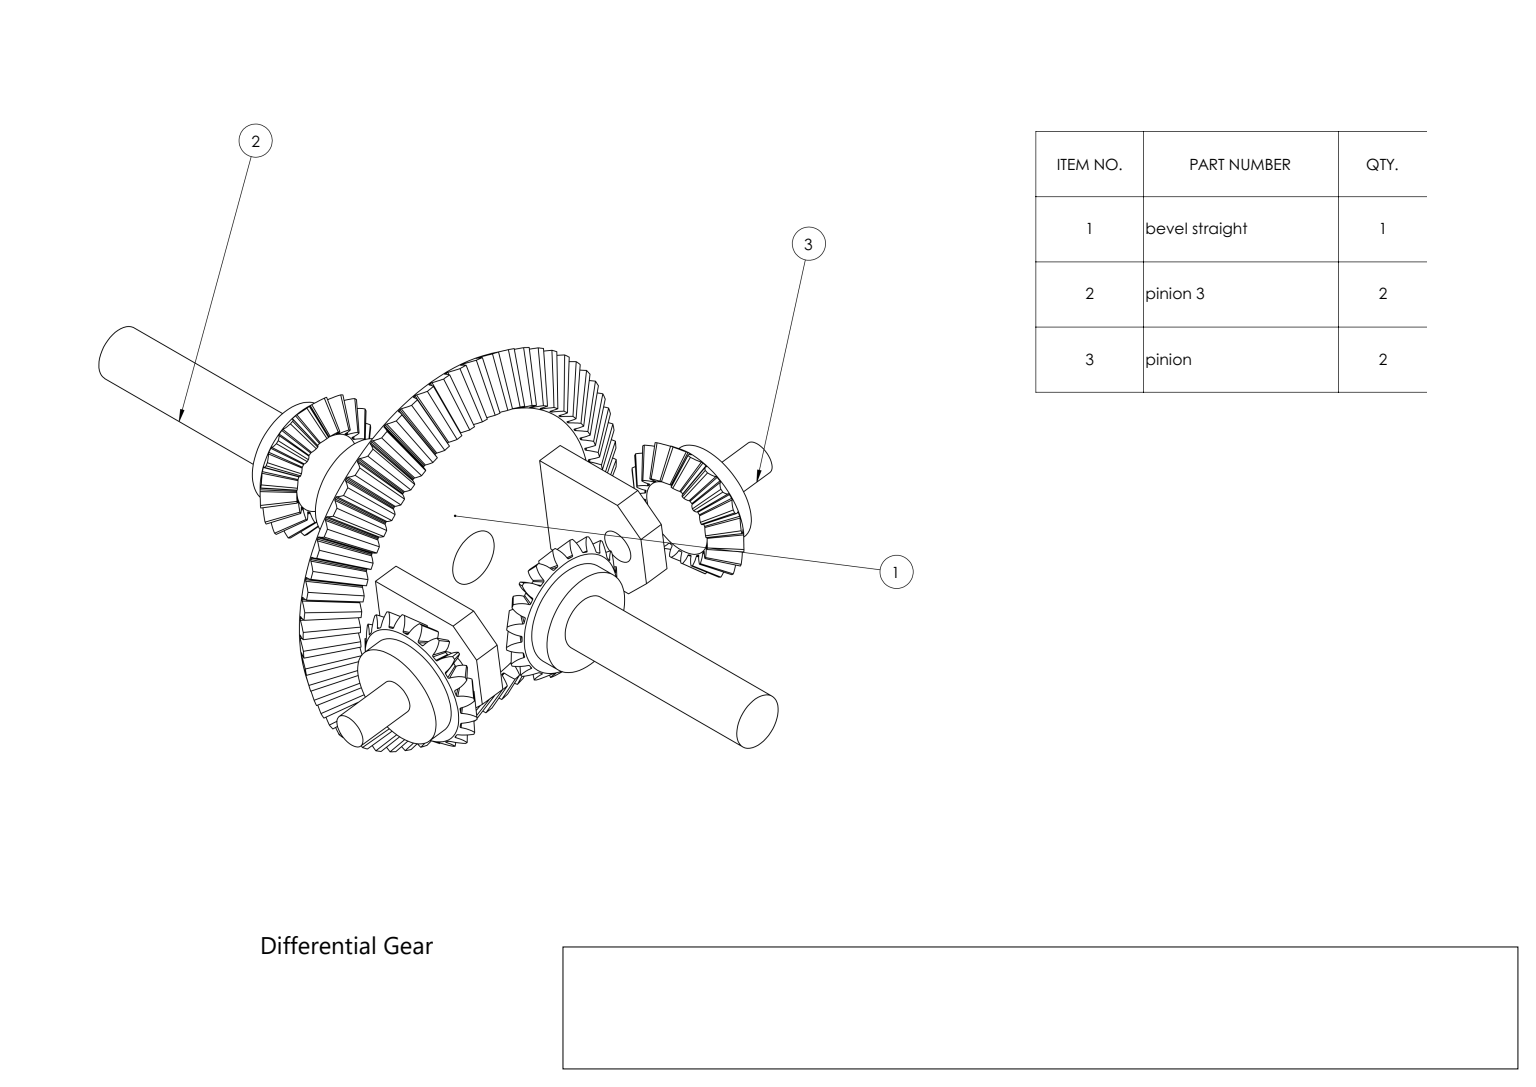
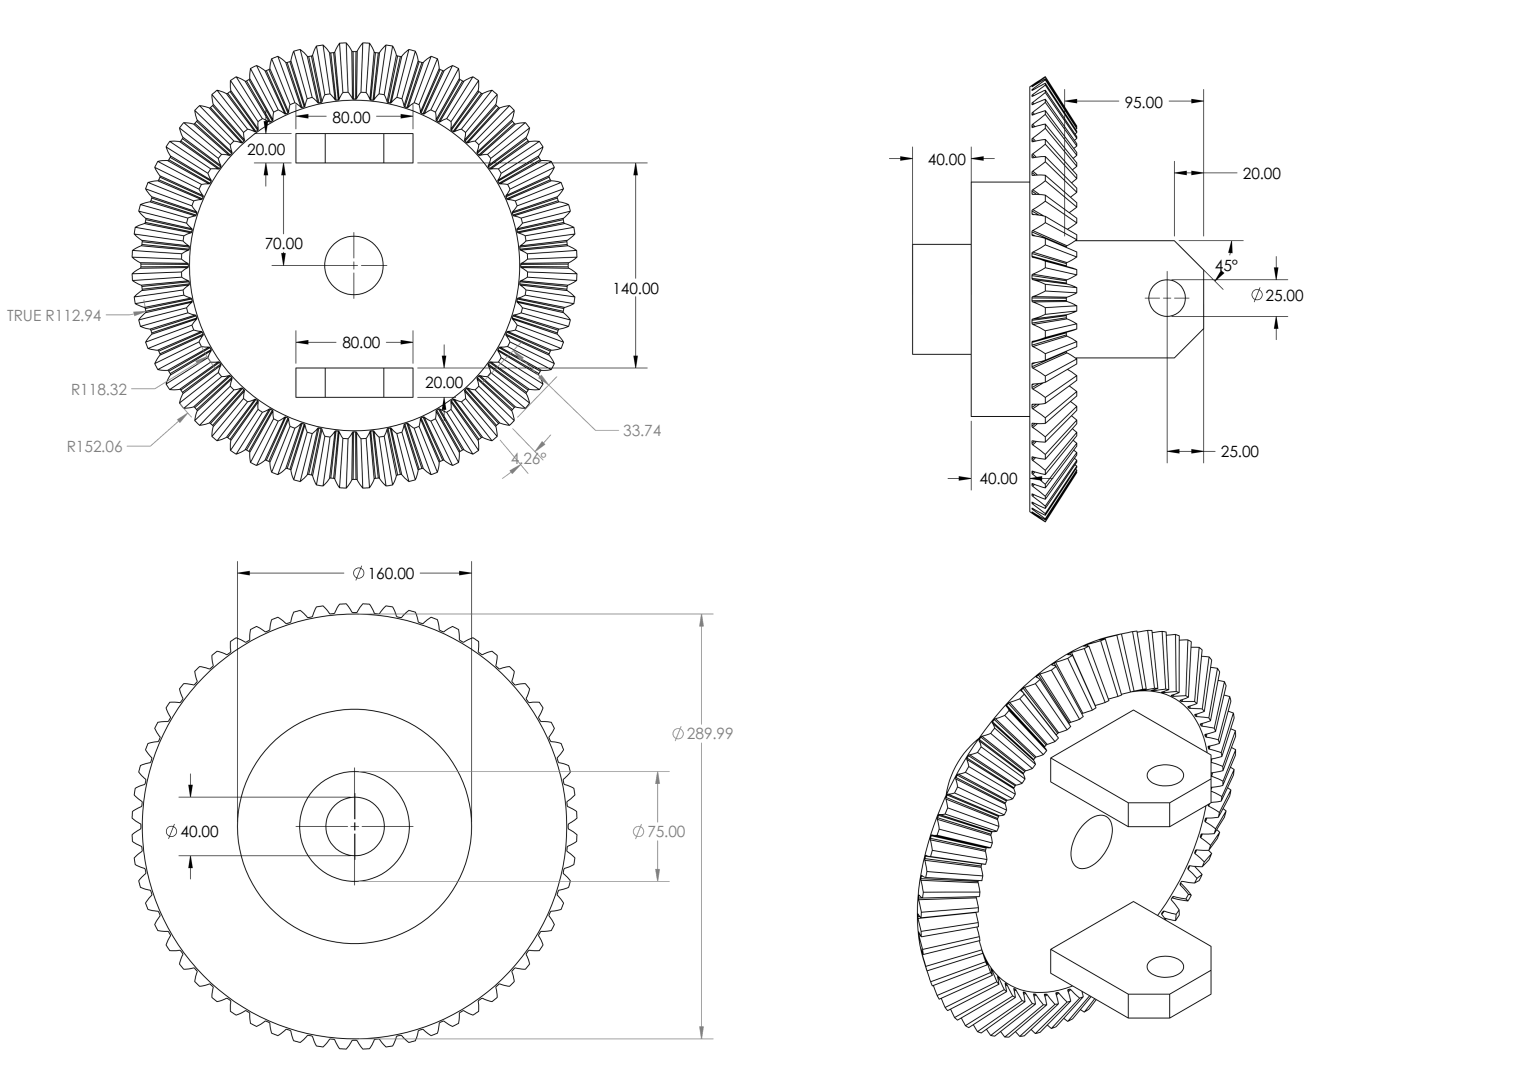
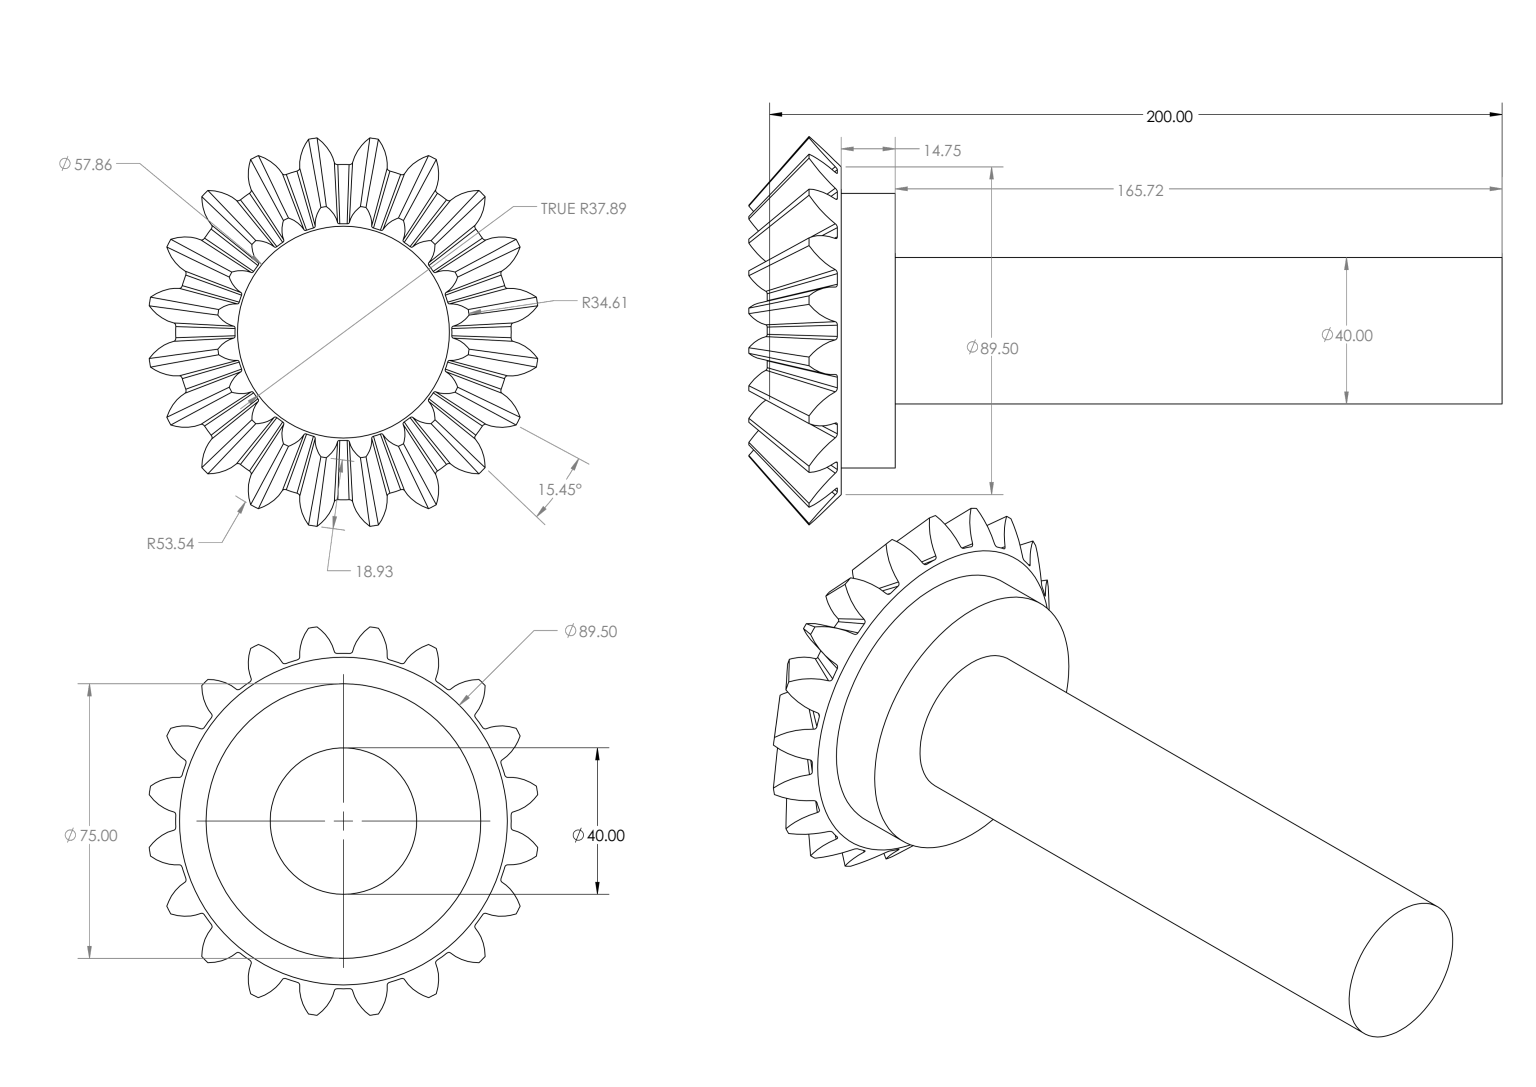
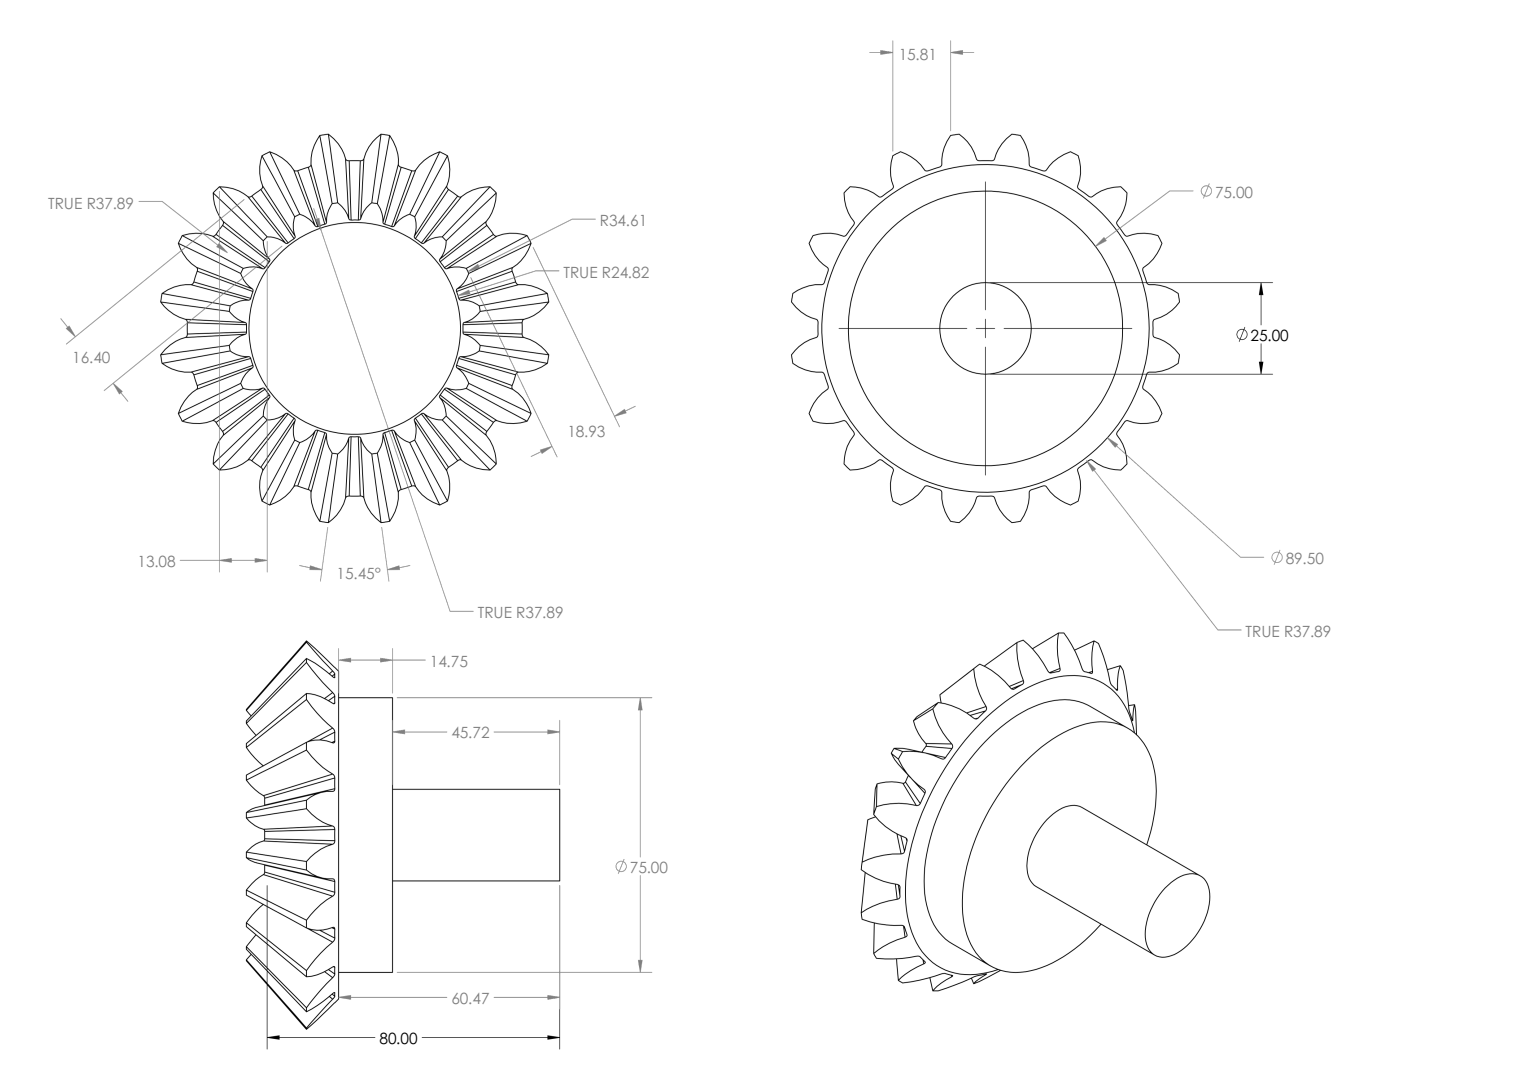
ISO-10303-21;
HEADER;
FILE_DESCRIPTION (('STEP AP214'),
    '1' );
FILE_NAME ('MAT-025',
    '2026-10-27T17:59:55',
    ( '' ),
    ( '' ),
    'SwSTEP 2.0',
    'SolidWorks 2025',
    '' );
FILE_SCHEMA (( 'AUTOMOTIVE_DESIGN' ));
ENDSEC;

DATA;
#1 = EDGE_LOOP ( 'NONE', ( #10472, #7018, #25272, #25137 ) ) ;
#2 = CARTESIAN_POINT ( 'NONE',  ( 1.833838850855486591, 72.47782099564645364, 125.7132320915350618 ) ) ;
#3 = CARTESIAN_POINT ( 'NONE',  ( -25.21435515916043713, -23.92354251275954979, -25.00736669481013053 ) ) ;
#4 = ORIENTED_EDGE ( 'NONE', *, *, #19841, .F. ) ;
#5 = CARTESIAN_POINT ( 'NONE',  ( 26.11404676487259024, 103.8885755249575453, -45.01677474591305383 ) ) ;
#6 = DIRECTION ( 'NONE',  ( -1.000000000000000000, 6.938893903907226837E-18, -1.734723475976806709E-18 ) ) ;
#7 = CARTESIAN_POINT ( 'NONE',  ( 1.833838850855486813, -44.75675607098831676, -138.0350826608191994 ) ) ;
#8 = LINE ( 'NONE', #19590, #21176 ) ;
#9 = CARTESIAN_POINT ( 'NONE',  ( -7.711401346138400115, 25.75361633141491424, -45.70592430511727144 ) ) ;
#10 = CARTESIAN_POINT ( 'NONE',  ( 1.833485406944043827, 96.69979900902318093, -108.1939177044916107 ) ) ;
#11 = CARTESIAN_POINT ( 'NONE',  ( -1.464342487929861214, -35.90631960086394514, 29.09292098541700611 ) ) ;
#12 = DIRECTION ( 'NONE',  ( -1.000000000000000000, -0.000000000000000000, -0.000000000000000000 ) ) ;
#13 = CARTESIAN_POINT ( 'NONE',  ( 1.834118845439484335, 107.9567937753806035, -96.96525081349894037 ) ) ;
#14 = CARTESIAN_POINT ( 'NONE',  ( -12.82751273423877514, -44.03362901246993744, 21.21958768041844579 ) ) ;
#15 = CARTESIAN_POINT ( 'NONE',  ( 2.433796855181219243, -43.58222566461740399, 138.8296532063086772 ) ) ;
#16 = CARTESIAN_POINT ( 'NONE',  ( 109.1721716018069657, 0.01157047143379281995, 0.01254847260354831351 ) ) ;
#17 = ORIENTED_EDGE ( 'NONE', *, *, #19645, .F. ) ;
#18 = EDGE_CURVE ( 'NONE', #18004, #25022, #27276, .T. ) ;
#19 = VERTEX_POINT ( 'NONE', #7434 ) ;
#20 = CARTESIAN_POINT ( 'NONE',  ( 1.833206308920067640, -126.0392061186627330, 71.90885838897354176 ) ) ;
#21 = CONICAL_SURFACE ( 'NONE', #3715, 34.60786435723138510, 0.8559913436420825139 ) ;
#22 = CARTESIAN_POINT ( 'NONE',  ( 32.73300124599738581, -32.68291970228155918, -113.0038235389605461 ) ) ;
#23 = VECTOR ( 'NONE', #27500, 1000.000000000000000 ) ;
#24 = EDGE_LOOP ( 'NONE', ( #16873, #10935, #10142, #25938 ) ) ;
#25 = VECTOR ( 'NONE', #23229, 1000.000000000000000 ) ;
#26 = VERTEX_POINT ( 'NONE', #9734 ) ;
#27 = EDGE_CURVE ( 'NONE', #15045, #24750, #18584, .T. ) ;
#28 = ORIENTED_EDGE ( 'NONE', *, *, #4351, .F. ) ;
#30 = AXIS2_PLACEMENT_3D ( 'NONE', #2388, #25118, #7714 ) ;
#29 =( BOUNDED_SURFACE ( )  B_SPLINE_SURFACE ( 3, 1, ( 
 ( #18833, #10616 ),
 ( #3858, #14509 ),
 ( #27599, #23743 ),
 ( #7922, #12623 ) ),
 .UNSPECIFIED., .F., .F., .F. ) 
 B_SPLINE_SURFACE_WITH_KNOTS ( ( 4, 4 ),
 ( 2, 2 ),
 ( 0.000000000000000000, 1.000000000000000000 ),
 ( 0.000000000000000000, 1.000000000000000000 ),
 .UNSPECIFIED. ) 
 GEOMETRIC_REPRESENTATION_ITEM ( )  RATIONAL_B_SPLINE_SURFACE ( (
 ( 1.000000000000000000, 1.000000000000000000),
 ( 0.9934239774497837239, 0.8357310067453919133),
 ( 0.9934239774497837239, 0.8357310067453919133),
 ( 1.000000000000000000, 1.000000000000000000) ) ) 
 REPRESENTATION_ITEM ( '' )  SURFACE ( )  );
#31 = EDGE_CURVE ( 'NONE', #25314, #21344, #6914, .T. ) ;
#32 = PRODUCT ( 'bevel straight', 'bevel straight', '', ( #7748 ) ) ;
#33 = CARTESIAN_POINT ( 'NONE',  ( 1.833838848569445235, 138.0625820091624689, 44.67212175381883554 ) ) ;
#34 = CARTESIAN_POINT ( 'NONE',  ( -1.019300379054419947, -44.15350047934390432, 12.21833869579511500 ) ) ;
#35 = B_SPLINE_CURVE_WITH_KNOTS ( 'NONE', 3,
 ( #6398, #19625, #8695, #17458, #4374, #21935, #7700, #20914, #16456, #5081 ),
 .UNSPECIFIED., .F., .F.,
 ( 4, 2, 2, 2, 4 ),
 ( 0.000000000000000000, 0.0003346267210630939765, 0.0006692534421261879529, 0.001003880163189281929, 0.001338506884252375906 ),
 .UNSPECIFIED. ) ;
#36 = CARTESIAN_POINT ( 'NONE',  ( -1.058197053496162887, -25.48582931365496762, -38.06270006878843759 ) ) ;
#37 = CARTESIAN_POINT ( 'NONE',  ( -20.57838717382308147, -16.28767523336102130, 25.16001208503123365 ) ) ;
#38 = CARTESIAN_POINT ( 'NONE',  ( 1.832998868059858122, 117.7096351258399238, -84.86110816369483700 ) ) ;
#39 = VECTOR ( 'NONE', #10071, 1000.000000000000000 ) ;
#40 = AXIS2_PLACEMENT_3D ( 'NONE', #19702, #25783, #12945 ) ;
#41 = CARTESIAN_POINT ( 'NONE',  ( -22.34422965417124374, 26.20925041532892763, 27.39717383755251490 ) ) ;
#42 = VECTOR ( 'NONE', #28114, 1000.000000000000000 ) ;
#43 = CARTESIAN_POINT ( 'NONE',  ( 25.64692872815576408, -110.5102270591924309, 23.16082795281220186 ) ) ;
#44 = CARTESIAN_POINT ( 'NONE',  ( -8.259864102781671491, -47.98931516265581365, 22.52209142944983711 ) ) ;
#45 = CARTESIAN_POINT ( 'NONE',  ( -1.050230346682696103, 37.05264119692688496, -26.91946103437118509 ) ) ;
#46 = CARTESIAN_POINT ( 'NONE',  ( 28.43349137099831836, 89.57679848841924297, -86.10800331998703427 ) ) ;
#47 = VECTOR ( 'NONE', #2248, 999.9999999999998863 ) ;
#48 = ORIENTED_EDGE ( 'NONE', *, *, #19991, .T. ) ;
#49 = ORIENTED_EDGE ( 'NONE', *, *, #17339, .T. ) ;
#51 = CARTESIAN_POINT ( 'NONE',  ( 5.340103556456315737, 133.7487107983443195, 62.06990747183722590 ) ) ;
#50 = DIRECTION ( 'NONE',  ( 0.000000000000000000, 5.223019709707975211E-21, -1.000000000000000000 ) ) ;
#52 = CARTESIAN_POINT ( 'NONE',  ( 2.433796855181233454, 109.1007109081226076, 96.28145139437721411 ) ) ;
#53 = CARTESIAN_POINT ( 'NONE',  ( 55.49584447822657296, -36.04376091928499903, -62.96491934286030556 ) ) ;
#54 = CARTESIAN_POINT ( 'NONE',  ( 32.73300124599741423, -75.82012867748416340, -89.94078864464141532 ) ) ;
#55 = CARTESIAN_POINT ( 'NONE',  ( -8.786685647604890903, -52.67761315067293282, -9.545808661480407409 ) ) ;
#56 = EDGE_LOOP ( 'NONE', ( #3504, #20915, #25986, #8058 ) ) ;
#57 = FACE_OUTER_BOUND ( 'NONE', #2614, .T. ) ;
#58 = EDGE_CURVE ( 'NONE', #28126, #17270, #1739, .T. ) ;
#59 = EDGE_LOOP ( 'NONE', ( #16364, #16288, #13278, #22767 ) ) ;
#60 = CARTESIAN_POINT ( 'NONE',  ( 2.108393763691174261, -144.3574619851891327, -16.46048390411948148 ) ) ;
#61 = FACE_OUTER_BOUND ( 'NONE', #13204, .T. ) ;
#62 = EDGE_LOOP ( 'NONE', ( #22452, #15366, #26764, #26750 ) ) ;
#63 = ORIENTED_EDGE ( 'NONE', *, *, #20098, .F. ) ;
#64 = ADVANCED_FACE ( 'NONE', ( #16053 ), #6020, .F. ) ;
#65 = CARTESIAN_POINT ( 'NONE',  ( 1.834118845439484335, 0.1779704863070283027, 145.1099497418795750 ) ) ;
#67 = ORIENTED_EDGE ( 'NONE', *, *, #11570, .T. ) ;
#66 = B_SPLINE_CURVE_WITH_KNOTS ( 'NONE', 3,
 ( #19256, #1821, #17232, #21839, #4133, #8326, #19665, #8599, #6307, #27897 ),
 .UNSPECIFIED., .F., .F.,
 ( 4, 3, 3, 4 ),
 ( 3.925231146709437917E-17, 0.0002669559177086131842, 0.0005339118354151096806, 0.001067817517169159696 ),
 .UNSPECIFIED. ) ;
#68 = CARTESIAN_POINT ( 'NONE',  ( 6.224689322667647851, -43.30635742325475945, 141.5842213414011894 ) ) ;
#69 = ORIENTED_EDGE ( 'NONE', *, *, #25818, .T. ) ;
#70 = EDGE_CURVE ( 'NONE', #24626, #27978, #23754, .T. ) ;
#71 = VECTOR ( 'NONE', #18224, 1000.000000000000114 ) ;
#72 =( GEOMETRIC_REPRESENTATION_CONTEXT ( 3 ) GLOBAL_UNCERTAINTY_ASSIGNED_CONTEXT ( ( #16000 ) ) GLOBAL_UNIT_ASSIGNED_CONTEXT ( ( #25277, #3392, #1644 ) ) REPRESENTATION_CONTEXT ( 'NONE', 'WORKASPACE' ) );
#73 = CARTESIAN_POINT ( 'NONE',  ( 1.833485406944057594, 97.49333871408690300, 107.4794113447412940 ) ) ;
#74 = EDGE_CURVE ( 'NONE', #7427, #22997, #15851, .T. ) ;
#75 = VECTOR ( 'NONE', #20368, 1000.000000000000000 ) ;
#76 = ORIENTED_EDGE ( 'NONE', *, *, #10432, .T. ) ;
#77 =( BOUNDED_SURFACE ( )  B_SPLINE_SURFACE ( 3, 1, ( 
 ( #18368, #537 ),
 ( #2696, #7179 ),
 ( #16223, #3130 ),
 ( #25029, #14055 ) ),
 .UNSPECIFIED., .F., .F., .F. ) 
 B_SPLINE_SURFACE_WITH_KNOTS ( ( 4, 4 ),
 ( 2, 2 ),
 ( 0.000000000000000000, 1.000000000000000000 ),
 ( 0.000000000000000000, 1.000000000000000000 ),
 .UNSPECIFIED. ) 
 GEOMETRIC_REPRESENTATION_ITEM ( )  RATIONAL_B_SPLINE_SURFACE ( (
 ( 1.000000000000000000, 1.000000000000000000),
 ( 0.7789835883360576307, 0.9689951854195403280),
 ( 0.7789835883360576307, 0.9689951854195403280),
 ( 1.000000000000000000, 1.000000000000000000) ) ) 
 REPRESENTATION_ITEM ( '' )  SURFACE ( )  );
#78 = CARTESIAN_POINT ( 'NONE',  ( 32.73300124599738581, -55.46353551261936587, -103.7392577722181812 ) ) ;
#79 = CARTESIAN_POINT ( 'NONE',  ( 2.430230287190589422, 13.76600171652836302, -144.8619874886005334 ) ) ;
#80 = CARTESIAN_POINT ( 'NONE',  ( 25.86096068574580897, 55.66087367585407009, 98.40249579084530751 ) ) ;
#81 = CARTESIAN_POINT ( 'NONE',  ( 10.93730112725972070, -4.928439153521261495, 151.0983828010090804 ) ) ;
#82 = B_SPLINE_CURVE_WITH_KNOTS ( 'NONE', 3,
 ( #16407, #22468, #25063, #2733, #11511, #18128 ),
 .UNSPECIFIED., .F., .F.,
 ( 4, 2, 4 ),
 ( 4.906538933386797396E-18, 0.0004335151646191543395, 0.0008670303292383036917 ),
 .UNSPECIFIED. ) ;
#83 = CARTESIAN_POINT ( 'NONE',  ( -1.583189561560256253, 11.94859433442902130, -44.83405390829675952 ) ) ;
#84 = FACE_OUTER_BOUND ( 'NONE', #26105, .T. ) ;
#85 = B_SPLINE_CURVE_WITH_KNOTS ( 'NONE', 3,
 ( #11291, #16435, #20350, #18180, #12122, #2499 ),
 .UNSPECIFIED., .F., .F.,
 ( 4, 2, 4 ),
 ( 3.525929482785130599E-16, 0.003576372551511158761, 0.007152745103021965374 ),
 .UNSPECIFIED. ) ;
#86 = CARTESIAN_POINT ( 'NONE',  ( 25.64681081121879203, -56.81519825470687834, -97.57530875170664331 ) ) ;
#87 = CARTESIAN_POINT ( 'NONE',  ( -24.53237795827004319, 33.71192251888839309, -3.868415699415555853 ) ) ;
#88 = CARTESIAN_POINT ( 'NONE',  ( 1.833206310202335487, 125.2945016693821572, -73.19872434058655131 ) ) ;
#89 = CARTESIAN_POINT ( 'NONE',  ( 28.37644542392839853, 115.1790646972555550, -46.84227702240664826 ) ) ;
#90 = DIRECTION ( 'NONE',  ( -0.5946245182733607137, 0.2512550613902174712, 0.7637359336799413034 ) ) ;
#91 = ORIENTED_EDGE ( 'NONE', *, *, #18115, .F. ) ;
#92 = CONICAL_SURFACE ( 'NONE', #10236, 117.6351876552689504, 0.9945805576725580410 ) ;
#93 = CARTESIAN_POINT ( 'NONE',  ( -25.21435515916043713, -34.05351380035337883, -6.169479169075319014 ) ) ;
#94 = CARTESIAN_POINT ( 'NONE',  ( 55.79472521941428198, -54.55111121764050353, -48.13855120843939517 ) ) ;
#95 = CARTESIAN_POINT ( 'NONE',  ( 30.58324630866339433, 67.85993782330898227, -100.1119227962713580 ) ) ;
#96 = EDGE_CURVE ( 'NONE', #11003, #17556, #6371, .T. ) ;
#97 = EDGE_LOOP ( 'NONE', ( #15926, #16768, #23788, #24002 ) ) ;
#98 = CARTESIAN_POINT ( 'NONE',  ( -55.24390624410018802, 0.009374879212967415429, 0.004572280736702902422 ) ) ;
#99 = EDGE_CURVE ( 'NONE', #10555, #9765, #28256, .T. ) ;
#100 = CARTESIAN_POINT ( 'NONE',  ( 25.64681081121879203, 84.18689316040048709, 75.24277141833519522 ) ) ;
#101 = ORIENTED_EDGE ( 'NONE', *, *, #24597, .T. ) ;
#102 = CARTESIAN_POINT ( 'NONE',  ( 25.64708228042119131, -112.9112740241347410, -0.03938584558111280637 ) ) ;
#103 = CARTESIAN_POINT ( 'NONE',  ( 55.49584447822657296, 29.75369869231044007, -66.16986612640745591 ) ) ;
#104 = AXIS2_PLACEMENT_3D ( 'NONE', #10529, #19295, #19436 ) ;
#105 = CARTESIAN_POINT ( 'NONE',  ( 10.93730112725932813, 150.7858122213658305, 10.89264110825069132 ) ) ;
#106 = VERTEX_POINT ( 'NONE', #1511 ) ;
#107 = CARTESIAN_POINT ( 'NONE',  ( -55.24390624410018802, -0.007245494385991085341, 0.007503127514277716827 ) ) ;
#108 = CIRCLE ( 'NONE', #9760, 53.53553390275978785 ) ;
#109 = CARTESIAN_POINT ( 'NONE',  ( -1.464342487929870096, 35.90631960086420094, -29.09292098541673965 ) ) ;
#110 = AXIS2_PLACEMENT_3D ( 'NONE', #20120, #552, #11348 ) ;
#111 = CARTESIAN_POINT ( 'NONE',  ( 28.37599760073042532, -10.20682761621855050, -114.2774414139536105 ) ) ;
#112 = DIRECTION ( 'NONE',  ( 0.5914120900931443270, 0.7870418015781034393, 0.1754905759872925630 ) ) ;
#113 = CARTESIAN_POINT ( 'NONE',  ( -25.21435515916043357, 16.39063784838743132, -30.48034229288645136 ) ) ;
#114 = CARTESIAN_POINT ( 'NONE',  ( 2.433796855181219243, -126.7346379669260443, 71.49415740225030902 ) ) ;
#115 = EDGE_LOOP ( 'NONE', ( #6839, #637, #24909, #28009 ) ) ;
#116 = CARTESIAN_POINT ( 'NONE',  ( 26.11404676487259024, -92.25884714080363835, -65.63269960453335727 ) ) ;
#117 = CARTESIAN_POINT ( 'NONE',  ( -16.86833981943422600, -7.884812276281804699, 43.51541671545733436 ) ) ;
#118 = CARTESIAN_POINT ( 'NONE',  ( -40.00000000000000000, 4.592425496802575944E-15, 37.50000000000002132 ) ) ;
#119 = VERTEX_POINT ( 'NONE', #8423 ) ;
#120 = ORIENTED_EDGE ( 'NONE', *, *, #24125, .T. ) ;
#121 = ORIENTED_EDGE ( 'NONE', *, *, #10704, .F. ) ;
#122 = ORIENTED_EDGE ( 'NONE', *, *, #1235, .F. ) ;
#123 = CARTESIAN_POINT ( 'NONE',  ( -1.048996300304493312, -27.53442103413720332, -36.59642367107734628 ) ) ;
#124 = CARTESIAN_POINT ( 'NONE',  ( -28.13707043255157103, -6.342158660426852279, 22.00298671236746273 ) ) ;
#125 = CARTESIAN_POINT ( 'NONE',  ( 25.64704443564079028, 75.45310550990150489, 83.99864088993793132 ) ) ;
#126 = CARTESIAN_POINT ( 'NONE',  ( 2.430230287190589422, 60.50928654924753403, 132.3371620660953170 ) ) ;
#127 = CARTESIAN_POINT ( 'NONE',  ( 25.64681081121879203, -103.3177883989782657, 45.54494737132187510 ) ) ;
#128 = CARTESIAN_POINT ( 'NONE',  ( 25.98552792386802324, 47.00040718953771801, 102.9121737515621930 ) ) ;
#129 = ORIENTED_EDGE ( 'NONE', *, *, #24590, .F. ) ;
#130 = CARTESIAN_POINT ( 'NONE',  ( -4.178947244162636743, 48.81675275154077553, -3.367451375481286036 ) ) ;
#131 = CARTESIAN_POINT ( 'NONE',  ( -23.79248802219731118, 28.61009539422409631, 16.82188324679449565 ) ) ;
#132 = CARTESIAN_POINT ( 'NONE',  ( -1.050229599974486616, -36.90196321294315140, -27.12684363859242254 ) ) ;
#133 = CARTESIAN_POINT ( 'NONE',  ( 25.70243777736188306, -112.9457924277214431, -0.7331659071607105060 ) ) ;
#134 = LINE ( 'NONE', #9062, #397 ) ;
#135 = EDGE_CURVE ( 'NONE', #16438, #8336, #27522, .T. ) ;
#136 = CARTESIAN_POINT ( 'NONE',  ( -8.259864102781710571, 46.42816643551610412, 25.58601832199028436 ) ) ;
#137 = VECTOR ( 'NONE', #20030, 1000.000000000000114 ) ;
#138 = CIRCLE ( 'NONE', #7979, 34.60786435723138510 ) ;
#139 = CARTESIAN_POINT ( 'NONE',  ( 1.833485406944043827, -107.4794113447415924, 97.49333871408656194 ) ) ;
#140 = EDGE_CURVE ( 'NONE', #22201, #4550, #16497, .T. ) ;
#141 = CARTESIAN_POINT ( 'NONE',  ( 25.64704443564077252, -56.33997466860336090, -97.85065179540814029 ) ) ;
#142 = VERTEX_POINT ( 'NONE', #25977 ) ;
#143 = B_SPLINE_CURVE_WITH_KNOTS ( 'NONE', 3,
 ( #16043, #26973, #20213, #20507, #7279, #22545, #24997 ),
 .UNSPECIFIED., .F., .F.,
 ( 4, 3, 4 ),
 ( 1.105886215935214523E-17, 0.0007657099931970557912, 0.001530725384384964971 ),
 .UNSPECIFIED. ) ;
#144 = EDGE_CURVE ( 'NONE', #16046, #25406, #13445, .T. ) ;
#145 = ORIENTED_EDGE ( 'NONE', *, *, #25140, .T. ) ;
#146 = ORIENTED_EDGE ( 'NONE', *, *, #20602, .T. ) ;
#147 = CARTESIAN_POINT ( 'NONE',  ( -1.056502255334264895, 45.80535052436397336, -0.5104472526221494055 ) ) ;
#148 = CARTESIAN_POINT ( 'NONE',  ( 2.430230287190592531, 125.2872625092172569, -74.01081053030968349 ) ) ;
#149 = DIRECTION ( 'NONE',  ( 0.000000000000000000, 0.000000000000000000, 1.000000000000000000 ) ) ;
#150 = EDGE_LOOP ( 'NONE', ( #7208, #20367, #2015, #26988 ) ) ;
#151 = CARTESIAN_POINT ( 'NONE',  ( -55.25297051322618813, 0.007247191603129411047, -0.01306918787467283537 ) ) ;
#152 = CONICAL_SURFACE ( 'NONE', #15759, 111.9614997405030152, 0.5880026024245678107 ) ;
#153 = EDGE_CURVE ( 'NONE', #12676, #6634, #10682, .T. ) ;
#154 = AXIS2_PLACEMENT_3D ( 'NONE', #16528, #25317, #5594 ) ;
#155 = CARTESIAN_POINT ( 'NONE',  ( -1.583189561560253589, 36.01941156322789084, -29.24830400313178558 ) ) ;
#156 = ORIENTED_EDGE ( 'NONE', *, *, #10565, .F. ) ;
#157 = CARTESIAN_POINT ( 'NONE',  ( 26.04756280548352265, 92.21166514879097065, 65.62256188141753910 ) ) ;
#158 = ORIENTED_EDGE ( 'NONE', *, *, #12725, .F. ) ;
#159 = CARTESIAN_POINT ( 'NONE',  ( 60.46576798286869803, -4.195655488513964285E-16, 1.048913872128491071E-16 ) ) ;
#160 = CARTESIAN_POINT ( 'NONE',  ( -1.583189561560256253, -2.490696082060189109, -46.33203782964460515 ) ) ;
#161 = CARTESIAN_POINT ( 'NONE',  ( -1.031422197589716205, -43.06660437151298026, 15.60268798220682562 ) ) ;
#162 = CARTESIAN_POINT ( 'NONE',  ( 1.894214914920957282, 73.39939580274932496, 125.2241265685472769 ) ) ;
#163 = LINE ( 'NONE', #11103, #42 ) ;
#164 = ADVANCED_FACE ( 'NONE', ( #4090 ), #17761, .F. ) ;
#165 = CARTESIAN_POINT ( 'NONE',  ( -55.25719721206881729, -0.004044147484877910065, -0.01041086141212526316 ) ) ;
#166 = EDGE_CURVE ( 'NONE', #18597, #20724, #3825, .T. ) ;
#167 = DIRECTION ( 'NONE',  ( 0.7563875759206388771, -0.1685564395263385584, -0.6320336713238493553 ) ) ;
#168 = CARTESIAN_POINT ( 'NONE',  ( -20.24419206586953379, -24.70913649113841970, -16.36655224501358319 ) ) ;
#169 = B_SPLINE_CURVE_WITH_KNOTS ( 'NONE', 3,
 ( #9089, #24504, #26632, #13540, #23032, #14, #6943 ),
 .UNSPECIFIED., .F., .F.,
 ( 4, 3, 4 ),
 ( 0.000000000000000000, 0.006568092053401781462, 0.02506242213020847681 ),
 .UNSPECIFIED. ) ;
#170 = CARTESIAN_POINT ( 'NONE',  ( -22.23226125620943705, 29.33577758406451252, -11.82389163795220455 ) ) ;
#171 = ADVANCED_FACE ( 'NONE', ( #3953 ), #26753, .F. ) ;
#172 = CARTESIAN_POINT ( 'NONE',  ( 109.1778270068192853, 0.008960903982066559248, 0.002542344697966475615 ) ) ;
#173 = ORIENTED_EDGE ( 'NONE', *, *, #8292, .T. ) ;
#174 = VERTEX_POINT ( 'NONE', #332 ) ;
#175 = CARTESIAN_POINT ( 'NONE',  ( 2.433796855181219243, -126.7346379669260443, 71.49415740225030902 ) ) ;
#176 = FACE_OUTER_BOUND ( 'NONE', #3047, .T. ) ;
#177 = ORIENTED_EDGE ( 'NONE', *, *, #10269, .T. ) ;
#178 = EDGE_LOOP ( 'NONE', ( #3906, #2305, #10108, #5522 ) ) ;
#179 = ORIENTED_EDGE ( 'NONE', *, *, #12730, .F. ) ;
#180 = CARTESIAN_POINT ( 'NONE',  ( 30.59141879584279877, 84.53180090073671238, 79.74795589902048221 ) ) ;
#181 = CARTESIAN_POINT ( 'NONE',  ( 109.1587776205901577, 0.005880209827416989048, 0.004375189885414189697 ) ) ;
#182 = VERTEX_POINT ( 'NONE', #2340 ) ;
#183 = FACE_OUTER_BOUND ( 'NONE', #401, .T. ) ;
#184 = CARTESIAN_POINT ( 'NONE',  ( 109.1589550718174877, 0.006826119083824074701, 0.003284595046925682486 ) ) ;
#185 = CARTESIAN_POINT ( 'NONE',  ( 1.831572820252008738, -142.1425225354581983, 29.20415387690522024 ) ) ;
#186 = CARTESIAN_POINT ( 'NONE',  ( -20.90916690077964191, 34.84883504600978910, 18.74041620980130674 ) ) ;
#187 = CARTESIAN_POINT ( 'NONE',  ( 30.59138290137883232, -92.40465044710784071, 70.47507990428522362 ) ) ;
#188 = CARTESIAN_POINT ( 'NONE',  ( 109.1592201516379674, 0.007051465909551715011, 0.003476928926125415296 ) ) ;
#189 = EDGE_CURVE ( 'NONE', #8031, #1001, #28395, .T. ) ;
#190 = CARTESIAN_POINT ( 'NONE',  ( 16.05277956358205316, -121.7045645913023293, 75.66118899150477262 ) ) ;
#191 = CARTESIAN_POINT ( 'NONE',  ( -55.25297051322618813, -0.01483298743815008106, -0.001818774723749387676 ) ) ;
#192 = CARTESIAN_POINT ( 'NONE',  ( 1.833485406944057594, -117.0814567582550154, 85.72460230293657446 ) ) ;
#193 = EDGE_CURVE ( 'NONE', #16027, #27728, #13099, .T. ) ;
#194 = VERTEX_POINT ( 'NONE', #11141 ) ;
#195 = VERTEX_POINT ( 'NONE', #19915 ) ;
#197 = CARTESIAN_POINT ( 'NONE',  ( -55.24728320129491266, 0.005114031043466756021, 0.01362040845703047127 ) ) ;
#196 = CARTESIAN_POINT ( 'NONE',  ( 2.433796855181219243, -145.5024947199069913, 1.451562450949123395 ) ) ;
#198 = CARTESIAN_POINT ( 'NONE',  ( 2.433796855181205476, 137.9325382748285165, 46.34326152018790168 ) ) ;
#199 = CARTESIAN_POINT ( 'NONE',  ( -1.323830074806772839, 38.58891736138533446, -25.17121255494489418 ) ) ;
#200 = CARTESIAN_POINT ( 'NONE',  ( 25.64681081121879203, 0.4157506337743640534, -112.9102952884414464 ) ) ;
#201 = CARTESIAN_POINT ( 'NONE',  ( 32.73300124599733607, 103.7392577722176270, 55.46353551262048853 ) ) ;
#202 = ORIENTED_EDGE ( 'NONE', *, *, #27365, .T. ) ;
#203 = CARTESIAN_POINT ( 'NONE',  ( -55.24300891470650754, -0.002702093572892964434, 0.009439835024158798812 ) ) ;
#204 = ORIENTED_EDGE ( 'NONE', *, *, #22614, .T. ) ;
#205 = CARTESIAN_POINT ( 'NONE',  ( -1.046936909428695328, 43.14407378092994350, -15.35929614323679893 ) ) ;
#206 = CARTESIAN_POINT ( 'NONE',  ( -25.21435515916043713, -4.655591116594118617, 34.29329011225960500 ) ) ;
#207 = VERTEX_POINT ( 'NONE', #201 ) ;
#208 = ORIENTED_EDGE ( 'NONE', *, *, #15962, .F. ) ;
#209 = B_SPLINE_CURVE_WITH_KNOTS ( 'NONE', 3,
 ( #19495, #4231, #17048, #26252, #19767, #28124, #6140, #6547 ),
 .UNSPECIFIED., .F., .F.,
 ( 4, 2, 2, 4 ),
 ( 0.000000000000000000, 0.002761524886576660620, 0.005523049773153321240, 0.01104609954630662513 ),
 .UNSPECIFIED. ) ;
#210 = CARTESIAN_POINT ( 'NONE',  ( -55.24198130335446422, -0.004276389980779660843, 0.008252882783648829434 ) ) ;
#211 = VERTEX_POINT ( 'NONE', #55 ) ;
#212 = CARTESIAN_POINT ( 'NONE',  ( 32.73300124599732186, 0.000000000000000000, 0.000000000000000000 ) ) ;
#213 = VERTEX_POINT ( 'NONE', #26527 ) ;
#214 = CARTESIAN_POINT ( 'NONE',  ( -19.53423201713129842, 3.678323623448370869E-15, -28.92774122539760384 ) ) ;
#215 = ORIENTED_EDGE ( 'NONE', *, *, #19681, .F. ) ;
#216 = CARTESIAN_POINT ( 'NONE',  ( 19.66333377628698997, 133.7337774475000458, 33.01772659807154753 ) ) ;
#217 = CARTESIAN_POINT ( 'NONE',  ( -1.050230346682673677, -14.15203301556463167, -43.55772679531845881 ) ) ;
#218 = CARTESIAN_POINT ( 'NONE',  ( 109.1778270068192853, -0.008743876326162617132, 0.003210287141653769046 ) ) ;
#219 = EDGE_CURVE ( 'NONE', #10856, #1807, #18227, .T. ) ;
#220 = CARTESIAN_POINT ( 'NONE',  ( -21.41427618760446450, 1.815001260755841450, -30.75468365310879193 ) ) ;
#221 = CARTESIAN_POINT ( 'NONE',  ( -1.031422197589711764, 45.78027046666443312, 1.530725436377622817 ) ) ;
#222 = CARTESIAN_POINT ( 'NONE',  ( 10.93730112725969938, 79.81734490845904872, 128.3908183996593948 ) ) ;
#223 = EDGE_CURVE ( 'NONE', #27632, #18732, #6944, .T. ) ;
#224 = CARTESIAN_POINT ( 'NONE',  ( -22.23342874802669655, -24.24669006619387090, -20.31166691703116811 ) ) ;
#225 = CARTESIAN_POINT ( 'NONE',  ( -55.24390624410018802, 0.009374879212967415429, 0.004572280736702902422 ) ) ;
#226 = EDGE_CURVE ( 'NONE', #4538, #24427, #4523, .T. ) ;
#227 = ORIENTED_EDGE ( 'NONE', *, *, #10953, .F. ) ;
#228 = CARTESIAN_POINT ( 'NONE',  ( 109.1587776205901861, -0.006661366261223573317, 0.003057017121600521300 ) ) ;
#229 = CARTESIAN_POINT ( 'NONE',  ( 32.73300124599732186, 0.000000000000000000, 0.000000000000000000 ) ) ;
#230 = CARTESIAN_POINT ( 'NONE',  ( -2.904412668506678674, -47.56768199507435213, -2.864640348250463653 ) ) ;
#231 = CARTESIAN_POINT ( 'NONE',  ( -20.20700224038492721, -27.82980252387812570, 10.08426345511618649 ) ) ;
#232 = EDGE_CURVE ( 'NONE', #4316, #25484, #25242, .T. ) ;
#233 = ORIENTED_EDGE ( 'NONE', *, *, #28355, .F. ) ;
#234 = CARTESIAN_POINT ( 'NONE',  ( -1.044557008772713180, 15.70482370518816495, -43.01636061108991527 ) ) ;
#235 = CARTESIAN_POINT ( 'NONE',  ( 32.73300124599738581, -44.31599526637883457, -108.9684813982493097 ) ) ;
#236 = CARTESIAN_POINT ( 'NONE',  ( 26.11404676487256893, -92.25884714080449100, 65.63269960453210672 ) ) ;
#237 = DIRECTION ( 'NONE',  ( -0.5914120900931443270, -0.7333565075147377987, 0.3352908775637131744 ) ) ;
#238 = VERTEX_POINT ( 'NONE', #2060 ) ;
#239 = CARTESIAN_POINT ( 'NONE',  ( -55.25297051322618813, -0.01466904165775489814, 0.002853887643043841529 ) ) ;
#240 = CARTESIAN_POINT ( 'NONE',  ( 13.36082413113063083, -70.90215303572219341, 135.4964217943305016 ) ) ;
#241 = CARTESIAN_POINT ( 'NONE',  ( -23.79248802219723302, -33.03370827286728684, 3.207402715357496881 ) ) ;
#242 =( BOUNDED_SURFACE ( )  B_SPLINE_SURFACE ( 3, 1, ( 
 ( #18082, #26857 ),
 ( #7167, #25021 ),
 ( #5274, #14047 ),
 ( #19092, #12595 ) ),
 .UNSPECIFIED., .F., .F., .F. ) 
 B_SPLINE_SURFACE_WITH_KNOTS ( ( 4, 4 ),
 ( 2, 2 ),
 ( 0.000000000000000000, 1.000000000000000000 ),
 ( 0.000000000000000000, 1.000000000000000000 ),
 .UNSPECIFIED. ) 
 GEOMETRIC_REPRESENTATION_ITEM ( )  RATIONAL_B_SPLINE_SURFACE ( (
 ( 1.000000000000000000, 1.000000000000000000),
 ( 0.6386103224230316178, 0.9954351624131538845),
 ( 0.6386103224230316178, 0.9954351624131538845),
 ( 1.000000000000000000, 1.000000000000000000) ) ) 
 REPRESENTATION_ITEM ( '' )  SURFACE ( )  );
#243 = VERTEX_POINT ( 'NONE', #11283 ) ;
#244 = CARTESIAN_POINT ( 'NONE',  ( -7.078251931573406708, -11.16394717458641850, 50.86685171665422445 ) ) ;
#245 = B_SPLINE_CURVE_WITH_KNOTS ( 'NONE', 3,
 ( #3724, #1420, #27900, #10365, #12769, #28028 ),
 .UNSPECIFIED., .F., .F.,
 ( 4, 2, 4 ),
 ( 0.000000000000000000, 0.0006311571484585922365, 0.001262314296917184473 ),
 .UNSPECIFIED. ) ;
#246 = VERTEX_POINT ( 'NONE', #20051 ) ;
#247 = CARTESIAN_POINT ( 'NONE',  ( 25.64692872815577829, 103.2799065540890524, -45.63107645358226705 ) ) ;
#248 = CARTESIAN_POINT ( 'NONE',  ( 13.84597867724968090, -129.3717503931856641, 69.17016226639006504 ) ) ;
#249 = CARTESIAN_POINT ( 'NONE',  ( -20.20700224038492010, -16.58740185276728241, -24.51628800869040958 ) ) ;
#250 = CARTESIAN_POINT ( 'NONE',  ( -20.47566338032515532, 28.85746366088581283, 7.708089572830123082 ) ) ;
#251 = FACE_OUTER_BOUND ( 'NONE', #25592, .T. ) ;
#252 = CARTESIAN_POINT ( 'NONE',  ( 32.73300124599732897, 117.3295799645430151, 8.473903470906510194 ) ) ;
#253 = EDGE_CURVE ( 'NONE', #19163, #21576, #4177, .T. ) ;
#254 = ORIENTED_EDGE ( 'NONE', *, *, #9034, .T. ) ;
#255 = B_SPLINE_CURVE_WITH_KNOTS ( 'NONE', 3,
 ( #24853, #22407, #7154, #15914, #800, #7433, #27419 ),
 .UNSPECIFIED., .F., .F.,
 ( 4, 3, 4 ),
 ( 0.000000000000000000, 0.006568092053401802279, 0.02506242213020847681 ),
 .UNSPECIFIED. ) ;
#256 = CARTESIAN_POINT ( 'NONE',  ( 109.1721716018069515, -0.01392660302850065417, 0.009868622090669508864 ) ) ;
#257 = CARTESIAN_POINT ( 'NONE',  ( 25.64681081121879203, 34.49579773461926635, -107.5125461021399218 ) ) ;
#258 = CARTESIAN_POINT ( 'NONE',  ( -20.21097721650786738, 29.61001326827675939, -0.3305964462498667822 ) ) ;
#259 = CARTESIAN_POINT ( 'NONE',  ( 32.73300124599741423, 114.2056417606551406, -28.19767303745493336 ) ) ;
#260 = ORIENTED_EDGE ( 'NONE', *, *, #18337, .F. ) ;
#261 = EDGE_CURVE ( 'NONE', #22201, #20516, #2798, .T. ) ;
#262 = ORIENTED_EDGE ( 'NONE', *, *, #7996, .F. ) ;
#263 = ORIENTED_EDGE ( 'NONE', *, *, #15518, .T. ) ;
#264 = CARTESIAN_POINT ( 'NONE',  ( -1.048171036023509917, -26.08692787913895472, -37.64178826568597458 ) ) ;
#265 = CARTESIAN_POINT ( 'NONE',  ( -1.019300379054419947, 45.76814864815091255, 2.023851374322834573 ) ) ;
#266 = CARTESIAN_POINT ( 'NONE',  ( -1.539763995773682614, -38.84665165401045073, 25.17088606276588791 ) ) ;
#267 = CARTESIAN_POINT ( 'NONE',  ( -1.048171036023513247, 1.020520027229132598, -45.78635789057864969 ) ) ;
#268 = CARTESIAN_POINT ( 'NONE',  ( 1.833838848569428581, 72.40075357737826778, -125.7577269771224735 ) ) ;
#269 = FACE_OUTER_BOUND ( 'NONE', #11940, .T. ) ;
#270 = ORIENTED_EDGE ( 'NONE', *, *, #4191, .F. ) ;
#271 = CARTESIAN_POINT ( 'NONE',  ( -55.24198130335446422, 0.008252882783649323831, 0.004276389980779915848 ) ) ;
#272 = CARTESIAN_POINT ( 'NONE',  ( 1.893872463202044054, -58.16604752596636274, -132.9857054814986554 ) ) ;
#273 = CARTESIAN_POINT ( 'NONE',  ( 2.430230287190572103, 144.8619874886008745, -13.76600171652493998 ) ) ;
#274 = FACE_OUTER_BOUND ( 'NONE', #23362, .T. ) ;
#275 = CARTESIAN_POINT ( 'NONE',  ( 1.832998868059890096, 73.01698022778356290, 125.4013017422233247 ) ) ;
#276 = ORIENTED_EDGE ( 'NONE', *, *, #7410, .F. ) ;
#277 = CARTESIAN_POINT ( 'NONE',  ( 1.832998868059890096, 44.33343224355239443, 138.1720401012268553 ) ) ;
#278 = CARTESIAN_POINT ( 'NONE',  ( 25.64699802086726521, -56.66140964017665738, -97.66487797954063410 ) ) ;
#279 = ORIENTED_EDGE ( 'NONE', *, *, #27399, .T. ) ;
#280 = ORIENTED_EDGE ( 'NONE', *, *, #15755, .F. ) ;
#281 = ORIENTED_EDGE ( 'NONE', *, *, #16616, .F. ) ;
#282 =( BOUNDED_SURFACE ( )  B_SPLINE_SURFACE ( 3, 1, ( 
 ( #7883, #14041 ),
 ( #12179, #23143 ),
 ( #27133, #12311 ),
 ( #3114, #25284 ) ),
 .UNSPECIFIED., .F., .F., .F. ) 
 B_SPLINE_SURFACE_WITH_KNOTS ( ( 4, 4 ),
 ( 2, 2 ),
 ( 0.000000000000000000, 1.000000000000000000 ),
 ( 0.000000000000000000, 1.000000000000000000 ),
 .UNSPECIFIED. ) 
 GEOMETRIC_REPRESENTATION_ITEM ( )  RATIONAL_B_SPLINE_SURFACE ( (
 ( 1.000000000000000000, 1.000000000000000000),
 ( 0.6386103224230302855, 0.9954351624131538845),
 ( 0.6386103224230302855, 0.9954351624131538845),
 ( 1.000000000000000000, 1.000000000000000000) ) ) 
 REPRESENTATION_ITEM ( '' )  SURFACE ( )  );
#283 = CARTESIAN_POINT ( 'NONE',  ( -20.57838717382308147, -18.89542499756482741, 23.26537097894125594 ) ) ;
#284 = CARTESIAN_POINT ( 'NONE',  ( -1.019300379054419947, -35.83762006677421397, -28.53917295602885318 ) ) ;
#285 = EDGE_LOOP ( 'NONE', ( #12898, #28285, #1711, #7886 ) ) ;
#286 = CARTESIAN_POINT ( 'NONE',  ( -55.24390624410018802, 0.01027195578987812573, -0.001811362924359468263 ) ) ;
#287 = EDGE_CURVE ( 'NONE', #27787, #26061, #35, .T. ) ;
#288 = CARTESIAN_POINT ( 'NONE',  ( -1.048171036023500147, -1.020520027228813298, 45.78635789057867100 ) ) ;
#289 = ORIENTED_EDGE ( 'NONE', *, *, #8409, .F. ) ;
#290 = EDGE_CURVE ( 'NONE', #23510, #9049, #9297, .T. ) ;
#291 = EDGE_LOOP ( 'NONE', ( #9552, #9379, #25852, #8534 ) ) ;
#292 = CARTESIAN_POINT ( 'NONE',  ( 2.433796855181233454, 126.7346379669255754, 71.49415740225120430 ) ) ;
#293 = CARTESIAN_POINT ( 'NONE',  ( 28.37644542392844826, -58.62516076109965724, -109.6517504963494929 ) ) ;
#294 = CARTESIAN_POINT ( 'NONE',  ( -8.786685647604855376, -7.199674155859337787, -53.04920435127184675 ) ) ;
#295 = EDGE_CURVE ( 'NONE', #5458, #2573, #27496, .T. ) ;
#296 = CARTESIAN_POINT ( 'NONE',  ( 1.833206308920041883, -0.7447049373421851248, 145.1075835660718383 ) ) ;
#297 = CARTESIAN_POINT ( 'NONE',  ( -1.113427685306983550, -12.28784199929904730, 44.18561238466750041 ) ) ;
#298 = CARTESIAN_POINT ( 'NONE',  ( -20.20700224038492721, -28.44216453106542986, -8.199606986804219844 ) ) ;
#299 = CARTESIAN_POINT ( 'NONE',  ( 2.433796855181205476, -57.85512797797802165, -133.5135467655523769 ) ) ;
#300 = CARTESIAN_POINT ( 'NONE',  ( -9.156249394959713683, -48.78605533024723684, 24.29252099376542517 ) ) ;
#301 = PLANE ( 'NONE',  #25895 ) ;
#302 = CARTESIAN_POINT ( 'NONE',  ( 25.98107933586721430, -65.61242423298374149, -92.16448350435784675 ) ) ;
#303 = CARTESIAN_POINT ( 'NONE',  ( 1.833206310202331712, 141.7818020564282619, -30.89799345102821349 ) ) ;
#304 = CARTESIAN_POINT ( 'NONE',  ( 55.79472521941428198, -23.17337251492715922, -68.96476385670688103 ) ) ;
#305 = ORIENTED_EDGE ( 'NONE', *, *, #26640, .T. ) ;
#306 = ORIENTED_EDGE ( 'NONE', *, *, #5781, .T. ) ;
#307 = CARTESIAN_POINT ( 'NONE',  ( 25.64681081121879203, 0.4157506337743640534, -112.9102952884414464 ) ) ;
#308 = CARTESIAN_POINT ( 'NONE',  ( 25.87036335909425944, 107.2165474610300322, -35.87755773825609396 ) ) ;
#309 = VERTEX_POINT ( 'NONE', #27238 ) ;
#310 = ORIENTED_EDGE ( 'NONE', *, *, #10304, .F. ) ;
#311 = ORIENTED_EDGE ( 'NONE', *, *, #19586, .T. ) ;
#312 = CARTESIAN_POINT ( 'NONE',  ( -1.046935749540015115, 37.78548154587994645, -25.87617179820928826 ) ) ;
#313 = EDGE_CURVE ( 'NONE', #17905, #7760, #18301, .T. ) ;
#314 = CARTESIAN_POINT ( 'NONE',  ( 1.833603222531974719, 137.8693250773477814, 45.26427810762952930 ) ) ;
#315 = ORIENTED_EDGE ( 'NONE', *, *, #23818, .T. ) ;
#316 = CARTESIAN_POINT ( 'NONE',  ( -20.38016308990357928, -18.69911008768351479, -23.16952666206578826 ) ) ;
#317 = ADVANCED_FACE ( 'NONE', ( #25104 ), #23847, .F. ) ;
#318 = CARTESIAN_POINT ( 'NONE',  ( 10.93730112725978110, -119.3442956573278479, 92.80059208661636205 ) ) ;
#319 = CARTESIAN_POINT ( 'NONE',  ( -1.050231094221198536, 43.63617436699759367, 13.91061116148147292 ) ) ;
#320 = CARTESIAN_POINT ( 'NONE',  ( 1.894214914920949955, -144.4515288797482526, -14.22353624692145324 ) ) ;
#321 = LINE ( 'NONE', #25093, #2849 ) ;
#322 = CARTESIAN_POINT ( 'NONE',  ( 8.186469829614352989, -127.5731248499971997, -77.65916164626476359 ) ) ;
#323 = CARTESIAN_POINT ( 'NONE',  ( 25.81918753295379787, -65.67738364544791807, 91.98563552013010280 ) ) ;
#324 = CARTESIAN_POINT ( 'NONE',  ( 109.1587776205901861, 0.002904816147411970386, -0.006729130500864220592 ) ) ;
#325 = CARTESIAN_POINT ( 'NONE',  ( -1.619063947482201282, 43.26576862488434472, -16.67502769180576649 ) ) ;
#326 = EDGE_LOOP ( 'NONE', ( #25366, #7082, #18538, #9597 ) ) ;
#328 = CARTESIAN_POINT ( 'NONE',  ( -55.24198130335446422, -0.008310594958152726572, 0.004163123460802491127 ) ) ;
#327 = CARTESIAN_POINT ( 'NONE',  ( 25.64692232868534560, 91.53874134430799359, 66.10288322707224040 ) ) ;
#329 = CARTESIAN_POINT ( 'NONE',  ( -55.24198130335446422, 0.001516807524704581441, 0.009170435128245077103 ) ) ;
#330 = CARTESIAN_POINT ( 'NONE',  ( 25.64703792032467433, 46.06101937225606235, 103.0889146124066968 ) ) ;
#331 = CARTESIAN_POINT ( 'NONE',  ( -4.473127245936431073, 37.94261489385763753, 31.51789735524151226 ) ) ;
#332 = CARTESIAN_POINT ( 'NONE',  ( 32.73300124599734318, 99.90245962373836619, 62.10906484417276374 ) ) ;
#333 = ORIENTED_EDGE ( 'NONE', *, *, #2698, .T. ) ;
#334 = CARTESIAN_POINT ( 'NONE',  ( 109.1624594426973260, -0.004489871836309199289, -0.01531968460305922070 ) ) ;
#335 = VERTEX_POINT ( 'NONE', #11997 ) ;
#336 = CARTESIAN_POINT ( 'NONE',  ( -6.574463467970648622, -20.55340846381166742, -47.03022655117394635 ) ) ;
#337 = CARTESIAN_POINT ( 'NONE',  ( 1.833485406944043827, 141.8265699653867387, 30.69200235378984232 ) ) ;
#338 = ORIENTED_EDGE ( 'NONE', *, *, #13237, .T. ) ;
#339 = B_SPLINE_CURVE_WITH_KNOTS ( 'NONE', 3,
 ( #7794, #16848, #3453, #21294, #25631, #12237, #12504, #1706 ),
 .UNSPECIFIED., .F., .F.,
 ( 4, 2, 2, 4 ),
 ( 6.938893903907228378E-18, 0.0002429592666046687642, 0.0004859185332093305895, 0.0009718370664186714789 ),
 .UNSPECIFIED. ) ;
#340 = ORIENTED_EDGE ( 'NONE', *, *, #22680, .F. ) ;
#341 = CARTESIAN_POINT ( 'NONE',  ( -1.045287976400362417, -28.14015102489855735, -36.12803364096578207 ) ) ;
#342 = VERTEX_POINT ( 'NONE', #20623 ) ;
#343 = CARTESIAN_POINT ( 'NONE',  ( 2.063896406836605024, -96.20114399516322123, -108.8509294491474861 ) ) ;
#344 = B_SPLINE_CURVE_WITH_KNOTS ( 'NONE', 3,
 ( #15021, #2939, #13866, #20192 ),
 .UNSPECIFIED., .F., .F.,
 ( 4, 4 ),
 ( 2.281672496420497865E-17, 0.008383560773332699931 ),
 .UNSPECIFIED. ) ;
#345 = ORIENTED_EDGE ( 'NONE', *, *, #8746, .T. ) ;
#346 = CARTESIAN_POINT ( 'NONE',  ( -20.57838717382308147, 16.28767523336121315, -25.16001208503110931 ) ) ;
#347 = EDGE_CURVE ( 'NONE', #22931, #27450, #12814, .T. ) ;
#348 = EDGE_CURVE ( 'NONE', #19892, #25954, #10374, .T. ) ;
#349 = CARTESIAN_POINT ( 'NONE',  ( 32.73300124599732186, 0.000000000000000000, 0.000000000000000000 ) ) ;
#350 = EDGE_CURVE ( 'NONE', #18707, #4229, #24424, .T. ) ;
#351 = CARTESIAN_POINT ( 'NONE',  ( -55.24300891470650754, -0.009225237711100996510, 0.003362556190412404646 ) ) ;
#352 = CARTESIAN_POINT ( 'NONE',  ( 25.64703792032472407, -66.24710921678119746, 91.43447020678409842 ) ) ;
#353 = AXIS2_PLACEMENT_3D ( 'NONE', #16721, #21587, #19154 ) ;
#354 = CARTESIAN_POINT ( 'NONE',  ( 1.832998868059890096, 138.1720401012272816, -44.33343224355093781 ) ) ;
#355 = CARTESIAN_POINT ( 'NONE',  ( 2.433796855181205476, -60.50726454507993424, 132.3327394885229182 ) ) ;
#356 = FACE_OUTER_BOUND ( 'NONE', #18685, .T. ) ;
#357 = B_SPLINE_CURVE_WITH_KNOTS ( 'NONE', 3,
 ( #19510, #22251, #9143, #17897, #28277, #17341, #26130 ),
 .UNSPECIFIED., .F., .F.,
 ( 4, 3, 4 ),
 ( 0.000000000000000000, 0.006568092053401790135, 0.02506242213020846640 ),
 .UNSPECIFIED. ) ;
#358 = CARTESIAN_POINT ( 'NONE',  ( -25.21435515916043002, 23.92354251275938992, -25.00736669481030106 ) ) ;
#359 = DIRECTION ( 'NONE',  ( 0.000000000000000000, 0.000000000000000000, 1.000000000000000000 ) ) ;
#360 = CARTESIAN_POINT ( 'NONE',  ( 25.64660436782549269, -112.2303901742708376, 12.37913844083004733 ) ) ;
#361 = FACE_OUTER_BOUND ( 'NONE', #15013, .T. ) ;
#363 = CARTESIAN_POINT ( 'NONE',  ( -6.574463467970653063, 20.55340846381200848, 47.03022655117382556 ) ) ;
#362 = CARTESIAN_POINT ( 'NONE',  ( 2.433796855181219243, -31.67151202412867761, -142.0211193075559493 ) ) ;
#364 = CARTESIAN_POINT ( 'NONE',  ( 25.64681081121879203, -107.2555980796243773, 35.28660243342513070 ) ) ;
#365 = CARTESIAN_POINT ( 'NONE',  ( 1.894214914920953952, -125.2241265685475895, 73.39939580274894126 ) ) ;
#366 = ORIENTED_EDGE ( 'NONE', *, *, #21501, .T. ) ;
#367 = CARTESIAN_POINT ( 'NONE',  ( -1.155001620486262759, 16.13799328198422245, -42.97366440495917317 ) ) ;
#368 = CARTESIAN_POINT ( 'NONE',  ( 25.65782528836479770, 110.5695798068306317, -22.91156770660693454 ) ) ;
#369 = FACE_OUTER_BOUND ( 'NONE', #18098, .T. ) ;
#370 = DIRECTION ( 'NONE',  ( -1.000000000000000000, -0.000000000000000000, -0.000000000000000000 ) ) ;
#371 = AXIS2_PLACEMENT_3D ( 'NONE', #18675, #18230, #11912 ) ;
#372 = ORIENTED_EDGE ( 'NONE', *, *, #18657, .T. ) ;
#373 = CARTESIAN_POINT ( 'NONE',  ( 109.1592201516379674, -0.005485778713202971689, -0.005631912476303796086 ) ) ;
#374 = VECTOR ( 'NONE', #5725, 1000.000000000000000 ) ;
#375 = EDGE_CURVE ( 'NONE', #9976, #3267, #7611, .T. ) ;
#376 = CARTESIAN_POINT ( 'NONE',  ( -8.786685647604885574, 6.096987947571466530E-17, -1.524246986892866633E-17 ) ) ;
#377 = CARTESIAN_POINT ( 'NONE',  ( -1.113548883309548376, 45.82026503946953255, 1.968251867499028585 ) ) ;
#378 = VERTEX_POINT ( 'NONE', #8125 ) ;
#379 = CARTESIAN_POINT ( 'NONE',  ( 6.224689322667630975, 84.93872395422975785, 121.2721959030541115 ) ) ;
#380 = ADVANCED_FACE ( 'NONE', ( #10939 ), #22761, .F. ) ;
#381 = ORIENTED_EDGE ( 'NONE', *, *, #6506, .T. ) ;
#382 = LINE ( 'NONE', #15620, #6481 ) ;
#383 = CARTESIAN_POINT ( 'NONE',  ( -1.239374126674604337, -16.50008610789329921, -42.99367564261275021 ) ) ;
#384 = VERTEX_POINT ( 'NONE', #15379 ) ;
#385 = EDGE_CURVE ( 'NONE', #12613, #15221, #10008, .T. ) ;
#386 = CARTESIAN_POINT ( 'NONE',  ( -28.41354790283022069, 23.16239616762931064, -1.249099604787157425 ) ) ;
#387 = CARTESIAN_POINT ( 'NONE',  ( 25.64708010899963142, -34.83947233573751134, 107.4019003251855366 ) ) ;
#388 = CARTESIAN_POINT ( 'NONE',  ( -10.86508079875782329, -46.07061504567103327, -22.20099862734805996 ) ) ;
#389 = CARTESIAN_POINT ( 'NONE',  ( -1.463510566862830986, 16.57250862017420090, -43.13857742234511505 ) ) ;
#390 = CARTESIAN_POINT ( 'NONE',  ( 25.64681081121879203, 110.3564950173081769, 23.88203588908119457 ) ) ;
#391 = VERTEX_POINT ( 'NONE', #27957 ) ;
#392 = B_SPLINE_CURVE_WITH_KNOTS ( 'NONE', 3,
 ( #24535, #6970, #24240, #26380, #19904, #11274, #17740, #26517, #26809, #22059 ),
 .UNSPECIFIED., .F., .F.,
 ( 4, 2, 2, 2, 4 ),
 ( 4.336808689942017255E-19, 0.0003346267210630946812, 0.0006692534421261889287, 0.001003880163189283230, 0.001338506884252377424 ),
 .UNSPECIFIED. ) ;
#393 = AXIS2_PLACEMENT_3D ( 'NONE', #9843, #3208, #902 ) ;
#394 = B_SPLINE_CURVE_WITH_KNOTS ( 'NONE', 3,
 ( #14459, #12169, #11525, #17848, #8956, #17713, #6658, #15405 ),
 .UNSPECIFIED., .F., .F.,
 ( 4, 2, 2, 4 ),
 ( 2.214340075454938295E-16, 0.002761568181852865067, 0.005523136363705506355, 0.01104627272741079066 ),
 .UNSPECIFIED. ) ;
#395 = CARTESIAN_POINT ( 'NONE',  ( -55.25297051322618813, -0.01019003092403672657, 0.01093108995495161231 ) ) ;
#396 = CARTESIAN_POINT ( 'NONE',  ( -55.24300891470648622, 0.006048736206180948920, -0.007734635432132875611 ) ) ;
#397 = VECTOR ( 'NONE', #413, 1000.000000000000114 ) ;
#398 = FACE_OUTER_BOUND ( 'NONE', #13442, .T. ) ;
#399 = ORIENTED_EDGE ( 'NONE', *, *, #9408, .F. ) ;
#400 = ORIENTED_EDGE ( 'NONE', *, *, #20280, .T. ) ;
#401 = EDGE_LOOP ( 'NONE', ( #6763, #21380, #8242, #7080 ) ) ;
#402 = CARTESIAN_POINT ( 'NONE',  ( -90.83090735639699176, 2.449293598294706119E-15, 20.00000000000000000 ) ) ;
#403 = LINE ( 'NONE', #691, #28171 ) ;
#404 = CARTESIAN_POINT ( 'NONE',  ( 25.98107933586746654, -24.58827779736852648, 110.4296102877912205 ) ) ;
#405 = CARTESIAN_POINT ( 'NONE',  ( -1.050230347699842692, 5.964912479342754695E-15, -45.79907861674080749 ) ) ;
#406 = CARTESIAN_POINT ( 'NONE',  ( -55.24390624410018802, 0.009374879212971231821, -0.004572280736701976080 ) ) ;
#407 = CARTESIAN_POINT ( 'NONE',  ( 25.65782528836481191, -103.3897864210299105, 45.39960327191575118 ) ) ;
#408 = ORIENTED_EDGE ( 'NONE', *, *, #26281, .F. ) ;
#409 = CARTESIAN_POINT ( 'NONE',  ( -20.21097721712959228, -29.61001327235739566, -0.3305963429841727863 ) ) ;
#410 = CARTESIAN_POINT ( 'NONE',  ( 109.1586900883932856, -0.006960773163852201732, 0.001582822706032804708 ) ) ;
#411 = CARTESIAN_POINT ( 'NONE',  ( 25.64706233108855216, -0.08898442853967061805, 112.9112020921832453 ) ) ;
#412 = CARTESIAN_POINT ( 'NONE',  ( 25.64681081121880624, 12.21581276189807497, 112.2483031020013868 ) ) ;
#413 = DIRECTION ( 'NONE',  ( 0.7637818620346800147, -0.6068965246771045319, -0.2198041754873859832 ) ) ;
#414 = VERTEX_POINT ( 'NONE', #12558 ) ;
#415 = CARTESIAN_POINT ( 'NONE',  ( -1.619063947482197729, 38.92136151114943488, 25.20140673341330739 ) ) ;
#416 =( BOUNDED_SURFACE ( )  B_SPLINE_SURFACE ( 3, 1, ( 
 ( #23177, #18546 ),
 ( #1262, #20412 ),
 ( #15948, #22887 ),
 ( #3145, #12211 ) ),
 .UNSPECIFIED., .F., .F., .F. ) 
 B_SPLINE_SURFACE_WITH_KNOTS ( ( 4, 4 ),
 ( 2, 2 ),
 ( 0.000000000000000000, 1.000000000000000000 ),
 ( 0.000000000000000000, 1.000000000000000000 ),
 .UNSPECIFIED. ) 
 GEOMETRIC_REPRESENTATION_ITEM ( )  RATIONAL_B_SPLINE_SURFACE ( (
 ( 1.000000000000000000, 1.000000000000000000),
 ( 0.9593753223639863714, 0.9995975284513187731),
 ( 0.9593753223639863714, 0.9995975284513187731),
 ( 1.000000000000000000, 1.000000000000000000) ) ) 
 REPRESENTATION_ITEM ( '' )  SURFACE ( )  );
#417 = EDGE_CURVE ( 'NONE', #342, #6343, #26799, .T. ) ;
#418 = ORIENTED_EDGE ( 'NONE', *, *, #11574, .F. ) ;
#419 = LINE ( 'NONE', #6915, #25368 ) ;
#420 = B_SPLINE_CURVE_WITH_KNOTS ( 'NONE', 3,
 ( #20470, #3346, #12134, #20901, #1191, #9985, #22944 ),
 .UNSPECIFIED., .F., .F.,
 ( 4, 3, 4 ),
 ( 1.734723475976807094E-18, 0.02816610861753245793, 0.04000277880656208374 ),
 .UNSPECIFIED. ) ;
#421 = CARTESIAN_POINT ( 'NONE',  ( 1.833838850855462166, -117.3439621615258233, -85.36536653357470072 ) ) ;
#422 = VERTEX_POINT ( 'NONE', #16758 ) ;
#423 = EDGE_CURVE ( 'NONE', #4272, #25436, #20279, .T. ) ;
#424 = ORIENTED_EDGE ( 'NONE', *, *, #2283, .T. ) ;
#425 = ORIENTED_EDGE ( 'NONE', *, *, #11302, .F. ) ;
#426 = EDGE_CURVE ( 'NONE', #2712, #13659, #1071, .T. ) ;
#427 = CARTESIAN_POINT ( 'NONE',  ( 9.884929003653608603, 109.0134320167733364, 103.8128997986861322 ) ) ;
#428 = EDGE_CURVE ( 'NONE', #3933, #17753, #6233, .T. ) ;
#429 = LINE ( 'NONE', #11507, #25331 ) ;
#430 = CARTESIAN_POINT ( 'NONE',  ( 2.430230287190589422, -109.1043569252007615, -96.28466919684210268 ) ) ;
#431 = VERTEX_POINT ( 'NONE', #21481 ) ;
#432 = CARTESIAN_POINT ( 'NONE',  ( 32.73300124599738581, 99.90245962373917621, -62.10906484417127871 ) ) ;
#433 = FACE_OUTER_BOUND ( 'NONE', #2313, .T. ) ;
#434 = CARTESIAN_POINT ( 'NONE',  ( 55.79472521941428198, -43.35047097963410323, -58.42842213658372685 ) ) ;
#435 = ORIENTED_EDGE ( 'NONE', *, *, #9896, .F. ) ;
#436 = LINE ( 'NONE', #22029, #7013 ) ;
#437 = VERTEX_POINT ( 'NONE', #1752 ) ;
#438 = CARTESIAN_POINT ( 'NONE',  ( 2.433796855181233454, 142.6247129145648387, 28.83182736670586266 ) ) ;
#439 = CARTESIAN_POINT ( 'NONE',  ( 16.75465622695653423, -67.05928661304268701, -125.4242432475199962 ) ) ;
#440 = LINE ( 'NONE', #9227, #24777 ) ;
#441 = CARTESIAN_POINT ( 'NONE',  ( 32.73300124599732186, 0.000000000000000000, 0.000000000000000000 ) ) ;
#442 = CARTESIAN_POINT ( 'NONE',  ( 2.430230287190589422, -46.34481016236729545, -137.9371479820467243 ) ) ;
#443 = CARTESIAN_POINT ( 'NONE',  ( 32.73300124599735739, 32.68291970228236920, 113.0038235389603472 ) ) ;
#444 = CARTESIAN_POINT ( 'NONE',  ( -7.078251931573406708, -47.71415099571790108, 20.86696228105274997 ) ) ;
#445 = CARTESIAN_POINT ( 'NONE',  ( -20.57838717382308147, 16.28767523336157552, 25.16001208503087838 ) ) ;
#446 = CARTESIAN_POINT ( 'NONE',  ( -55.24271866751342941, -0.001545935011626541761, -0.009369360294294543784 ) ) ;
#447 = CARTESIAN_POINT ( 'NONE',  ( 1.832998868059890096, 97.49378069860796359, 107.4798986104863303 ) ) ;
#448 = CARTESIAN_POINT ( 'NONE',  ( 25.69398547355840989, -107.6418378907641511, -34.19446713634692259 ) ) ;
#449 = VERTEX_POINT ( 'NONE', #25543 ) ;
#450 =( BOUNDED_SURFACE ( )  B_SPLINE_SURFACE ( 3, 1, ( 
 ( #22540, #11583 ),
 ( #13591, #17896 ),
 ( #15756, #11163 ),
 ( #11441, #9010 ) ),
 .UNSPECIFIED., .F., .F., .F. ) 
 B_SPLINE_SURFACE_WITH_KNOTS ( ( 4, 4 ),
 ( 2, 2 ),
 ( 0.000000000000000000, 1.000000000000000000 ),
 ( 0.000000000000000000, 1.000000000000000000 ),
 .UNSPECIFIED. ) 
 GEOMETRIC_REPRESENTATION_ITEM ( )  RATIONAL_B_SPLINE_SURFACE ( (
 ( 1.000000000000000000, 1.000000000000000000),
 ( 0.9960225298536222738, 0.9999952330161893110),
 ( 0.9960225298536222738, 0.9999952330161893110),
 ( 1.000000000000000000, 1.000000000000000000) ) ) 
 REPRESENTATION_ITEM ( '' )  SURFACE ( )  );
#451 = ORIENTED_EDGE ( 'NONE', *, *, #25516, .F. ) ;
#452 = CARTESIAN_POINT ( 'NONE',  ( 25.64681081121879203, 23.88203588908081443, 110.3564950173082480 ) ) ;
#453 = CARTESIAN_POINT ( 'NONE',  ( -1.019300379054419947, -28.53917295602871818, 35.83762006677432055 ) ) ;
#454 = ORIENTED_EDGE ( 'NONE', *, *, #2186, .F. ) ;
#455 = EDGE_CURVE ( 'NONE', #26384, #7211, #18757, .T. ) ;
#456 = EDGE_LOOP ( 'NONE', ( #7870, #6919, #10973, #27044 ) ) ;
#457 = VERTEX_POINT ( 'NONE', #12411 ) ;
#458 = CARTESIAN_POINT ( 'NONE',  ( -55.24271866751342941, 0.001545935011631000867, -0.009369360294295843092 ) ) ;
#459 = EDGE_CURVE ( 'NONE', #23588, #27642, #11361, .T. ) ;
#460 = EDGE_CURVE ( 'NONE', #21703, #19144, #134, .T. ) ;
#461 = AXIS2_PLACEMENT_3D ( 'NONE', #8171, #27874, #16935 ) ;
#462 = CARTESIAN_POINT ( 'NONE',  ( 28.37603512858456156, 58.91311972676539455, 98.45183098817996381 ) ) ;
#463 = CARTESIAN_POINT ( 'NONE',  ( -55.24198130335446422, 0.009190321388309335635, 0.001391250620105184774 ) ) ;
#464 = B_SPLINE_CURVE_WITH_KNOTS ( 'NONE', 3,
 ( #6253, #23690, #8010, #3941 ),
 .UNSPECIFIED., .F., .F.,
 ( 4, 4 ),
 ( 0.0009910334943225120648, 0.001982023823822943315 ),
 .UNSPECIFIED. ) ;
#465 = CARTESIAN_POINT ( 'NONE',  ( -20.57838717382308502, 28.96176188950218844, -7.715628353033780584 ) ) ;
#466 = CARTESIAN_POINT ( 'NONE',  ( -7.078251931573400491, 5.101176922830666705, -51.82710018979476274 ) ) ;
#467 = CARTESIAN_POINT ( 'NONE',  ( -20.20700224038492010, 24.51628800869071867, 16.58740185276683832 ) ) ;
#468 = CARTESIAN_POINT ( 'NONE',  ( 8.186469777910550860, 143.0750864738774624, 42.84118569629400497 ) ) ;
#469 = CARTESIAN_POINT ( 'NONE',  ( 25.64670758986457599, 34.41755235608744101, 107.5375791514044579 ) ) ;
#470 = CARTESIAN_POINT ( 'NONE',  ( 25.87036335909428075, -65.65170964736196879, 92.04585932622757127 ) ) ;
#471 = CARTESIAN_POINT ( 'NONE',  ( -8.786685647604896232, 25.35688121747570278, 47.14957014837326454 ) ) ;
#472 = ORIENTED_EDGE ( 'NONE', *, *, #26439, .F. ) ;
#473 = AXIS2_PLACEMENT_3D ( 'NONE', #13879, #26834, #13590 ) ;
#474 = CARTESIAN_POINT ( 'NONE',  ( 32.73300124599740002, 62.10906484417377271, -99.90245962373766986 ) ) ;
#475 = VECTOR ( 'NONE', #9261, 1000.000000000000227 ) ;
#476 = CARTESIAN_POINT ( 'NONE',  ( 32.73300124599739291, 81.52272205837319063, -84.80615050150287004 ) ) ;
#477 = CARTESIAN_POINT ( 'NONE',  ( 109.1586900883932856, 0.005371970278528643075, 0.004701023939945730111 ) ) ;
#478 = CARTESIAN_POINT ( 'NONE',  ( 109.1624594426973118, 0.002863932759303090912, -0.01570508117120619079 ) ) ;
#479 = CARTESIAN_POINT ( 'NONE',  ( -22.23342874802668234, -26.81018246605525590, 16.78332232459670337 ) ) ;
#480 = ORIENTED_EDGE ( 'NONE', *, *, #423, .T. ) ;
#481 = CARTESIAN_POINT ( 'NONE',  ( -20.20700224038492721, -10.08426345511609235, -27.82980252387815767 ) ) ;
#482 = ORIENTED_EDGE ( 'NONE', *, *, #25056, .F. ) ;
#483 = CARTESIAN_POINT ( 'NONE',  ( -1.048172774974303278, 43.23017713506524728, -15.11899685083838030 ) ) ;
#484 = CARTESIAN_POINT ( 'NONE',  ( 28.37599760073040045, -100.2461467136614175, 55.80522390574083857 ) ) ;
#485 = ORIENTED_EDGE ( 'NONE', *, *, #70, .T. ) ;
#486 = ADVANCED_FACE ( 'NONE', ( #274 ), #4144, .F. ) ;
#487 = CARTESIAN_POINT ( 'NONE',  ( -1.619063947482197729, -29.22875152547781852, -35.99532424477369830 ) ) ;
#488 = ORIENTED_EDGE ( 'NONE', *, *, #17893, .F. ) ;
#489 = DIRECTION ( 'NONE',  ( 0.000000000000000000, 0.000000000000000000, 1.000000000000000000 ) ) ;
#490 = ORIENTED_EDGE ( 'NONE', *, *, #6319, .F. ) ;
#491 = EDGE_CURVE ( 'NONE', #21106, #21028, #26123, .T. ) ;
#492 = EDGE_CURVE ( 'NONE', #14205, #24138, #20617, .T. ) ;
#493 = ORIENTED_EDGE ( 'NONE', *, *, #16429, .F. ) ;
#494 = CARTESIAN_POINT ( 'NONE',  ( 10.93730112725996406, 10.89264110825190457, -150.7858122213661716 ) ) ;
#495 = CIRCLE ( 'NONE', #5559, 151.1787379149930359 ) ;
#496 = B_SPLINE_CURVE_WITH_KNOTS ( 'NONE', 3,
 ( #10138, #14280, #27678, #12557, #8124, #3925, #6368 ),
 .UNSPECIFIED., .F., .F.,
 ( 4, 3, 4 ),
 ( 5.442941977417787173E-16, 0.02816610861753245793, 0.04000277880656272211 ),
 .UNSPECIFIED. ) ;
#497 = CARTESIAN_POINT ( 'NONE',  ( 109.1586059443104944, -0.001014167950280833253, 0.007001002073871743885 ) ) ;
#498 = CARTESIAN_POINT ( 'NONE',  ( -1.049817751779873687, -13.66628317065018017, -43.71287583013722156 ) ) ;
#499 = DIRECTION ( 'NONE',  ( -0.7563875759206388771, -0.5490129373055306905, -0.3556158456312839555 ) ) ;
#500 = CIRCLE ( 'NONE', #6062, 34.60786435723138510 ) ;
#501 = CARTESIAN_POINT ( 'NONE',  ( 109.1586900883932856, -0.006231977675082131345, 0.003481399864227353348 ) ) ;
#502 = CARTESIAN_POINT ( 'NONE',  ( -55.24390624410018802, -0.001811362924359030029, -0.01027195578987783083 ) ) ;
#503 = CARTESIAN_POINT ( 'NONE',  ( -20.47566338032521216, -16.24827550219808003, 25.06314818626711372 ) ) ;
#505 = CARTESIAN_POINT ( 'NONE',  ( 25.65782528836480836, -0.5778133093785753349, 112.9169519833626509 ) ) ;
#504 = CARTESIAN_POINT ( 'NONE',  ( -28.41354790283022069, 1.249099604787076601, -23.16239616762931064 ) ) ;
#506 = CARTESIAN_POINT ( 'NONE',  ( -1.113427685306999759, -1.967672929087495470, -45.82016658690750432 ) ) ;
#507 = ORIENTED_EDGE ( 'NONE', *, *, #17028, .F. ) ;
#508 = CARTESIAN_POINT ( 'NONE',  ( -20.90916690077964901, -18.74041620980142753, 34.84883504600970383 ) ) ;
#509 = DIRECTION ( 'NONE',  ( 0.7563875759206388771, 0.03500244528122559151, -0.6531865459554678788 ) ) ;
#510 = CARTESIAN_POINT ( 'NONE',  ( -1.019300379054419947, -38.21680004809145714, 25.26451264419685572 ) ) ;
#511 = CARTESIAN_POINT ( 'NONE',  ( 2.430230287190589422, -43.58368230469487514, 138.8342928068218498 ) ) ;
#512 = CARTESIAN_POINT ( 'NONE',  ( 2.433796855181233454, 126.7346379669255754, 71.49415740225120430 ) ) ;
#513 = EDGE_CURVE ( 'NONE', #28027, #12090, #11490, .T. ) ;
#514 = ORIENTED_EDGE ( 'NONE', *, *, #11989, .T. ) ;
#515 = CARTESIAN_POINT ( 'NONE',  ( -23.77929240705204705, 26.20227034809557054, -25.06639637888430272 ) ) ;
#516 = VECTOR ( 'NONE', #25527, 1000.000000000000114 ) ;
#517 = CARTESIAN_POINT ( 'NONE',  ( 25.70243777736189017, 110.6300896395620157, -22.76560620136952906 ) ) ;
#518 = CARTESIAN_POINT ( 'NONE',  ( 1.832998868059858122, 45.34898734666231235, -137.8420662456165644 ) ) ;
#519 = ORIENTED_EDGE ( 'NONE', *, *, #17768, .F. ) ;
#520 = CARTESIAN_POINT ( 'NONE',  ( 25.64700659047692710, 110.4909389345862536, -23.25292178500255247 ) ) ;
#521 = VECTOR ( 'NONE', #13115, 1000.000000000000000 ) ;
#523 = EDGE_LOOP ( 'NONE', ( #9442, #25220, #8557, #9955 ) ) ;
#522 = EDGE_CURVE ( 'NONE', #14145, #16310, #19942, .T. ) ;
#524 = CARTESIAN_POINT ( 'NONE',  ( -1.058473599757830286, -15.81436910992550438, -42.99101666105224240 ) ) ;
#525 = EDGE_CURVE ( 'NONE', #18738, #20839, #8007, .T. ) ;
#526 = CIRCLE ( 'NONE', #16645, 117.6351876552689504 ) ;
#527 = CARTESIAN_POINT ( 'NONE',  ( 10.93730112725990011, -151.0983828010092225, 4.928439153519769356 ) ) ;
#528 = CARTESIAN_POINT ( 'NONE',  ( 26.11404676487257603, 112.4785329405483765, -12.95861723607337979 ) ) ;
#529 = ORIENTED_EDGE ( 'NONE', *, *, #3330, .T. ) ;
#530 = CARTESIAN_POINT ( 'NONE',  ( -21.41430102051751660, -28.68859753627386766, 11.22990201072307137 ) ) ;
#531 = VERTEX_POINT ( 'NONE', #9493 ) ;
#532 = CARTESIAN_POINT ( 'NONE',  ( -20.24399999263414784, 28.55700515887720670, -7.930419334766287243 ) ) ;
#533 = B_SPLINE_CURVE_WITH_KNOTS ( 'NONE', 3,
 ( #405, #17949, #26593, #834, #2856, #9186, #26735, #267, #4869, #25041 ),
 .UNSPECIFIED., .F., .F.,
 ( 4, 3, 3, 4 ),
 ( 0.001530725384384652287, 0.001531419946797919589, 0.002296279302920155134, 0.003061450627205758099 ),
 .UNSPECIFIED. ) ;
#534 = CARTESIAN_POINT ( 'NONE',  ( 10.93730112725991077, -79.81734490845832397, -128.3908183996600201 ) ) ;
#535 = B_SPLINE_CURVE_WITH_KNOTS ( 'NONE', 3,
 ( #21357, #5971, #23537, #25826, #16620, #12292, #12840 ),
 .UNSPECIFIED., .F., .F.,
 ( 4, 3, 4 ),
 ( 0.000000000000000000, 0.006568092053401830901, 0.02506242213020847681 ),
 .UNSPECIFIED. ) ;
#536 = CARTESIAN_POINT ( 'NONE',  ( -25.21435515916043713, -34.05351380035337883, -6.169479169075319014 ) ) ;
#537 = CARTESIAN_POINT ( 'NONE',  ( -1.583189561560253589, 16.68617981233763814, 43.29471907393723029 ) ) ;
#538 = B_SPLINE_CURVE_WITH_KNOTS ( 'NONE', 3,
 ( #22328, #10958, #3277, #25461, #1248, #12470, #17073, #12058, #12199, #19232 ),
 .UNSPECIFIED., .F., .F.,
 ( 4, 3, 3, 4 ),
 ( 5.003707553108401214E-17, 0.0002669559177086153526, 0.0005339118354151005733, 0.001067817517169148637 ),
 .UNSPECIFIED. ) ;
#539 = ORIENTED_EDGE ( 'NONE', *, *, #25407, .T. ) ;
#540 = CARTESIAN_POINT ( 'NONE',  ( 32.73300124599735739, -51.32617430724984331, 105.8473486001049224 ) ) ;
#541 = CARTESIAN_POINT ( 'NONE',  ( -55.24271866751342941, -0.001425019990781919424, 0.009388511352197656881 ) ) ;
#542 = CARTESIAN_POINT ( 'NONE',  ( 1.834118845439484335, 141.9759513273468485, -29.99597360112932520 ) ) ;
#543 = EDGE_LOOP ( 'NONE', ( #12436, #24728, #15919, #11277 ) ) ;
#544 = VECTOR ( 'NONE', #20502, 1000.000000000000000 ) ;
#545 = ADVANCED_FACE ( 'NONE', ( #26604 ), #27863, .F. ) ;
#546 = VERTEX_POINT ( 'NONE', #17962 ) ;
#547 = ORIENTED_EDGE ( 'NONE', *, *, #14124, .T. ) ;
#548 = FACE_OUTER_BOUND ( 'NONE', #7468, .T. ) ;
#549 = CARTESIAN_POINT ( 'NONE',  ( -25.21435515916043002, 23.92354251275938992, -25.00736669481030106 ) ) ;
#550 = CARTESIAN_POINT ( 'NONE',  ( -8.786685647604890903, -37.00619870957905277, 38.68584556812340480 ) ) ;
#551 = CARTESIAN_POINT ( 'NONE',  ( -55.24271866751342941, -0.009388511352199774979, 0.001425019990778933097 ) ) ;
#552 = DIRECTION ( 'NONE',  ( 0.000000000000000000, -1.000000000000000000, 0.000000000000000000 ) ) ;
#553 = CARTESIAN_POINT ( 'NONE',  ( 21.16825799904901828, -46.02882515936396857, -127.3716170292828167 ) ) ;
#554 = CARTESIAN_POINT ( 'NONE',  ( 10.93730112725993919, -42.00474393596157086, -145.2260730187406352 ) ) ;
#555 = EDGE_CURVE ( 'NONE', #27960, #13900, #7200, .T. ) ;
#556 = ORIENTED_EDGE ( 'NONE', *, *, #4783, .T. ) ;
#557 = CARTESIAN_POINT ( 'NONE',  ( 1.894214914920960835, 145.1469726764544532, -0.9536781033365084870 ) ) ;
#558 = CARTESIAN_POINT ( 'NONE',  ( -1.583189561560256253, -38.94740041318311796, -25.21827308671218404 ) ) ;
#559 = CARTESIAN_POINT ( 'NONE',  ( -25.21435515916043713, 15.02493970636190745, 31.17620025257570759 ) ) ;
#560 = CARTESIAN_POINT ( 'NONE',  ( 14.74894986621300319, -1.023413983156987147E-16, 2.558534957892467869E-17 ) ) ;
#561 = EDGE_CURVE ( 'NONE', #945, #6378, #2452, .T. ) ;
#562 = CARTESIAN_POINT ( 'NONE',  ( 13.36082413113061307, 81.89226687792266546, -129.1512766091112780 ) ) ;
#563 = ORIENTED_EDGE ( 'NONE', *, *, #1401, .F. ) ;
#564 = CARTESIAN_POINT ( 'NONE',  ( 25.64681081121879203, -12.21581276189731469, -112.2483031020014579 ) ) ;
#565 = VERTEX_POINT ( 'NONE', #13653 ) ;
#566 = CARTESIAN_POINT ( 'NONE',  ( -20.38016308990358638, 29.73560196176844528, -1.509191766064308382 ) ) ;
#567 = CARTESIAN_POINT ( 'NONE',  ( -20.20700224038492010, -0.9908225410476447781, 29.58392382092673500 ) ) ;
#568 = ORIENTED_EDGE ( 'NONE', *, *, #226, .T. ) ;
#569 = VECTOR ( 'NONE', #11846, 1000.000000000000114 ) ;
#570 = ORIENTED_EDGE ( 'NONE', *, *, #4414, .T. ) ;
#571 = ORIENTED_EDGE ( 'NONE', *, *, #1469, .T. ) ;
#572 = CARTESIAN_POINT ( 'NONE',  ( -55.25719721206881729, -0.01115102788683311301, 0.0006290797159230496292 ) ) ;
#573 = CARTESIAN_POINT ( 'NONE',  ( 109.1586900883932856, -0.005715190711488748326, -0.004277182003220934836 ) ) ;
#574 = DIRECTION ( 'NONE',  ( 0.000000000000000000, 0.000000000000000000, 1.000000000000000000 ) ) ;
#575 = CARTESIAN_POINT ( 'NONE',  ( 28.37644542392841274, 17.02293047611527399, -123.1691345231580783 ) ) ;
#576 = EDGE_LOOP ( 'NONE', ( #8508, #7598, #22350, #4722 ) ) ;
#577 = CARTESIAN_POINT ( 'NONE',  ( 1.894214914920941517, 14.22353624692188667, -144.4515288797482242 ) ) ;
#578 = CARTESIAN_POINT ( 'NONE',  ( -22.23226125620942284, 11.82389163795251541, 29.33577758406437042 ) ) ;
#579 = CARTESIAN_POINT ( 'NONE',  ( 25.64660436782565256, -45.39454672041182448, 103.3839381879729444 ) ) ;
#580 = ORIENTED_EDGE ( 'NONE', *, *, #26933, .T. ) ;
#581 = EDGE_CURVE ( 'NONE', #23740, #22045, #4854, .T. ) ;
#582 = ORIENTED_EDGE ( 'NONE', *, *, #6651, .F. ) ;
#583 = CARTESIAN_POINT ( 'NONE',  ( -1.019300379054419947, -45.76814864815092676, -2.023851374322514829 ) ) ;
#584 = ADVANCED_FACE ( 'NONE', ( #995 ), #20713, .F. ) ;
#585 = CARTESIAN_POINT ( 'NONE',  ( 19.66333377628711432, -64.94841092372091396, -121.4767361208140670 ) ) ;
#586 = CARTESIAN_POINT ( 'NONE',  ( -55.24271866751342941, -0.006671293903667678896, -0.006757859501010191408 ) ) ;
#587 = CARTESIAN_POINT ( 'NONE',  ( 24.01988960052062438, 23.05141021591281714, 129.0012934948647683 ) ) ;
#588 = CARTESIAN_POINT ( 'NONE',  ( 30.58324630866345473, -63.85566901681546881, -102.7123253644122087 ) ) ;
#590 =( BOUNDED_SURFACE ( )  B_SPLINE_SURFACE ( 3, 1, ( 
 ( #23272, #3523 ),
 ( #12305, #12797 ),
 ( #23778, #4027 ),
 ( #10517, #28197 ) ),
 .UNSPECIFIED., .F., .F., .F. ) 
 B_SPLINE_SURFACE_WITH_KNOTS ( ( 4, 4 ),
 ( 2, 2 ),
 ( 0.000000000000000000, 1.000000000000000000 ),
 ( 0.000000000000000000, 1.000000000000000000 ),
 .UNSPECIFIED. ) 
 GEOMETRIC_REPRESENTATION_ITEM ( )  RATIONAL_B_SPLINE_SURFACE ( (
 ( 1.000000000000000000, 1.000000000000000000),
 ( 0.9956975270656954757, 0.8568959468854893125),
 ( 0.9956975270656954757, 0.8568959468854893125),
 ( 1.000000000000000000, 1.000000000000000000) ) ) 
 REPRESENTATION_ITEM ( '' )  SURFACE ( )  );
#589 = CIRCLE ( 'NONE', #19894, 12.50000000000000000 ) ;
#591 = CARTESIAN_POINT ( 'NONE',  ( 9.884929003653626367, -50.49804566712026599, -141.8132360130362883 ) ) ;
#592 = CARTESIAN_POINT ( 'NONE',  ( 5.340103579038268045, 43.36842539899559767, -140.9275371836307613 ) ) ;
#593 = FACE_OUTER_BOUND ( 'NONE', #4583, .T. ) ;
#594 = VECTOR ( 'NONE', #26291, 1000.000000000000000 ) ;
#595 = ADVANCED_FACE ( 'NONE', ( #18838 ), #19043, .F. ) ;
#596 = FACE_OUTER_BOUND ( 'NONE', #16790, .T. ) ;
#597 = CARTESIAN_POINT ( 'NONE',  ( -4.162674018437132695, -41.48630000627035486, 25.90909455705156006 ) ) ;
#598 = CARTESIAN_POINT ( 'NONE',  ( 13.36082413113063083, 109.3026516754246558, -106.9547846563624773 ) ) ;
#599 = EDGE_CURVE ( 'NONE', #14659, #15269, #12220, .T. ) ;
#600 = VERTEX_POINT ( 'NONE', #5452 ) ;
#601 = DIRECTION ( 'NONE',  ( 0.000000000000000000, 0.000000000000000000, 1.000000000000000000 ) ) ;
#602 = CARTESIAN_POINT ( 'NONE',  ( -1.048994561756802169, 45.79144455904140898, 0.7655149579825029083 ) ) ;
#603 = B_SPLINE_CURVE_WITH_KNOTS ( 'NONE', 3,
 ( #15031, #8290, #3829, #25855, #6149, #12737 ),
 .UNSPECIFIED., .F., .F.,
 ( 4, 2, 4 ),
 ( 5.898697549827395015E-18, 0.0006311636237756845487, 0.001262327247551363243 ),
 .UNSPECIFIED. ) ;
#604 = VERTEX_POINT ( 'NONE', #5604 ) ;
#605 = CONICAL_SURFACE ( 'NONE', #20816, 151.1787379149930359, 0.5880026024245678107 ) ;
#606 = ORIENTED_EDGE ( 'NONE', *, *, #15154, .F. ) ;
#607 = VERTEX_POINT ( 'NONE', #25482 ) ;
#608 = DIRECTION ( 'NONE',  ( 0.000000000000000000, 5.223019709707975211E-21, -1.000000000000000000 ) ) ;
#609 = LINE ( 'NONE', #20463, #14259 ) ;
#610 = AXIS2_PLACEMENT_3D ( 'NONE', #8684, #19070, #1914 ) ;
#611 = CARTESIAN_POINT ( 'NONE',  ( -55.24271866751342941, 0.009388511352200527849, -0.001425019990779188969 ) ) ;
#612 = CARTESIAN_POINT ( 'NONE',  ( 10.93730112725972781, -71.28103789255033007, 133.3192575531796251 ) ) ;
#613 = CIRCLE ( 'NONE', #154, 20.00000000000000000 ) ;
#614 = FACE_BOUND ( 'NONE', #9901, .T. ) ;
#615 = CARTESIAN_POINT ( 'NONE',  ( 26.11404676487257603, -107.3263591096427945, -36.06104232266560672 ) ) ;
#616 = DIRECTION ( 'NONE',  ( -1.000000000000000000, -0.000000000000000000, -0.000000000000000000 ) ) ;
#617 = CARTESIAN_POINT ( 'NONE',  ( 25.64699802086724389, 112.2675771984165891, -12.03888878460358391 ) ) ;
#618 = CARTESIAN_POINT ( 'NONE',  ( 1.833485406944057594, 132.7804117027888253, 58.53321471326925263 ) ) ;
#619 = EDGE_CURVE ( 'NONE', #10772, #4669, #18254, .T. ) ;
#620 = B_SPLINE_CURVE_WITH_KNOTS ( 'NONE', 3,
 ( #10934, #14824, #28333, #23637, #19426, #23909, #17396, #19697, #14681, #26184, #16985, #24049, #3750 ),
 .UNSPECIFIED., .F., .F.,
 ( 4, 3, 3, 3, 4 ),
 ( 9.813077866773594792E-18, 0.0007657099931970658743, 0.001531419946797928045, 0.002296279302920156435, 0.003061450627205745956 ),
 .UNSPECIFIED. ) ;
#621 = CARTESIAN_POINT ( 'NONE',  ( 2.433796855181205476, -31.67151202413066713, 142.0211193075554945 ) ) ;
#622 = CARTESIAN_POINT ( 'NONE',  ( 1.833485406944057594, 59.50871042846225834, 132.3460930279893262 ) ) ;
#623 = CARTESIAN_POINT ( 'NONE',  ( 109.1592201516379674, 0.001331853079201392653, -0.007748443302134886378 ) ) ;
#624 = CARTESIAN_POINT ( 'NONE',  ( 25.64681081121880624, -23.88203588908156760, 110.3564950173080916 ) ) ;
#625 =( BOUNDED_SURFACE ( )  B_SPLINE_SURFACE ( 3, 1, ( 
 ( #16688, #27896 ),
 ( #10072, #14794 ),
 ( #25481, #19255 ),
 ( #7780, #16955 ) ),
 .UNSPECIFIED., .F., .F., .F. ) 
 B_SPLINE_SURFACE_WITH_KNOTS ( ( 4, 4 ),
 ( 2, 2 ),
 ( 0.000000000000000000, 1.000000000000000000 ),
 ( 0.000000000000000000, 1.000000000000000000 ),
 .UNSPECIFIED. ) 
 GEOMETRIC_REPRESENTATION_ITEM ( )  RATIONAL_B_SPLINE_SURFACE ( (
 ( 1.000000000000000000, 1.000000000000000000),
 ( 0.7789835883360578528, 0.9689951854195403280),
 ( 0.7789835883360578528, 0.9689951854195403280),
 ( 1.000000000000000000, 1.000000000000000000) ) ) 
 REPRESENTATION_ITEM ( '' )  SURFACE ( )  );
#627 = ORIENTED_EDGE ( 'NONE', *, *, #8785, .T. ) ;
#626 = EDGE_CURVE ( 'NONE', #21463, #9601, #19292, .T. ) ;
#628 = FACE_OUTER_BOUND ( 'NONE', #11290, .T. ) ;
#629 = CARTESIAN_POINT ( 'NONE',  ( -55.24271866751342941, -0.004365563123939050251, 0.008433070970613824532 ) ) ;
#630 = CARTESIAN_POINT ( 'NONE',  ( 16.75465622695655199, 87.30527857298585559, -112.2763423369171107 ) ) ;
#631 = CARTESIAN_POINT ( 'NONE',  ( 30.59141879584321799, 101.9665761624300728, -55.75104644134783172 ) ) ;
#632 = CARTESIAN_POINT ( 'NONE',  ( -1.058473599757814521, 15.81436910992580991, 42.99101666105212161 ) ) ;
#633 = ORIENTED_EDGE ( 'NONE', *, *, #20499, .F. ) ;
#634 = ORIENTED_EDGE ( 'NONE', *, *, #20397, .T. ) ;
#635 = DIRECTION ( 'NONE',  ( 1.000000000000000000, -6.938893903907226837E-18, 1.734723475976806709E-18 ) ) ;
#636 = CARTESIAN_POINT ( 'NONE',  ( 25.65782528836479770, -12.37768345530052905, 112.2379831684172302 ) ) ;
#637 = ORIENTED_EDGE ( 'NONE', *, *, #19856, .F. ) ;
#638 = CARTESIAN_POINT ( 'NONE',  ( -1.539760825549682410, -29.16712717142786460, -35.94320866319479535 ) ) ;
#639 = ORIENTED_EDGE ( 'NONE', *, *, #20990, .T. ) ;
#640 = CARTESIAN_POINT ( 'NONE',  ( 30.59141879584291956, -99.26511058698852707, -60.43012207291066318 ) ) ;
#641 = ORIENTED_EDGE ( 'NONE', *, *, #26722, .T. ) ;
#642 = EDGE_LOOP ( 'NONE', ( #20424, #21101, #20237, #10246 ) ) ;
#643 = CYLINDRICAL_SURFACE ( 'NONE', #10147, 12.50000000000000000 ) ;
#644 = CARTESIAN_POINT ( 'NONE',  ( -15.02187109954784106, 45.60876405941888123, -8.264310930412539946 ) ) ;
#645 = LINE ( 'NONE', #22976, #13807 ) ;
#646 = CARTESIAN_POINT ( 'NONE',  ( -25.21435515916043002, 4.655591116594353984, -34.29329011225956947 ) ) ;
#647 = CARTESIAN_POINT ( 'NONE',  ( -55.24271866751342941, 0.008488649505343330570, 0.004256484107795472684 ) ) ;
#648 = EDGE_CURVE ( 'NONE', #3159, #8671, #4487, .T. ) ;
#649 = B_SPLINE_CURVE_WITH_KNOTS ( 'NONE', 3,
 ( #20292, #9647, #11812, #722, #22472, #5322, #13667, #27341, #11664, #7351 ),
 .UNSPECIFIED., .F., .F.,
 ( 4, 3, 3, 4 ),
 ( 2.501853776554200607E-17, 0.0002669560319015759414, 0.0005492286108966312622, 0.0008315040496093394767 ),
 .UNSPECIFIED. ) ;
#650 = CARTESIAN_POINT ( 'NONE',  ( -24.53239521893645048, 22.94500969220232633, -24.99972072650149713 ) ) ;
#651 = CARTESIAN_POINT ( 'NONE',  ( -1.048994561756802391, 27.53485040342894408, -36.59609844253136401 ) ) ;
#652 = CARTESIAN_POINT ( 'NONE',  ( 25.86096068574580542, 83.34468010038291652, 76.38617895399373481 ) ) ;
#653 = EDGE_CURVE ( 'NONE', #28198, #2053, #6600, .T. ) ;
#654 = VERTEX_POINT ( 'NONE', #3441 ) ;
#655 = CARTESIAN_POINT ( 'NONE',  ( -16.86833981943426153, -20.94590537750580239, 38.94907963570745579 ) ) ;
#657 = CARTESIAN_POINT ( 'NONE',  ( -2.911734481061403645, 17.36785190846042681, 44.38410240830284437 ) ) ;
#656 = CARTESIAN_POINT ( 'NONE',  ( 55.49584447822657296, 72.12568090333353155, -7.849835876627591524 ) ) ;
#658 = ADVANCED_FACE ( 'NONE', ( #5307 ), #7111, .F. ) ;
#659 = CARTESIAN_POINT ( 'NONE',  ( -1.619063947482197729, -43.26576862488445130, -16.67502769180545386 ) ) ;
#660 = CARTESIAN_POINT ( 'NONE',  ( 1.833485406944043827, 138.1714136985314383, -44.33323125129781772 ) ) ;
#661 = EDGE_LOOP ( 'NONE', ( #13887, #8286, #21471, #8177 ) ) ;
#662 = ORIENTED_EDGE ( 'NONE', *, *, #9978, .F. ) ;
#663 = CARTESIAN_POINT ( 'NONE',  ( 109.1586900883932856, -0.005371970278523999220, 0.004701023939953835606 ) ) ;
#664 = CARTESIAN_POINT ( 'NONE',  ( 109.1586900883932856, -0.007002774699553650055, 0.001385221016536926190 ) ) ;
#665 = CARTESIAN_POINT ( 'NONE',  ( 109.1721716018069515, 0.01254847260354035460, 0.01157047143378742843 ) ) ;
#666 = CARTESIAN_POINT ( 'NONE',  ( 25.64681081121879203, 110.3564950173084895, -23.88203588907973085 ) ) ;
#667 = ORIENTED_EDGE ( 'NONE', *, *, #20614, .T. ) ;
#668 =( BOUNDED_SURFACE ( )  B_SPLINE_SURFACE ( 3, 1, ( 
 ( #9433, #12157 ),
 ( #16468, #784 ),
 ( #1213, #25259 ),
 ( #27255, #3373 ) ),
 .UNSPECIFIED., .F., .F., .F. ) 
 B_SPLINE_SURFACE_WITH_KNOTS ( ( 4, 4 ),
 ( 2, 2 ),
 ( 0.000000000000000000, 1.000000000000000000 ),
 ( 0.000000000000000000, 1.000000000000000000 ),
 .UNSPECIFIED. ) 
 GEOMETRIC_REPRESENTATION_ITEM ( )  RATIONAL_B_SPLINE_SURFACE ( (
 ( 1.000000000000000000, 1.000000000000000000),
 ( 0.9956975270656955868, 0.8568959468854907557),
 ( 0.9956975270656955868, 0.8568959468854907557),
 ( 1.000000000000000000, 1.000000000000000000) ) ) 
 REPRESENTATION_ITEM ( '' )  SURFACE ( )  );
#669 = CARTESIAN_POINT ( 'NONE',  ( -22.23342874802670011, -31.55488258420090375, -2.180636882146402833 ) ) ;
#670 = EDGE_LOOP ( 'NONE', ( #19059, #14520, #8651, #23980 ) ) ;
#672 = EDGE_CURVE ( 'NONE', #14178, #9075, #27322, .T. ) ;
#671 = CARTESIAN_POINT ( 'NONE',  ( 8.186469829614464899, 143.0750865143074577, -42.84118568057052556 ) ) ;
#673 = ORIENTED_EDGE ( 'NONE', *, *, #10366, .F. ) ;
#674 = CARTESIAN_POINT ( 'NONE',  ( 109.1586059443104944, -0.006856640434645994327, -0.001740416220250450095 ) ) ;
#675 = VERTEX_POINT ( 'NONE', #1688 ) ;
#676 = EDGE_CURVE ( 'NONE', #6702, #27834, #5901, .T. ) ;
#677 = CARTESIAN_POINT ( 'NONE',  ( 16.75465622695643475, -125.4242432475199394, 67.05928661304321281 ) ) ;
#678 = DIRECTION ( 'NONE',  ( -1.000000000000000000, -0.000000000000000000, -0.000000000000000000 ) ) ;
#679 = DIRECTION ( 'NONE',  ( 1.000000000000000000, -6.938893903907226837E-18, 1.734723475976806709E-18 ) ) ;
#680 = CARTESIAN_POINT ( 'NONE',  ( 10.93730112725985926, -150.7858122213662853, 10.89264110824944609 ) ) ;
#681 = EDGE_CURVE ( 'NONE', #27239, #7066, #7645, .T. ) ;
#682 = ORIENTED_EDGE ( 'NONE', *, *, #14733, .T. ) ;
#683 = ADVANCED_FACE ( 'NONE', ( #1966 ), #21971, .F. ) ;
#684 = CARTESIAN_POINT ( 'NONE',  ( -20.57838717382308147, -7.715628353033481268, 28.96176188950225949 ) ) ;
#685 = CARTESIAN_POINT ( 'NONE',  ( 32.73300124599735739, 51.32617430724909013, 105.8473486001052777 ) ) ;
#686 = CARTESIAN_POINT ( 'NONE',  ( 24.01988960052036148, -111.2910478357999295, -69.18817751538435346 ) ) ;
#687 = ORIENTED_EDGE ( 'NONE', *, *, #26528, .T. ) ;
#688 = EDGE_LOOP ( 'NONE', ( #23009, #27097, #24333, #18034 ) ) ;
#689 = ORIENTED_EDGE ( 'NONE', *, *, #24280, .T. ) ;
#690 = FACE_OUTER_BOUND ( 'NONE', #725, .T. ) ;
#691 = CARTESIAN_POINT ( 'NONE',  ( 55.79472521941428198, 58.42842213658386896, -43.35047097963390428 ) ) ;
#693 = CARTESIAN_POINT ( 'NONE',  ( -55.24198130335446422, -0.008310594958150379491, -0.004163123460805868634 ) ) ;
#692 = CARTESIAN_POINT ( 'NONE',  ( 109.1589550718174877, 0.002553077953671612117, -0.007132058561965959158 ) ) ;
#694 = LINE ( 'NONE', #7473, #6923 ) ;
#695 = CARTESIAN_POINT ( 'NONE',  ( 32.73300124599738581, 8.473903470907664826, -117.3295799645428588 ) ) ;
#696 = CARTESIAN_POINT ( 'NONE',  ( -7.733045908741326357, -51.44704017882769875, 10.42750254442592706 ) ) ;
#697 = ORIENTED_EDGE ( 'NONE', *, *, #27504, .F. ) ;
#698 = CARTESIAN_POINT ( 'NONE',  ( 1.832998868059858122, -142.0492247521720799, -29.64765804470217958 ) ) ;
#699 = CARTESIAN_POINT ( 'NONE',  ( -1.259972190295303385, -16.33417789844404666, -43.01178231151323672 ) ) ;
#700 = CARTESIAN_POINT ( 'NONE',  ( 25.64681081121879203, -0.4157506337735756285, 112.9102952884414464 ) ) ;
#701 = CARTESIAN_POINT ( 'NONE',  ( 2.430230287190581429, -74.01081053031187196, 125.2872625092160064 ) ) ;
#702 = CARTESIAN_POINT ( 'NONE',  ( 109.1586059443104944, 0.003930911098385077469, -0.005881369279880109546 ) ) ;
#703 = CARTESIAN_POINT ( 'NONE',  ( 25.73574536432417048, 102.8730547980549659, 46.68445899255523557 ) ) ;
#704 = VERTEX_POINT ( 'NONE', #10621 ) ;
#705 = LINE ( 'NONE', #26893, #20384 ) ;
#706 = EDGE_LOOP ( 'NONE', ( #2799, #7129, #15020, #177, #14414, #23981 ) ) ;
#707 = CARTESIAN_POINT ( 'NONE',  ( 1.833838850093465034, -30.17001957361884124, -141.9387658801234124 ) ) ;
#708 = FACE_OUTER_BOUND ( 'NONE', #2088, .T. ) ;
#709 = VERTEX_POINT ( 'NONE', #26019 ) ;
#710 = VERTEX_POINT ( 'NONE', #21415 ) ;
#711 = VERTEX_POINT ( 'NONE', #19533 ) ;
#712 = CARTESIAN_POINT ( 'NONE',  ( 10.93730112725996051, -4.928439153519255989, -151.0983828010092793 ) ) ;
#713 = EDGE_CURVE ( 'NONE', #12372, #246, #28206, .T. ) ;
#714 = VECTOR ( 'NONE', #2936, 1000.000000000000000 ) ;
#715 = CARTESIAN_POINT ( 'NONE',  ( 2.430230287190592531, 138.8342928068220203, 43.58368230469437776 ) ) ;
#716 = EDGE_CURVE ( 'NONE', #21261, #24227, #66, .T. ) ;
#717 = LINE ( 'NONE', #26759, #22695 ) ;
#718 = LINE ( 'NONE', #9508, #7650 ) ;
#719 = ORIENTED_EDGE ( 'NONE', *, *, #1749, .T. ) ;
#720 = CARTESIAN_POINT ( 'NONE',  ( -1.031422197589711987, 28.14735071801795740, 36.13727897780095333 ) ) ;
#721 = EDGE_CURVE ( 'NONE', #1061, #823, #15129, .T. ) ;
#722 = CARTESIAN_POINT ( 'NONE',  ( 25.64703792032470631, -103.0889146124068532, 46.06101937225569287 ) ) ;
#723 = CARTESIAN_POINT ( 'NONE',  ( -1.045287976400365970, -45.76855895860947498, -1.530335034933654859 ) ) ;
#724 = ORIENTED_EDGE ( 'NONE', *, *, #20732, .F. ) ;
#725 = EDGE_LOOP ( 'NONE', ( #2704, #27015 ) ) ;
#726 = CARTESIAN_POINT ( 'NONE',  ( -1.048994561756802169, -43.31369460697986540, -14.87838255483240246 ) ) ;
#727 = CARTESIAN_POINT ( 'NONE',  ( 25.64708010899964208, -45.97512510001836006, -103.1273237223354187 ) ) ;
#728 = CARTESIAN_POINT ( 'NONE',  ( -20.57838717382308147, 16.28767523336157552, 25.16001208503087838 ) ) ;
#729 = CARTESIAN_POINT ( 'NONE',  ( 1.833206308920081407, 96.54250175814114243, 108.3342547309368484 ) ) ;
#730 = B_SPLINE_CURVE_WITH_KNOTS ( 'NONE', 3,
 ( #20327, #11407, #25094, #11985, #18163, #20756 ),
 .UNSPECIFIED., .F., .F.,
 ( 4, 2, 4 ),
 ( 1.389302603484999005E-17, 0.0006311571484586055722, 0.001262314296917197484 ),
 .UNSPECIFIED. ) ;
#731 = FACE_OUTER_BOUND ( 'NONE', #16382, .T. ) ;
#732 = B_SPLINE_CURVE_WITH_KNOTS ( 'NONE', 3,
 ( #22479, #26914, #2448, #11240, #9083, #4764 ),
 .UNSPECIFIED., .F., .F.,
 ( 4, 2, 4 ),
 ( 1.852685484479510670E-17, 0.0006311636237756926802, 0.001262327247551366495 ),
 .UNSPECIFIED. ) ;
#733 = VERTEX_POINT ( 'NONE', #24017 ) ;
#734 = CARTESIAN_POINT ( 'NONE',  ( 25.64681081121879203, 46.30456157731328659, 102.9795863647030103 ) ) ;
#735 = CARTESIAN_POINT ( 'NONE',  ( 5.340103579038250281, -32.90561047415497598, -143.7310399932981397 ) ) ;
#736 = CARTESIAN_POINT ( 'NONE',  ( -1.239374126674604337, -16.50008610789269170, 42.99367564261294206 ) ) ;
#737 = CARTESIAN_POINT ( 'NONE',  ( 25.64681081121879203, -75.86069728269045243, 83.63051021305875565 ) ) ;
#738 = CARTESIAN_POINT ( 'NONE',  ( 25.69398547355839924, -0.7422864227357194311, -112.9401428107247369 ) ) ;
#739 = EDGE_LOOP ( 'NONE', ( #19600, #26923, #1375, #15922 ) ) ;
#740 = ORIENTED_EDGE ( 'NONE', *, *, #14373, .T. ) ;
#741 = CARTESIAN_POINT ( 'NONE',  ( 26.04756280548352976, -57.54844730865598734, -97.45505646068890826 ) ) ;
#742 = ORIENTED_EDGE ( 'NONE', *, *, #24451, .T. ) ;
#743 = ORIENTED_EDGE ( 'NONE', *, *, #24981, .F. ) ;
#744 = VERTEX_POINT ( 'NONE', #16956 ) ;
#745 = CARTESIAN_POINT ( 'NONE',  ( -1.048171036023497260, 37.64178826568608116, -26.08692787913882327 ) ) ;
#746 = EDGE_CURVE ( 'NONE', #14753, #8031, #12746, .T. ) ;
#747 = SHAPE_REPRESENTATION ( 'pinion', ( #27263 ), #6137 ) ;
#748 = EDGE_CURVE ( 'NONE', #11307, #9768, #22724, .T. ) ;
#749 = CARTESIAN_POINT ( 'NONE',  ( -25.21435515916043357, 16.39063784838743132, -30.48034229288645136 ) ) ;
#750 = FACE_OUTER_BOUND ( 'NONE', #3616, .T. ) ;
#751 = ADVANCED_FACE ( 'NONE', ( #24729 ), #17387, .T. ) ;
#752 = FACE_OUTER_BOUND ( 'NONE', #21378, .T. ) ;
#753 = CARTESIAN_POINT ( 'NONE',  ( -4.780792508754321268, 25.98388465890140964, 42.16805077400930202 ) ) ;
#754 =( BOUNDED_SURFACE ( )  B_SPLINE_SURFACE ( 3, 1, ( 
 ( #5912, #7944 ),
 ( #27908, #14668 ),
 ( #28042, #8347 ),
 ( #23761, #21145 ) ),
 .UNSPECIFIED., .F., .F., .F. ) 
 B_SPLINE_SURFACE_WITH_KNOTS ( ( 4, 4 ),
 ( 2, 2 ),
 ( 0.000000000000000000, 1.000000000000000000 ),
 ( 0.000000000000000000, 1.000000000000000000 ),
 .UNSPECIFIED. ) 
 GEOMETRIC_REPRESENTATION_ITEM ( )  RATIONAL_B_SPLINE_SURFACE ( (
 ( 1.000000000000000000, 1.000000000000000000),
 ( 0.9960225298536222738, 0.9999952330161893110),
 ( 0.9960225298536222738, 0.9999952330161893110),
 ( 1.000000000000000000, 1.000000000000000000) ) ) 
 REPRESENTATION_ITEM ( '' )  SURFACE ( )  );
#755 = EDGE_CURVE ( 'NONE', #14003, #2917, #5214, .T. ) ;
#756 = CARTESIAN_POINT ( 'NONE',  ( -23.77929240705207192, -35.68044874544700207, -6.464423883190233866 ) ) ;
#757 = CARTESIAN_POINT ( 'NONE',  ( 25.73574536432414561, -35.67555431182906744, 107.1893601970593863 ) ) ;
#758 = DIRECTION ( 'NONE',  ( -0.7563875759206388771, -0.03500244528123461207, -0.6531865459554673237 ) ) ;
#759 = FACE_OUTER_BOUND ( 'NONE', #1679, .T. ) ;
#760 = CARTESIAN_POINT ( 'NONE',  ( -12.94347594948480662, 35.22469990145658159, 33.69581619287838947 ) ) ;
#761 = CARTESIAN_POINT ( 'NONE',  ( 1.833485406944043827, 117.0814567582556407, -85.72460230293573602 ) ) ;
#762 = CARTESIAN_POINT ( 'NONE',  ( 25.70243777736190438, -55.83795591307065109, -98.18050844655130049 ) ) ;
#764 = CARTESIAN_POINT ( 'NONE',  ( -28.41354790283022069, -8.345538364877233661, -21.64275480268745255 ) ) ;
#763 = CARTESIAN_POINT ( 'NONE',  ( -18.41936578851709072, 7.566034416291376630, 41.75701384111728487 ) ) ;
#765 = FACE_OUTER_BOUND ( 'NONE', #8133, .T. ) ;
#766 = CARTESIAN_POINT ( 'NONE',  ( -1.046936909428682672, -36.28616897897433091, 27.93981068760662012 ) ) ;
#767 = CARTESIAN_POINT ( 'NONE',  ( 26.11404676487257603, 65.63269960453241936, 92.25884714080432047 ) ) ;
#768 = CARTESIAN_POINT ( 'NONE',  ( -1.045287976400365970, 15.59869763335156101, 43.05558670614217931 ) ) ;
#769 = ORIENTED_EDGE ( 'NONE', *, *, #5904, .T. ) ;
#770 = CARTESIAN_POINT ( 'NONE',  ( -55.24390624410018802, 0.004896917417128144288, 0.009209468562451129242 ) ) ;
#771 = VERTEX_POINT ( 'NONE', #9316 ) ;
#772 = CARTESIAN_POINT ( 'NONE',  ( 109.1587776205901861, -0.005978137617721869003, -0.004240403845331854223 ) ) ;
#773 = B_SPLINE_CURVE_WITH_KNOTS ( 'NONE', 3,
 ( #27875, #7903, #16664, #25460, #5733, #19103, #8173 ),
 .UNSPECIFIED., .F., .F.,
 ( 4, 3, 4 ),
 ( 4.967492064660139599E-16, 0.02816610861753249262, 0.04000277880656270824 ),
 .UNSPECIFIED. ) ;
#774 = DIRECTION ( 'NONE',  ( -1.000000000000000000, -0.000000000000000000, -0.000000000000000000 ) ) ;
#775 = ORIENTED_EDGE ( 'NONE', *, *, #11570, .F. ) ;
#776 = ORIENTED_EDGE ( 'NONE', *, *, #21780, .F. ) ;
#777 = EDGE_LOOP ( 'NONE', ( #11721, #1209, #5595, #9182 ) ) ;
#778 = EDGE_CURVE ( 'NONE', #20282, #13345, #21328, .T. ) ;
#779 = B_SPLINE_CURVE_WITH_KNOTS ( 'NONE', 3,
 ( #26938, #7250, #16003, #22359 ),
 .UNSPECIFIED., .F., .F.,
 ( 4, 4 ),
 ( 2.248458606249288556E-16, 0.008383748772659682658 ),
 .UNSPECIFIED. ) ;
#780 = EDGE_CURVE ( 'NONE', #9272, #4028, #15485, .T. ) ;
#781 = ORIENTED_EDGE ( 'NONE', *, *, #28040, .F. ) ;
#782 = CARTESIAN_POINT ( 'NONE',  ( 109.1778270068192853, 0.009307953841262543021, 0.0003511581237570110558 ) ) ;
#783 = ADVANCED_FACE ( 'NONE', ( #6867 ), #2280, .F. ) ;
#784 = CARTESIAN_POINT ( 'NONE',  ( 1.831572820252008738, -16.14965423926307153, 144.2101521542829801 ) ) ;
#785 = CARTESIAN_POINT ( 'NONE',  ( -1.049819825607592794, -14.63675055554412374, -43.39756533277876827 ) ) ;
#786 = CARTESIAN_POINT ( 'NONE',  ( -8.259864102781680373, 47.98931516265592734, -22.52209142944943565 ) ) ;
#787 =( BOUNDED_SURFACE ( )  B_SPLINE_SURFACE ( 3, 1, ( 
 ( #2630, #26655 ),
 ( #16010, #2481 ),
 ( #8981, #16158 ),
 ( #17741, #18022 ) ),
 .UNSPECIFIED., .F., .F., .F. ) 
 B_SPLINE_SURFACE_WITH_KNOTS ( ( 4, 4 ),
 ( 2, 2 ),
 ( 0.000000000000000000, 1.000000000000000000 ),
 ( 0.000000000000000000, 1.000000000000000000 ),
 .UNSPECIFIED. ) 
 GEOMETRIC_REPRESENTATION_ITEM ( )  RATIONAL_B_SPLINE_SURFACE ( (
 ( 1.000000000000000000, 1.000000000000000000),
 ( 0.9960225298536222738, 0.9999952330161893110),
 ( 0.9960225298536222738, 0.9999952330161893110),
 ( 1.000000000000000000, 1.000000000000000000) ) ) 
 REPRESENTATION_ITEM ( '' )  SURFACE ( )  );
#788 = CARTESIAN_POINT ( 'NONE',  ( 109.1624594426973260, 0.01216903288310108508, -0.01033277910988601375 ) ) ;
#789 = CARTESIAN_POINT ( 'NONE',  ( -25.21435515916043713, -34.05351380035328646, 6.169479169075816394 ) ) ;
#790 = CARTESIAN_POINT ( 'NONE',  ( 1.832998868059890096, 107.4798986104860319, 97.49378069860830465 ) ) ;
#791 = DIRECTION ( 'NONE',  ( 0.5946245182733607137, -0.5357871896547450330, -0.5994612328333200901 ) ) ;
#792 = CARTESIAN_POINT ( 'NONE',  ( 25.64681081121879203, -34.49579773461859133, 107.5125461021401492 ) ) ;
#793 = CARTESIAN_POINT ( 'NONE',  ( 109.1586900883932856, 0.003656351050331851926, 0.006130969560687375870 ) ) ;
#794 = EDGE_LOOP ( 'NONE', ( #6516, #11457 ) ) ;
#795 = ORIENTED_EDGE ( 'NONE', *, *, #1305, .T. ) ;
#796 = CARTESIAN_POINT ( 'NONE',  ( 119.2224693531408803, 90.00000000000005684, -40.00000000000000711 ) ) ;
#798 = LINE ( 'NONE', #7286, #16006 ) ;
#797 = CARTESIAN_POINT ( 'NONE',  ( -1.239374126674604337, -35.79060836339833429, -28.97829083655425819 ) ) ;
#799 = CARTESIAN_POINT ( 'NONE',  ( -6.588769196390767746, -51.10255870850473769, -4.956336548259470121 ) ) ;
#800 = CARTESIAN_POINT ( 'NONE',  ( -16.86833981943424376, -43.82216161736207738, 5.948101187262031964 ) ) ;
#801 = CARTESIAN_POINT ( 'NONE',  ( -55.25297051322618813, 0.01466904165775178431, 0.002853887643042449414 ) ) ;
#802 = ORIENTED_EDGE ( 'NONE', *, *, #17983, .T. ) ;
#803 = CARTESIAN_POINT ( 'NONE',  ( 24.22246935314087324, 69.99999999999998579, -40.00000000000000711 ) ) ;
#804 = B_SPLINE_CURVE_WITH_KNOTS ( 'NONE', 3,
 ( #21480, #25810, #25951, #14578, #4198, #14991 ),
 .UNSPECIFIED., .F., .F.,
 ( 4, 2, 4 ),
 ( 1.396102177145585797E-16, 0.003570751334075631788, 0.007141502668151123931 ),
 .UNSPECIFIED. ) ;
#805 = CARTESIAN_POINT ( 'NONE',  ( 109.1589550718174877, 0.007553890059312246691, -0.0005685167901298649948 ) ) ;
#806 = CARTESIAN_POINT ( 'NONE',  ( 9.884929003653626367, -85.04731144912598495, 124.2095058357574544 ) ) ;
#807 = ORIENTED_EDGE ( 'NONE', *, *, #23491, .F. ) ;
#808 = CARTESIAN_POINT ( 'NONE',  ( -55.24390624410018802, 0.009209468562451588944, -0.004896917417127890151 ) ) ;
#809 = EDGE_LOOP ( 'NONE', ( #28304, #26897 ) ) ;
#810 = CARTESIAN_POINT ( 'NONE',  ( 32.73300124599737160, -84.80615050150427692, 81.52272205837169849 ) ) ;
#811 = FACE_OUTER_BOUND ( 'NONE', #27029, .T. ) ;
#812 = ADVANCED_FACE ( 'NONE', ( #26429 ), #24939, .F. ) ;
#813 = VERTEX_POINT ( 'NONE', #24432 ) ;
#814 = ORIENTED_EDGE ( 'NONE', *, *, #21780, .T. ) ;
#815 = EDGE_CURVE ( 'NONE', #20966, #16465, #11181, .T. ) ;
#816 = CARTESIAN_POINT ( 'NONE',  ( -55.24390624410018802, -0.004896917417131185259, 0.009209468562452437224 ) ) ;
#817 = EDGE_LOOP ( 'NONE', ( #4201, #23942, #19669, #10493 ) ) ;
#818 = EDGE_CURVE ( 'NONE', #2385, #24314, #8998, .T. ) ;
#819 = CARTESIAN_POINT ( 'NONE',  ( 32.73300124599735739, -103.7392577722179823, 55.46353551261974957 ) ) ;
#820 = B_SPLINE_CURVE_WITH_KNOTS ( 'NONE', 3,
 ( #26367, #13402, #6669, #22352, #26505, #15555 ),
 .UNSPECIFIED., .F., .F.,
 ( 4, 2, 4 ),
 ( 0.000000000000000000, 0.0004335184443140219679, 0.0008670368886280439358 ),
 .UNSPECIFIED. ) ;
#821 = CARTESIAN_POINT ( 'NONE',  ( 25.64703792032469920, 107.3388703233126904, -35.03296646432450245 ) ) ;
#822 = CARTESIAN_POINT ( 'NONE',  ( 1.833838850093440165, -125.6687394363102896, 72.55488452980823411 ) ) ;
#823 = VERTEX_POINT ( 'NONE', #26563 ) ;
#824 = CARTESIAN_POINT ( 'NONE',  ( 5.340103556456459621, -32.90561046456809180, 143.7310399800116727 ) ) ;
#825 = CARTESIAN_POINT ( 'NONE',  ( 25.69398547355838858, 34.19446713634726365, -107.6418378907640943 ) ) ;
#826 = CARTESIAN_POINT ( 'NONE',  ( 10.93730112725971715, -20.69552240458431314, 149.7554878793147282 ) ) ;
#827 = ORIENTED_EDGE ( 'NONE', *, *, #2766, .F. ) ;
#828 = ORIENTED_EDGE ( 'NONE', *, *, #20094, .T. ) ;
#829 = ORIENTED_EDGE ( 'NONE', *, *, #16054, .F. ) ;
#830 = LINE ( 'NONE', #20840, #2333 ) ;
#831 = FACE_OUTER_BOUND ( 'NONE', #22609, .T. ) ;
#833 = CARTESIAN_POINT ( 'NONE',  ( 25.64704443564074765, 11.93517308299288082, -112.2786464378872751 ) ) ;
#832 = CARTESIAN_POINT ( 'NONE',  ( 30.59141879584283075, 9.457572341076559752, 115.8270959620728320 ) ) ;
#834 = CARTESIAN_POINT ( 'NONE',  ( -1.050230346682677007, 0.0006945978175690684661, -45.79907861045643358 ) ) ;
#835 = CARTESIAN_POINT ( 'NONE',  ( 1.833691583653549229, 144.2771263798446455, 15.52203496788964365 ) ) ;
#836 = DIRECTION ( 'NONE',  ( 0.7563875759206388771, -0.5078650950445684487, -0.4122509917856733708 ) ) ;
#837 =( BOUNDED_SURFACE ( )  B_SPLINE_SURFACE ( 3, 1, ( 
 ( #9543, #18295 ),
 ( #16154, #23664 ),
 ( #14702, #21473 ),
 ( #10543, #25672 ) ),
 .UNSPECIFIED., .F., .F., .F. ) 
 B_SPLINE_SURFACE_WITH_KNOTS ( ( 4, 4 ),
 ( 2, 2 ),
 ( 0.000000000000000000, 1.000000000000000000 ),
 ( 0.000000000000000000, 1.000000000000000000 ),
 .UNSPECIFIED. ) 
 GEOMETRIC_REPRESENTATION_ITEM ( )  RATIONAL_B_SPLINE_SURFACE ( (
 ( 1.000000000000000000, 1.000000000000000000),
 ( 0.9960225298536222738, 0.9999952330161893110),
 ( 0.9960225298536222738, 0.9999952330161893110),
 ( 1.000000000000000000, 1.000000000000000000) ) ) 
 REPRESENTATION_ITEM ( '' )  SURFACE ( )  );
#838 = CARTESIAN_POINT ( 'NONE',  ( -2.265401668238153032, -45.46007138824032978, 11.98901689611089516 ) ) ;
#839 = ORIENTED_EDGE ( 'NONE', *, *, #3305, .T. ) ;
#840 = CARTESIAN_POINT ( 'NONE',  ( -20.21097721650785672, -29.61001326827676294, 0.3305964462500739498 ) ) ;
#841 = CARTESIAN_POINT ( 'NONE',  ( -1.031422197589711987, -37.93675465142491277, -25.67058493451428802 ) ) ;
#842 = CARTESIAN_POINT ( 'NONE',  ( -1.045287976400351981, 12.68782741917293855, -44.00138577190654132 ) ) ;
#843 = CARTESIAN_POINT ( 'NONE',  ( 9.884929003653608603, 103.8128997986872690, -109.0134320167722137 ) ) ;
#844 = CARTESIAN_POINT ( 'NONE',  ( 28.37599760073042532, -48.29934869928239749, 104.0705811520812460 ) ) ;
#845 = PRODUCT_RELATED_PRODUCT_CATEGORY ( 'part', '', ( #32 ) ) ;
#846 = CARTESIAN_POINT ( 'NONE',  ( 16.05277956358235869, 132.7473359121861165, 53.98852998724608909 ) ) ;
#847 = LINE ( 'NONE', #11934, #6608 ) ;
#848 = CARTESIAN_POINT ( 'NONE',  ( -12.94347594948482971, 47.96504705787755540, -8.691477019903484091 ) ) ;
#850 = FACE_OUTER_BOUND ( 'NONE', #1927, .T. ) ;
#849 = B_SPLINE_CURVE_WITH_KNOTS ( 'NONE', 3,
 ( #13988, #5213, #7380, #18743, #3201, #14264 ),
 .UNSPECIFIED., .F., .F.,
 ( 4, 2, 4 ),
 ( 1.512296865354101973E-16, 0.003570751334075637860, 0.007141502668151123931 ),
 .UNSPECIFIED. ) ;
#851 = ORIENTED_EDGE ( 'NONE', *, *, #15279, .T. ) ;
#852 = EDGE_CURVE ( 'NONE', #19554, #24126, #4700, .T. ) ;
#853 = EDGE_LOOP ( 'NONE', ( #27414, #15523, #25287, #28098 ) ) ;
#854 = EDGE_LOOP ( 'NONE', ( #27943, #8561, #14969, #11566 ) ) ;
#855 = CARTESIAN_POINT ( 'NONE',  ( -1.050230346682680560, 45.79907861045643358, 0.0006945978177289460027 ) ) ;
#856 = CARTESIAN_POINT ( 'NONE',  ( 25.64703792032468854, -23.62108504469166803, -110.4127989088532900 ) ) ;
#857 = CARTESIAN_POINT ( 'NONE',  ( 13.36082413113063083, 147.2768864064167929, 41.18148072373664803 ) ) ;
#858 = AXIS2_PLACEMENT_3D ( 'NONE', #3079, #23101, #908 ) ;
#859 = CARTESIAN_POINT ( 'NONE',  ( -20.20612092514784308, 24.59769888281557471, 16.46550332780499559 ) ) ;
#860 = DIRECTION ( 'NONE',  ( 1.000000000000000000, -6.938893903907226837E-18, 1.734723475976806709E-18 ) ) ;
#861 = CARTESIAN_POINT ( 'NONE',  ( 2.108985857320903712, 13.91228467252010148, -144.6256801373125427 ) ) ;
#862 = CARTESIAN_POINT ( 'NONE',  ( 25.64681081121879203, 34.49579773461785948, 107.5125461021403765 ) ) ;
#863 = CARTESIAN_POINT ( 'NONE',  ( -28.13707043255157103, 22.00298671236740233, -6.342158660427079653 ) ) ;
#864 = VERTEX_POINT ( 'NONE', #18350 ) ;
#865 = ORIENTED_EDGE ( 'NONE', *, *, #5403, .T. ) ;
#866 = DIRECTION ( 'NONE',  ( 0.7637818620346800147, 0.2198041754873883424, -0.6068965246771037547 ) ) ;
#867 = CARTESIAN_POINT ( 'NONE',  ( -1.050231094221207417, -36.90262059116448512, 27.12595454131546191 ) ) ;
#868 = CARTESIAN_POINT ( 'NONE',  ( 109.1586900883932856, 0.006819617742893400482, 0.002109621908814826672 ) ) ;
#869 = DIRECTION ( 'NONE',  ( 0.000000000000000000, 0.000000000000000000, 1.000000000000000000 ) ) ;
#870 = CARTESIAN_POINT ( 'NONE',  ( 1.834118845439484335, -107.9567937753799782, 96.96525081349965092 ) ) ;
#871 = DIRECTION ( 'NONE',  ( 0.000000000000000000, 0.000000000000000000, -1.000000000000000000 ) ) ;
#872 = CARTESIAN_POINT ( 'NONE',  ( 1.831572820252009626, 142.1425225354579993, 29.20415387690616171 ) ) ;
#873 = EDGE_LOOP ( 'NONE', ( #20603, #6803, #23325, #21961 ) ) ;
#874 = DIRECTION ( 'NONE',  ( 1.000000000000000000, -6.938893903907226837E-18, 1.734723475976806709E-18 ) ) ;
#875 = CARTESIAN_POINT ( 'NONE',  ( 2.433796855181205476, 16.65276281464756636, -144.5536872373190533 ) ) ;
#876 =( BOUNDED_SURFACE ( )  B_SPLINE_SURFACE ( 3, 1, ( 
 ( #20704, #2871 ),
 ( #12085, #11649 ),
 ( #7783, #3301 ),
 ( #27177, #14082 ) ),
 .UNSPECIFIED., .F., .F., .F. ) 
 B_SPLINE_SURFACE_WITH_KNOTS ( ( 4, 4 ),
 ( 2, 2 ),
 ( 0.000000000000000000, 1.000000000000000000 ),
 ( 0.000000000000000000, 1.000000000000000000 ),
 .UNSPECIFIED. ) 
 GEOMETRIC_REPRESENTATION_ITEM ( )  RATIONAL_B_SPLINE_SURFACE ( (
 ( 1.000000000000000000, 1.000000000000000000),
 ( 0.9956975270656954757, 0.8568959468854893125),
 ( 0.9956975270656954757, 0.8568959468854893125),
 ( 1.000000000000000000, 1.000000000000000000) ) ) 
 REPRESENTATION_ITEM ( '' )  SURFACE ( )  );
#877 = CARTESIAN_POINT ( 'NONE',  ( 26.11404676487257603, -65.63269960453179408, -92.25884714080473259 ) ) ;
#878 = DIRECTION ( 'NONE',  ( -0.5914120900931443270, 0.6942916636548193132, -0.4101107478121997496 ) ) ;
#879 = CARTESIAN_POINT ( 'NONE',  ( 25.64692872815576408, -107.4838747185723378, 34.58541472378613690 ) ) ;
#880 = ADVANCED_FACE ( 'NONE', ( #16493 ), #5242, .F. ) ;
#881 = ORIENTED_EDGE ( 'NONE', *, *, #1372, .T. ) ;
#882 = ADVANCED_FACE ( 'NONE', ( #22853 ), #3615, .T. ) ;
#883 = ORIENTED_EDGE ( 'NONE', *, *, #26063, .T. ) ;
#884 = CARTESIAN_POINT ( 'NONE',  ( 26.28373643307407903, -105.5888781856746448, -71.57300207276496451 ) ) ;
#885 = ORIENTED_EDGE ( 'NONE', *, *, #27518, .F. ) ;
#886 = EDGE_CURVE ( 'NONE', #25087, #20633, #25492, .T. ) ;
#887 = B_SPLINE_CURVE_WITH_KNOTS ( 'NONE', 3,
 ( #21127, #14927, #20984, #3717 ),
 .UNSPECIFIED., .F., .F.,
 ( 4, 4 ),
 ( 3.469446951953614189E-18, 0.008383560773332729421 ),
 .UNSPECIFIED. ) ;
#888 = ORIENTED_EDGE ( 'NONE', *, *, #16125, .T. ) ;
#889 = ORIENTED_EDGE ( 'NONE', *, *, #8584, .F. ) ;
#890 = CARTESIAN_POINT ( 'NONE',  ( -1.239374126674604337, -35.79060836339793639, 28.97829083655478399 ) ) ;
#891 = CARTESIAN_POINT ( 'NONE',  ( 28.37644542392842695, 111.8804331835015233, 54.25112470585763447 ) ) ;
#892 = CARTESIAN_POINT ( 'NONE',  ( 2.063896406836605024, -144.6078654718903067, 13.84738934186143666 ) ) ;
#893 = CARTESIAN_POINT ( 'NONE',  ( 1.833485406944043827, -14.63699153649458040, 144.3694338680884641 ) ) ;
#894 = CARTESIAN_POINT ( 'NONE',  ( -25.21435515916043002, 4.655591116594353984, -34.29329011225956947 ) ) ;
#895 = EDGE_LOOP ( 'NONE', ( #11336, #3517, #24492, #9208 ) ) ;
#896 = DIRECTION ( 'NONE',  ( 1.000000000000000000, -6.938893903907226837E-18, 1.734723475976806709E-18 ) ) ;
#897 = FACE_OUTER_BOUND ( 'NONE', #24368, .T. ) ;
#898 = B_SPLINE_CURVE_WITH_KNOTS ( 'NONE', 3,
 ( #12919, #4423, #19967, #6193, #23893, #22132, #21854, #13195, #28315, #8480 ),
 .UNSPECIFIED., .F., .F.,
 ( 4, 2, 2, 2, 4 ),
 ( 1.563658610346375379E-18, 0.0003346267210630944644, 0.0006692534421261873024, 0.001003880163189280195, 0.001338506884252373087 ),
 .UNSPECIFIED. ) ;
#899 = DIRECTION ( 'NONE',  ( -1.000000000000000000, -0.000000000000000000, -0.000000000000000000 ) ) ;
#900 = CARTESIAN_POINT ( 'NONE',  ( -20.20700224038492365, -8.199606986804534259, -28.44216453106533748 ) ) ;
#901 = CARTESIAN_POINT ( 'NONE',  ( -8.786685647604894456, 37.00619870957989832, 38.68584556812258768 ) ) ;
#902 = DIRECTION ( 'NONE',  ( 0.000000000000000000, 0.000000000000000000, 1.000000000000000000 ) ) ;
#903 = ADVANCED_FACE ( 'NONE', ( #7296 ), #282, .F. ) ;
#904 = CARTESIAN_POINT ( 'NONE',  ( -21.41430102051751660, -25.94791611261628717, -16.60879216503625244 ) ) ;
#905 = CARTESIAN_POINT ( 'NONE',  ( -9.156249394959713683, -25.18996226954579498, 48.32878616081037393 ) ) ;
#906 = CARTESIAN_POINT ( 'NONE',  ( 109.1586900883932856, 0.006757191295060846481, 0.002301750759599797969 ) ) ;
#907 = CARTESIAN_POINT ( 'NONE',  ( 2.430230287190592531, -96.28466919684171899, 109.1043569252011025 ) ) ;
#908 = DIRECTION ( 'NONE',  ( 0.000000000000000000, 0.000000000000000000, 1.000000000000000000 ) ) ;
#909 = EDGE_CURVE ( 'NONE', #3564, #1317, #19633, .T. ) ;
#910 = ORIENTED_EDGE ( 'NONE', *, *, #5742, .F. ) ;
#911 = CARTESIAN_POINT ( 'NONE',  ( 109.1721716018069515, 0.001984900887706656826, -0.01695288006056419258 ) ) ;
#912 = ADVANCED_FACE ( 'NONE', ( #1233 ), #3229, .F. ) ;
#913 = ORIENTED_EDGE ( 'NONE', *, *, #10709, .F. ) ;
#914 = DIRECTION ( 'NONE',  ( 0.000000000000000000, 5.223019709707975211E-21, -1.000000000000000000 ) ) ;
#915 =( BOUNDED_SURFACE ( )  B_SPLINE_SURFACE ( 3, 1, ( 
 ( #18286, #24946 ),
 ( #6379, #20172 ),
 ( #26645, #10844 ),
 ( #24228, #11263 ) ),
 .UNSPECIFIED., .F., .F., .F. ) 
 B_SPLINE_SURFACE_WITH_KNOTS ( ( 4, 4 ),
 ( 2, 2 ),
 ( 0.000000000000000000, 1.000000000000000000 ),
 ( 0.000000000000000000, 1.000000000000000000 ),
 .UNSPECIFIED. ) 
 GEOMETRIC_REPRESENTATION_ITEM ( )  RATIONAL_B_SPLINE_SURFACE ( (
 ( 1.000000000000000000, 1.000000000000000000),
 ( 0.9956975270656954757, 0.8568959468854893125),
 ( 0.9956975270656954757, 0.8568959468854893125),
 ( 1.000000000000000000, 1.000000000000000000) ) ) 
 REPRESENTATION_ITEM ( '' )  SURFACE ( )  );
#916 = CARTESIAN_POINT ( 'NONE',  ( -1.045287976400365970, 28.14015102489882736, 36.12803364096558312 ) ) ;
#917 = ORIENTED_EDGE ( 'NONE', *, *, #13125, .T. ) ;
#918 = ORIENTED_EDGE ( 'NONE', *, *, #7791, .F. ) ;
#919 = ORIENTED_EDGE ( 'NONE', *, *, #18893, .T. ) ;
#920 = B_SPLINE_CURVE_WITH_KNOTS ( 'NONE', 3,
 ( #12975, #27954, #17427, #28364, #25950, #10834 ),
 .UNSPECIFIED., .F., .F.,
 ( 4, 2, 4 ),
 ( 1.734723475976807094E-18, 0.0004335151646191503279, 0.0008670303292382989212 ),
 .UNSPECIFIED. ) ;
#921 =( BOUNDED_SURFACE ( )  B_SPLINE_SURFACE ( 3, 1, ( 
 ( #9026, #4135 ),
 ( #2238, #1969 ),
 ( #17507, #26294 ),
 ( #15476, #2381 ) ),
 .UNSPECIFIED., .F., .F., .F. ) 
 B_SPLINE_SURFACE_WITH_KNOTS ( ( 4, 4 ),
 ( 2, 2 ),
 ( 0.000000000000000000, 1.000000000000000000 ),
 ( 0.000000000000000000, 1.000000000000000000 ),
 .UNSPECIFIED. ) 
 GEOMETRIC_REPRESENTATION_ITEM ( )  RATIONAL_B_SPLINE_SURFACE ( (
 ( 1.000000000000000000, 1.000000000000000000),
 ( 0.6386103224230302855, 0.9954351624131538845),
 ( 0.6386103224230302855, 0.9954351624131538845),
 ( 1.000000000000000000, 1.000000000000000000) ) ) 
 REPRESENTATION_ITEM ( '' )  SURFACE ( )  );
#922 = ORIENTED_EDGE ( 'NONE', *, *, #28349, .T. ) ;
#923 = CARTESIAN_POINT ( 'NONE',  ( 109.1721716018069515, 0.01488186354165284969, -0.008358834333178128198 ) ) ;
#924 = CARTESIAN_POINT ( 'NONE',  ( 1.832998868059890096, -125.4013017422236089, 73.01698022778312236 ) ) ;
#925 = CARTESIAN_POINT ( 'NONE',  ( 2.433796855181205476, 138.8296532063094162, -43.58222566461498815 ) ) ;
#926 = CARTESIAN_POINT ( 'NONE',  ( 1.833809397773861649, 29.99591688577088178, 141.9756687985003794 ) ) ;
#927 = CARTESIAN_POINT ( 'NONE',  ( 25.64670758986456889, 35.36461833156663914, -107.2298587623391768 ) ) ;
#928 = CARTESIAN_POINT ( 'NONE',  ( 109.1586900883932856, -0.005371970278523997486, 0.004701023939953838209 ) ) ;
#929 = LINE ( 'NONE', #3380, #25774 ) ;
#930 = VECTOR ( 'NONE', #12606, 1000.000000000000114 ) ;
#931 = CARTESIAN_POINT ( 'NONE',  ( 109.1587776205901577, -0.0008489206734409406778, 0.007280006032833115891 ) ) ;
#932 = CARTESIAN_POINT ( 'NONE',  ( 25.64704443564077252, 56.33997466860400749, 97.85065179540777081 ) ) ;
#933 = LINE ( 'NONE', #9724, #23078 ) ;
#934 = VECTOR ( 'NONE', #15204, 1000.000000000000114 ) ;
#935 = EDGE_CURVE ( 'NONE', #246, #26070, #25013, .T. ) ;
#936 = ORIENTED_EDGE ( 'NONE', *, *, #17252, .F. ) ;
#937 = EDGE_LOOP ( 'NONE', ( #2335, #18121, #2579, #3275 ) ) ;
#938 = CARTESIAN_POINT ( 'NONE',  ( 25.64681081121879203, 91.59071981940661544, -66.03065707438841514 ) ) ;
#939 = EDGE_CURVE ( 'NONE', #22112, #15531, #951, .T. ) ;
#941 = CARTESIAN_POINT ( 'NONE',  ( 25.64708010899961366, -91.31497827399779510, 66.41183455464110352 ) ) ;
#940 = CARTESIAN_POINT ( 'NONE',  ( 25.64704443564077252, 66.47548630737979636, -91.26857357624498945 ) ) ;
#942 = CARTESIAN_POINT ( 'NONE',  ( -20.20700224038492721, -24.51628800869035274, 16.58740185276737122 ) ) ;
#943 = DIRECTION ( 'NONE',  ( -1.000000000000000000, -0.000000000000000000, -0.000000000000000000 ) ) ;
#944 = CARTESIAN_POINT ( 'NONE',  ( -7.078251931573400491, 20.86696228105224549, -47.71415099571811425 ) ) ;
#945 = VERTEX_POINT ( 'NONE', #18510 ) ;
#946 = CARTESIAN_POINT ( 'NONE',  ( 10.93730112725972070, -51.37919228020375328, 142.1801301103782293 ) ) ;
#947 = EDGE_CURVE ( 'NONE', #1416, #19279, #2081, .T. ) ;
#948 = CARTESIAN_POINT ( 'NONE',  ( 2.063896406836605024, 144.3268707900447225, 16.52087515463826151 ) ) ;
#949 = LINE ( 'NONE', #9739, #14379 ) ;
#950 = ORIENTED_EDGE ( 'NONE', *, *, #18124, .T. ) ;
#951 = LINE ( 'NONE', #9741, #11893 ) ;
#952 = PLANE ( 'NONE',  #23667 ) ;
#953 = ADVANCED_FACE ( 'NONE', ( #1099 ), #25363, .F. ) ;
#954 = VECTOR ( 'NONE', #18803, 1000.000000000000114 ) ;
#955 = CARTESIAN_POINT ( 'NONE',  ( -1.058473599757824735, 1.755404039370064950, 45.77379534793241334 ) ) ;
#956 = B_SPLINE_CURVE_WITH_KNOTS ( 'NONE', 3,
 ( #4955, #25257, #9287, #13728 ),
 .UNSPECIFIED., .F., .F.,
 ( 4, 4 ),
 ( 0.000000000000000000, 0.008383560773332696461 ),
 .UNSPECIFIED. ) ;
#957 = VECTOR ( 'NONE', #13588, 1000.000000000000114 ) ;
#958 = B_SPLINE_CURVE_WITH_KNOTS ( 'NONE', 3,
 ( #5013, #22156, #9356, #22449, #11489, #22599 ),
 .UNSPECIFIED., .F., .F.,
 ( 4, 2, 4 ),
 ( 1.447636874611986795E-16, 0.003570751334075636125, 0.007141502668151127400 ),
 .UNSPECIFIED. ) ;
#959 = ORIENTED_EDGE ( 'NONE', *, *, #1565, .T. ) ;
#960 = CARTESIAN_POINT ( 'NONE',  ( 1.833485406944043827, -84.86072343962486286, -117.7091014914958578 ) ) ;
#961 =( BOUNDED_SURFACE ( )  B_SPLINE_SURFACE ( 3, 1, ( 
 ( #5989, #12724 ),
 ( #25708, #23410 ),
 ( #21373, #8153 ),
 ( #5708, #5847 ) ),
 .UNSPECIFIED., .F., .F., .F. ) 
 B_SPLINE_SURFACE_WITH_KNOTS ( ( 4, 4 ),
 ( 2, 2 ),
 ( 0.000000000000000000, 1.000000000000000000 ),
 ( 0.000000000000000000, 1.000000000000000000 ),
 .UNSPECIFIED. ) 
 GEOMETRIC_REPRESENTATION_ITEM ( )  RATIONAL_B_SPLINE_SURFACE ( (
 ( 1.000000000000000000, 1.000000000000000000),
 ( 0.7789835883360576307, 0.9689951854195403280),
 ( 0.7789835883360576307, 0.9689951854195403280),
 ( 1.000000000000000000, 1.000000000000000000) ) ) 
 REPRESENTATION_ITEM ( '' )  SURFACE ( )  );
#962 = ORIENTED_EDGE ( 'NONE', *, *, #8677, .F. ) ;
#963 = CARTESIAN_POINT ( 'NONE',  ( -55.24300891470650754, -0.002702093572892964434, 0.009439835024158798812 ) ) ;
#964 = ORIENTED_EDGE ( 'NONE', *, *, #17303, .T. ) ;
#965 =( NAMED_UNIT ( * ) PLANE_ANGLE_UNIT ( ) SI_UNIT ( $, .RADIAN. ) );
#966 = CARTESIAN_POINT ( 'NONE',  ( -1.031422197589711987, 37.93675465142509040, 25.67058493451400381 ) ) ;
#967 = CARTESIAN_POINT ( 'NONE',  ( -1.048172774974287069, 15.11899685083884393, 43.23017713506509097 ) ) ;
#968 = CARTESIAN_POINT ( 'NONE',  ( 1.831572820252008738, 141.7320553118906048, 31.13525033585541735 ) ) ;
#969 = CARTESIAN_POINT ( 'NONE',  ( 1.833750490713684123, -107.6587173638740467, -97.29556423840249124 ) ) ;
#970 = ORIENTED_EDGE ( 'NONE', *, *, #27106, .F. ) ;
#971 = CARTESIAN_POINT ( 'NONE',  ( 32.73300124599741423, -84.80615050150312584, -81.52272205837286378 ) ) ;
#972 = CARTESIAN_POINT ( 'NONE',  ( 109.1624594426973260, 0.009004164758061389967, 0.01318243916934106613 ) ) ;
#973 = CARTESIAN_POINT ( 'NONE',  ( 2.433796855181219243, 144.5536872373191670, 16.65276281464612396 ) ) ;
#974 = ORIENTED_EDGE ( 'NONE', *, *, #4787, .T. ) ;
#975 = VECTOR ( 'NONE', #24764, 1000.000000000000000 ) ;
#976 = VERTEX_POINT ( 'NONE', #7085 ) ;
#977 = EDGE_LOOP ( 'NONE', ( #3699, #10552, #19085, #2167 ) ) ;
#978 = PLANE ( 'NONE',  #18447 ) ;
#979 = CARTESIAN_POINT ( 'NONE',  ( 32.73300124599738581, 51.32617430725051832, -105.8473486001045387 ) ) ;
#980 = ADVANCED_FACE ( 'NONE', ( #26487 ), #2904, .F. ) ;
#982 = CARTESIAN_POINT ( 'NONE',  ( 109.1586900883932856, 0.007137750914552286330, 0.0001010081143884431274 ) ) ;
#981 = CARTESIAN_POINT ( 'NONE',  ( 19.66333377628693313, 108.7423656420560008, 84.55762186019606474 ) ) ;
#983 = CONICAL_SURFACE ( 'NONE', #7413, 34.60786435723138510, 0.8559913436420825139 ) ;
#984 = CARTESIAN_POINT ( 'NONE',  ( -20.57838717382308147, 7.715628353033680220, -28.96176188950220975 ) ) ;
#985 = CARTESIAN_POINT ( 'NONE',  ( -20.20700224038492010, -18.19058640100240254, -23.35150625415651859 ) ) ;
#986 = CARTESIAN_POINT ( 'NONE',  ( 25.64699802086726876, 45.70780507840577656, -103.2460182674612668 ) ) ;
#987 = VERTEX_POINT ( 'NONE', #728 ) ;
#988 = CARTESIAN_POINT ( 'NONE',  ( 2.263178607246642216, 145.3892423243864584, -1.401567185706980245 ) ) ;
#989 = VECTOR ( 'NONE', #21263, 1000.000000000000000 ) ;
#990 = CARTESIAN_POINT ( 'NONE',  ( -1.058473599757832062, 44.07591602137171094, 12.47539220917817815 ) ) ;
#991 = CARTESIAN_POINT ( 'NONE',  ( 25.81918753295376590, -67.18811037444370982, -90.88802830332029714 ) ) ;
#992 = EDGE_CURVE ( 'NONE', #14085, #11759, #7270, .T. ) ;
#993 = CARTESIAN_POINT ( 'NONE',  ( -20.47566338032516597, -27.87687989047309145, 10.72601609985058957 ) ) ;
#994 = DIRECTION ( 'NONE',  ( 0.000000000000000000, -0.000000000000000000, 1.000000000000000000 ) ) ;
#995 = FACE_OUTER_BOUND ( 'NONE', #19528, .T. ) ;
#996 = ORIENTED_EDGE ( 'NONE', *, *, #15714, .T. ) ;
#997 = CARTESIAN_POINT ( 'NONE',  ( 1.833485406944071361, 29.64752363041738548, -142.0485807715643034 ) ) ;
#998 = CARTESIAN_POINT ( 'NONE',  ( 26.11404676487257603, -65.63269960453179408, -92.25884714080473259 ) ) ;
#999 = CARTESIAN_POINT ( 'NONE',  ( 10.93730112725970294, 65.95960219663110990, 136.0306644680985642 ) ) ;
#1000 = ORIENTED_EDGE ( 'NONE', *, *, #7940, .T. ) ;
#1001 = VERTEX_POINT ( 'NONE', #4613 ) ;
#1002 = FACE_OUTER_BOUND ( 'NONE', #27553, .T. ) ;
#1003 = CARTESIAN_POINT ( 'NONE',  ( 2.433796855181205476, 74.00833731765735024, -125.2830755159746445 ) ) ;
#1004 = ORIENTED_EDGE ( 'NONE', *, *, #3036, .F. ) ;
#1005 = CARTESIAN_POINT ( 'NONE',  ( -1.048994561756802169, -14.87838255483227101, 43.31369460697990803 ) ) ;
#1006 = AXIS2_PLACEMENT_3D ( 'NONE', #13827, #3328, #7810 ) ;
#1007 = CARTESIAN_POINT ( 'NONE',  ( 25.64681081121879203, 83.63051021305903987, 75.86069728269016821 ) ) ;
#1008 = FACE_OUTER_BOUND ( 'NONE', #523, .T. ) ;
#1009 = ORIENTED_EDGE ( 'NONE', *, *, #12133, .F. ) ;
#1010 = CARTESIAN_POINT ( 'NONE',  ( 2.433796855181233454, 13.76554153471886366, -144.8571464219887730 ) ) ;
#1011 = CARTESIAN_POINT ( 'NONE',  ( -1.239374126674604337, 42.99367564261301311, 16.50008610789253893 ) ) ;
#1012 =( BOUNDED_SURFACE ( )  B_SPLINE_SURFACE ( 3, 1, ( 
 ( #11858, #9699 ),
 ( #10699, #19466 ),
 ( #15124, #26083 ),
 ( #19602, #27829 ) ),
 .UNSPECIFIED., .F., .F., .F. ) 
 B_SPLINE_SURFACE_WITH_KNOTS ( ( 4, 4 ),
 ( 2, 2 ),
 ( 0.000000000000000000, 1.000000000000000000 ),
 ( 0.000000000000000000, 1.000000000000000000 ),
 .UNSPECIFIED. ) 
 GEOMETRIC_REPRESENTATION_ITEM ( )  RATIONAL_B_SPLINE_SURFACE ( (
 ( 1.000000000000000000, 1.000000000000000000),
 ( 0.9960225298536222738, 0.9999952330161893110),
 ( 0.9960225298536222738, 0.9999952330161893110),
 ( 1.000000000000000000, 1.000000000000000000) ) ) 
 REPRESENTATION_ITEM ( '' )  SURFACE ( )  );
#1013 = CARTESIAN_POINT ( 'NONE',  ( -20.57838717382308147, -27.96569011373093971, -10.78122205916989529 ) ) ;
#1014 = EDGE_LOOP ( 'NONE', ( #22771, #13153, #16173, #16960 ) ) ;
#1015 = ORIENTED_EDGE ( 'NONE', *, *, #21712, .F. ) ;
#1016 = CARTESIAN_POINT ( 'NONE',  ( -55.25719721206881729, 0.0006290797159235729736, 0.01115102788683339750 ) ) ;
#1017 = CARTESIAN_POINT ( 'NONE',  ( 16.05277956358203895, -80.40847413522624265, 118.6216415718958359 ) ) ;
#1018 = EDGE_CURVE ( 'NONE', #18216, #9135, #11027, .T. ) ;
#1019 = CARTESIAN_POINT ( 'NONE',  ( 28.43349137099838941, -17.01091693849658526, -123.0821667346709489 ) ) ;
#1020 = CARTESIAN_POINT ( 'NONE',  ( 109.1721716018069515, 0.0002019688922688021263, -0.01706748904931388797 ) ) ;
#1021 = CARTESIAN_POINT ( 'NONE',  ( -1.619063947482194177, 35.99532424477422410, 29.22875152547716482 ) ) ;
#1022 = CARTESIAN_POINT ( 'NONE',  ( 25.64681081121879203, 107.5125461021402486, 34.49579773461821475 ) ) ;
#1023 = B_SPLINE_CURVE_WITH_KNOTS ( 'NONE', 3,
 ( #15716, #187, #8834, #26653 ),
 .UNSPECIFIED., .F., .F.,
 ( 4, 4 ),
 ( 1.745790404657100200E-16, 0.008383748772659646228 ),
 .UNSPECIFIED. ) ;
#1024 = CARTESIAN_POINT ( 'NONE',  ( -1.050230346682665239, -45.79907861045645490, -0.0006945978174090946524 ) ) ;
#1025 = VERTEX_POINT ( 'NONE', #22181 ) ;
#1026 = LINE ( 'NONE', #12112, #16910 ) ;
#1027 = CARTESIAN_POINT ( 'NONE',  ( 32.73300124599732186, 0.000000000000000000, 0.000000000000000000 ) ) ;
#1028 = CARTESIAN_POINT ( 'NONE',  ( 30.59138290137883942, -75.73279410806787837, 88.14703743378208856 ) ) ;
#1029 = ADVANCED_FACE ( 'NONE', ( #9517 ), #15798, .F. ) ;
#1030 = EDGE_CURVE ( 'NONE', #24050, #19015, #732, .T. ) ;
#1031 = CARTESIAN_POINT ( 'NONE',  ( -7.733045908741322805, -45.70676731105703539, 25.81515396910911875 ) ) ;
#1032 = VECTOR ( 'NONE', #13741, 1000.000000000000114 ) ;
#1033 = CARTESIAN_POINT ( 'NONE',  ( -1.259972190295298500, 38.49631882650683679, 25.19627397134255986 ) ) ;
#1034 = VERTEX_POINT ( 'NONE', #2742 ) ;
#1035 = VECTOR ( 'NONE', #20009, 1000.000000000000114 ) ;
#1036 = EDGE_LOOP ( 'NONE', ( #12535, #4918, #20028, #24513 ) ) ;
#1037 = CARTESIAN_POINT ( 'NONE',  ( 25.64692232868535626, -75.30916867847156482, 84.12764974008001673 ) ) ;
#1038 = EDGE_LOOP ( 'NONE', ( #13079, #8094, #11343, #21519 ) ) ;
#1039 = ORIENTED_EDGE ( 'NONE', *, *, #17983, .F. ) ;
#1040 = ORIENTED_EDGE ( 'NONE', *, *, #21609, .F. ) ;
#1041 = CARTESIAN_POINT ( 'NONE',  ( 10.93730112725939030, 136.0306644680981947, 65.95960219663135149 ) ) ;
#1042 = PRODUCT_DEFINITION_CONTEXT ( 'detailed design', #27763, 'design' ) ;
#1043 = CARTESIAN_POINT ( 'NONE',  ( -2.265401668238139266, -17.02144111536849636, 43.82493763960401623 ) ) ;
#1044 = CARTESIAN_POINT ( 'NONE',  ( 109.1586900883932856, 0.004277182003227222341, 0.005715190711481739176 ) ) ;
#1045 = CONICAL_SURFACE ( 'NONE', #16695, 53.53553390275978785, 0.7853981625000051592 ) ;
#1046 = EDGE_CURVE ( 'NONE', #8158, #19215, #440, .T. ) ;
#1047 = AXIS2_PLACEMENT_3D ( 'NONE', #4963, #16042, #359 ) ;
#1048 = CARTESIAN_POINT ( 'NONE',  ( -8.786685647604894456, 37.00619870957989832, 38.68584556812258768 ) ) ;
#1049 = CARTESIAN_POINT ( 'NONE',  ( 1.833809397773829453, 132.4918864201828228, 59.18399778167182745 ) ) ;
#1050 = EDGE_CURVE ( 'NONE', #17941, #7710, #9660, .T. ) ;
#1051 = EDGE_CURVE ( 'NONE', #9366, #14748, #20844, .T. ) ;
#1052 = CARTESIAN_POINT ( 'NONE',  ( 5.340103556456507583, -108.0219267027623715, -100.3626145793573698 ) ) ;
#1053 = CARTESIAN_POINT ( 'NONE',  ( 1.833603222531957400, -84.93295186324782264, -117.6571262511687195 ) ) ;
#1054 = CARTESIAN_POINT ( 'NONE',  ( 1.832998868059890096, 73.01698022778529662, -125.4013017422223299 ) ) ;
#1055 = CARTESIAN_POINT ( 'NONE',  ( 26.11404676487256893, -55.62948129436175293, -98.61392875273419634 ) ) ;
#1056 = CARTESIAN_POINT ( 'NONE',  ( -20.20700224038492721, -23.35150625415671755, -18.19058640100215385 ) ) ;
#1057 = CARTESIAN_POINT ( 'NONE',  ( 26.11404676487259024, -22.43340081644844020, 110.9778746459746372 ) ) ;
#1058 = CARTESIAN_POINT ( 'NONE',  ( 16.75465622695657331, 34.09043808962603350, -138.0797984721902196 ) ) ;
#1059 = CARTESIAN_POINT ( 'NONE',  ( -20.47566262905010248, 29.82700878811083811, 1.586617686065662447 ) ) ;
#1060 = CARTESIAN_POINT ( 'NONE',  ( 2.263178607246672414, -107.1074316126224488, 98.32595927618818621 ) ) ;
#1061 = VERTEX_POINT ( 'NONE', #27791 ) ;
#1062 = DIRECTION ( 'NONE',  ( 0.000000000000000000, 0.000000000000000000, 1.000000000000000000 ) ) ;
#1063 = ORIENTED_EDGE ( 'NONE', *, *, #13566, .F. ) ;
#1064 = CARTESIAN_POINT ( 'NONE',  ( -1.048171036023507252, 43.86077206077069235, -13.17819047681618372 ) ) ;
#1065 = CARTESIAN_POINT ( 'NONE',  ( 6.224689322667630975, -62.55544044765341027, 134.1951906609236858 ) ) ;
#1066 = EDGE_LOOP ( 'NONE', ( #5349, #11502, #21928, #16662 ) ) ;
#1067 = AXIS2_PLACEMENT_3D ( 'NONE', #14772, #4114, #28146 ) ;
#1068 = VERTEX_POINT ( 'NONE', #21157 ) ;
#1069 = VECTOR ( 'NONE', #13291, 1000.000000000000114 ) ;
#1070 = EDGE_LOOP ( 'NONE', ( #17805, #6885, #23534, #12703 ) ) ;
#1071 = B_SPLINE_CURVE_WITH_KNOTS ( 'NONE', 3,
 ( #3634, #14439, #4446, #1336, #23673, #24187, #13221 ),
 .UNSPECIFIED., .F., .F.,
 ( 4, 3, 4 ),
 ( 3.404394821604483923E-17, 0.0002669559177086211531, 0.0005339083821118883934 ),
 .UNSPECIFIED. ) ;
#1072 = ORIENTED_EDGE ( 'NONE', *, *, #22607, .T. ) ;
#1073 = CARTESIAN_POINT ( 'NONE',  ( 2.430230287190592531, 16.65331920325739645, 144.5585181921886715 ) ) ;
#1074 = CARTESIAN_POINT ( 'NONE',  ( 109.1586059443104944, 0.005881369279875405844, -0.003930911098393235874 ) ) ;
#1075 = CARTESIAN_POINT ( 'NONE',  ( 2.063896406836605024, -84.29612368209072315, -118.3103904147690173 ) ) ;
#1076 = EDGE_CURVE ( 'NONE', #813, #11790, #25508, .T. ) ;
#1077 = CARTESIAN_POINT ( 'NONE',  ( -1.031422197589716205, -28.14735071801717936, 36.13727897780158571 ) ) ;
#1078 = EDGE_CURVE ( 'NONE', #17856, #14908, #16032, .T. ) ;
#1079 = CARTESIAN_POINT ( 'NONE',  ( -1.056502255334265339, 26.51074901220557933, 37.35734037467605617 ) ) ;
#1080 = CARTESIAN_POINT ( 'NONE',  ( 119.2224693531408803, 90.00000000000005684, -19.99999999999998934 ) ) ;
#1081 = CARTESIAN_POINT ( 'NONE',  ( -1.323439229708136100, 25.17120723334093313, -38.58845475799776636 ) ) ;
#1083 = CARTESIAN_POINT ( 'NONE',  ( -1.048994561756786625, -13.42228657661154401, -43.78680886990936472 ) ) ;
#1082 = CARTESIAN_POINT ( 'NONE',  ( -20.20612092514784663, 10.22177639105900226, 27.77903665678154255 ) ) ;
#1084 = CARTESIAN_POINT ( 'NONE',  ( -21.41430102051744910, -7.777552968935554034, 29.81033373822135246 ) ) ;
#1085 = VECTOR ( 'NONE', #3210, 999.9999999999998863 ) ;
#1086 = VERTEX_POINT ( 'NONE', #14540 ) ;
#1087 = VERTEX_POINT ( 'NONE', #18421 ) ;
#1088 = CARTESIAN_POINT ( 'NONE',  ( -1.046936909428682005, -25.87632113675133283, 37.78538189376536849 ) ) ;
#1090 = CARTESIAN_POINT ( 'NONE',  ( 32.73300124599737160, -108.9684813982492244, 44.31599526637918274 ) ) ;
#1089 = CARTESIAN_POINT ( 'NONE',  ( -23.79223135445720061, 13.25822371132295352, -30.42557260166815780 ) ) ;
#1091 = CARTESIAN_POINT ( 'NONE',  ( 8.186469777910742707, -27.65107827750183134, 146.7694294853781685 ) ) ;
#1092 = SURFACE_SIDE_STYLE ('',( #20514 ) ) ;
#1093 = CARTESIAN_POINT ( 'NONE',  ( 2.433796855181233454, 144.8571464219889151, 13.76554153471742481 ) ) ;
#1094 = VERTEX_POINT ( 'NONE', #5478 ) ;
#1095 = CARTESIAN_POINT ( 'NONE',  ( 1.833838850855463720, 44.75675607098931152, 138.0350826608189720 ) ) ;
#1096 = CARTESIAN_POINT ( 'NONE',  ( -9.156249394959706578, -53.90509764945135629, -8.027840202793747437 ) ) ;
#1097 = CARTESIAN_POINT ( 'NONE',  ( -1.019300379054419947, 28.53917295602898463, -35.83762006677410028 ) ) ;
#1098 = ORIENTED_EDGE ( 'NONE', *, *, #9233, .F. ) ;
#1099 = FACE_OUTER_BOUND ( 'NONE', #1014, .T. ) ;
#1100 = CARTESIAN_POINT ( 'NONE',  ( -28.13707043255157103, 21.52861750560949972, 7.802116958608778852 ) ) ;
#1101 = ADVANCED_FACE ( 'NONE', ( #16274 ), #27971, .T. ) ;
#1102 =( BOUNDED_SURFACE ( )  B_SPLINE_SURFACE ( 3, 1, ( 
 ( #17013, #15264 ),
 ( #24360, #15545 ),
 ( #20022, #26212 ),
 ( #13250, #6515 ) ),
 .UNSPECIFIED., .F., .F., .F. ) 
 B_SPLINE_SURFACE_WITH_KNOTS ( ( 4, 4 ),
 ( 2, 2 ),
 ( 0.000000000000000000, 1.000000000000000000 ),
 ( 0.000000000000000000, 1.000000000000000000 ),
 .UNSPECIFIED. ) 
 GEOMETRIC_REPRESENTATION_ITEM ( )  RATIONAL_B_SPLINE_SURFACE ( (
 ( 1.000000000000000000, 1.000000000000000000),
 ( 0.9934239774497838349, 0.8357310067453913582),
 ( 0.9934239774497838349, 0.8357310067453913582),
 ( 1.000000000000000000, 1.000000000000000000) ) ) 
 REPRESENTATION_ITEM ( '' )  SURFACE ( )  );
#1103 = VECTOR ( 'NONE', #24555, 1000.000000000000114 ) ;
#1104 = CARTESIAN_POINT ( 'NONE',  ( 32.73300124599732186, 0.000000000000000000, 0.000000000000000000 ) ) ;
#1105 = EDGE_CURVE ( 'NONE', #14457, #15269, #6847, .T. ) ;
#1106 = ORIENTED_EDGE ( 'NONE', *, *, #3667, .F. ) ;
#1107 = CARTESIAN_POINT ( 'NONE',  ( 1.834118845439484335, -144.3336252355298370, 14.99112450600202173 ) ) ;
#1108 = CARTESIAN_POINT ( 'NONE',  ( 26.04756280548353331, 112.6689254848259196, 10.72497307632831642 ) ) ;
#1109 = EDGE_CURVE ( 'NONE', #16636, #9768, #14101, .T. ) ;
#1110 = ORIENTED_EDGE ( 'NONE', *, *, #4327, .T. ) ;
#1111 = CARTESIAN_POINT ( 'NONE',  ( 881.1325374217867648, 943.0690745387362313, 1502.633622565728274 ) ) ;
#1112 = CARTESIAN_POINT ( 'NONE',  ( 109.1589550718174877, -0.005777059646704624067, 0.004900004919104979095 ) ) ;
#1113 = EDGE_CURVE ( 'NONE', #13345, #26365, #18077, .T. ) ;
#1114 = DIRECTION ( 'NONE',  ( 0.7563875759206387661, -0.6320336713238486892, 0.1685564395263406956 ) ) ;
#1115 = DIRECTION ( 'NONE',  ( -0.7637818620346801257, 0.3965875333584876761, 0.5092696688508626668 ) ) ;
#1116 = VERTEX_POINT ( 'NONE', #12375 ) ;
#1117 = ADVANCED_FACE ( 'NONE', ( #27198 ), #5848, .F. ) ;
#1118 = CARTESIAN_POINT ( 'NONE',  ( -1.050230346682671678, -14.15335421912552860, 43.55729751025877761 ) ) ;
#1120 = CARTESIAN_POINT ( 'NONE',  ( 109.1592201516379674, 0.007620268632968142664, 0.001934867487012853927 ) ) ;
#1119 = CARTESIAN_POINT ( 'NONE',  ( 16.05277956358206737, -142.9335921074871010, -10.32496049470232435 ) ) ;
#1121 = ORIENTED_EDGE ( 'NONE', *, *, #144, .F. ) ;
#1122 = ORIENTED_EDGE ( 'NONE', *, *, #14095, .T. ) ;
#1123 = ORIENTED_EDGE ( 'NONE', *, *, #14062, .T. ) ;
#1124 = CARTESIAN_POINT ( 'NONE',  ( 55.79472521941426777, 63.36760613016273425, -35.74479459808780746 ) ) ;
#1125 = CARTESIAN_POINT ( 'NONE',  ( -55.24390624410018802, 0.009374879212971231821, -0.004572280736701976080 ) ) ;
#1127 = CARTESIAN_POINT ( 'NONE',  ( 28.37644542392838432, -115.1790646972553276, 46.84227702240740143 ) ) ;
#1126 = CARTESIAN_POINT ( 'NONE',  ( 2.063896406836609909, 16.52087515463778544, 144.3268707900447794 ) ) ;
#1128 = CARTESIAN_POINT ( 'NONE',  ( -55.24271866751342941, 0.006671293903668397071, 0.006757859501010046559 ) ) ;
#1129 = CARTESIAN_POINT ( 'NONE',  ( -1.058197053496160667, -12.47644286888545828, -44.07533330186785037 ) ) ;
#1130 = VERTEX_POINT ( 'NONE', #10097 ) ;
#1131 = CARTESIAN_POINT ( 'NONE',  ( 1.833485406944043827, 107.4794113447409529, 97.49333871408727248 ) ) ;
#1132 = FACE_OUTER_BOUND ( 'NONE', #8743, .T. ) ;
#1133 = EDGE_LOOP ( 'NONE', ( #14391, #13621, #6892, #12399 ) ) ;
#1134 = CARTESIAN_POINT ( 'NONE',  ( -4.780792508754322157, 42.16805077400959334, -25.98388465890095489 ) ) ;
#1135 = CARTESIAN_POINT ( 'NONE',  ( -20.47566338032530098, -23.19796701701852015, 18.81547714195498244 ) ) ;
#1136 = CARTESIAN_POINT ( 'NONE',  ( -20.47566338032515532, 28.85746366088581283, 7.708089572830123082 ) ) ;
#1137 = CARTESIAN_POINT ( 'NONE',  ( 1.834118845439484335, 85.14950727126013419, -117.5010238212690155 ) ) ;
#1138 = CARTESIAN_POINT ( 'NONE',  ( -1.583189561560252701, -44.83405390829663872, 11.94859433442948493 ) ) ;
#1139 = CARTESIAN_POINT ( 'NONE',  ( 2.108393763691209788, -108.8265195087755188, 96.26428731761947688 ) ) ;
#1140 = CARTESIAN_POINT ( 'NONE',  ( -55.25719721206881729, 0.009391134844729439810, -0.006045473558784624467 ) ) ;
#1141 = ORIENTED_EDGE ( 'NONE', *, *, #1465, .F. ) ;
#1142 = FACE_OUTER_BOUND ( 'NONE', #17437, .T. ) ;
#1143 =( BOUNDED_SURFACE ( )  B_SPLINE_SURFACE ( 3, 1, ( 
 ( #11515, #18262 ),
 ( #13957, #1011 ),
 ( #3315, #18573 ),
 ( #16412, #23053 ) ),
 .UNSPECIFIED., .F., .F., .F. ) 
 B_SPLINE_SURFACE_WITH_KNOTS ( ( 4, 4 ),
 ( 2, 2 ),
 ( 0.000000000000000000, 1.000000000000000000 ),
 ( 0.000000000000000000, 1.000000000000000000 ),
 .UNSPECIFIED. ) 
 GEOMETRIC_REPRESENTATION_ITEM ( )  RATIONAL_B_SPLINE_SURFACE ( (
 ( 1.000000000000000000, 1.000000000000000000),
 ( 0.9934239774497837239, 0.8357310067453919133),
 ( 0.9934239774497837239, 0.8357310067453919133),
 ( 1.000000000000000000, 1.000000000000000000) ) ) 
 REPRESENTATION_ITEM ( '' )  SURFACE ( )  );
#1144 = DIRECTION ( 'NONE',  ( 0.000000000000000000, 0.000000000000000000, -1.000000000000000000 ) ) ;
#1145 = B_SPLINE_CURVE_WITH_KNOTS ( 'NONE', 3,
 ( #2477, #20038, #320, #17868, #16151, #24956 ),
 .UNSPECIFIED., .F., .F.,
 ( 4, 2, 4 ),
 ( 8.684452633802430946E-18, 0.0006311571484586112101, 0.001262314296917213747 ),
 .UNSPECIFIED. ) ;
#1146 = CARTESIAN_POINT ( 'NONE',  ( -55.24390624410018802, -0.004572280736701530256, -0.009374879212970928244 ) ) ;
#1147 = B_SPLINE_CURVE_WITH_KNOTS ( 'NONE', 3,
 ( #28328, #10655, #16980, #17256, #28191, #14819, #8493, #1996, #25772, #8360 ),
 .UNSPECIFIED., .F., .F.,
 ( 4, 2, 2, 2, 4 ),
 ( 1.301042606982605128E-18, 0.0003346267210630945186, 0.0006692534421261877361, 0.001003880163189281062, 0.001338506884252374171 ),
 .UNSPECIFIED. ) ;
#1148 = ORIENTED_EDGE ( 'NONE', *, *, #27023, .T. ) ;
#1149 = ORIENTED_EDGE ( 'NONE', *, *, #16963, .T. ) ;
#1150 = ADVANCED_FACE ( 'NONE', ( #10249 ), #8779, .F. ) ;
#1151 = DIRECTION ( 'NONE',  ( -1.000000000000000000, -0.000000000000000000, -0.000000000000000000 ) ) ;
#1152 = CARTESIAN_POINT ( 'NONE',  ( 109.1778270068192853, -0.009031542838317238586, -0.002278716897421720778 ) ) ;
#1153 = ORIENTED_EDGE ( 'NONE', *, *, #11866, .T. ) ;
#1154 = CARTESIAN_POINT ( 'NONE',  ( -22.23226125620943705, -11.82389163795231468, -29.33577758406444858 ) ) ;
#1155 = EDGE_CURVE ( 'NONE', #22965, #4951, #14176, .T. ) ;
#1156 = CARTESIAN_POINT ( 'NONE',  ( 9.884929003653626367, -150.4771565009630763, 4.203795436551833298 ) ) ;
#1157 = CARTESIAN_POINT ( 'NONE',  ( -8.786685647604890903, 52.67761315067286176, -9.545808661480789326 ) ) ;
#1158 = CARTESIAN_POINT ( 'NONE',  ( 1.833485406944043827, -144.3694338680886062, 14.63699153649312201 ) ) ;
#1159 = CARTESIAN_POINT ( 'NONE',  ( 55.49584447822657296, -72.12568090333348891, 7.849835876628097786 ) ) ;
#1160 = CARTESIAN_POINT ( 'NONE',  ( 28.37603512858355614, 22.09615328858603789, -112.5845402829046833 ) ) ;
#1161 = VERTEX_POINT ( 'NONE', #8626 ) ;
#1162 = ORIENTED_EDGE ( 'NONE', *, *, #14150, .T. ) ;
#1163 = ORIENTED_EDGE ( 'NONE', *, *, #13205, .T. ) ;
#1164 = B_SPLINE_CURVE_WITH_KNOTS ( 'NONE', 3,
 ( #19899, #17735, #36, #20034, #8829, #17865, #4639, #17590, #26371, #26512 ),
 .UNSPECIFIED., .F., .F.,
 ( 4, 2, 2, 2, 4 ),
 ( 2.825996620262520077E-16, 0.0003346187017559037265, 0.0006692374035115249099, 0.001003856105267145931, 0.001338474807022767060 ),
 .UNSPECIFIED. ) ;
#1165 = CARTESIAN_POINT ( 'NONE',  ( 6.224689322667630975, -111.7293398381271459, 97.14981701196286679 ) ) ;
#1166 = CARTESIAN_POINT ( 'NONE',  ( 2.430230287190572103, 132.3371620660950896, 60.50928654924799588 ) ) ;
#1167 = CARTESIAN_POINT ( 'NONE',  ( -1.049817751779873021, 13.66628317065048392, 43.71287583013712208 ) ) ;
#1168 = CARTESIAN_POINT ( 'NONE',  ( -2.265401668238144151, 36.42007794497294526, 29.73100299756526965 ) ) ;
#1169 = DIRECTION ( 'NONE',  ( 0.000000000000000000, 3.122502256758243698E-15, -1.000000000000000000 ) ) ;
#1170 = ORIENTED_EDGE ( 'NONE', *, *, #15237, .F. ) ;
#1171 = CARTESIAN_POINT ( 'NONE',  ( -1.583189561560256253, 43.29471907393742924, -16.68617981233717273 ) ) ;
#1172 = DIRECTION ( 'NONE',  ( 1.000000000000000000, -6.938893903907226837E-18, 1.734723475976806709E-18 ) ) ;
#1173 = CARTESIAN_POINT ( 'NONE',  ( -28.41354790283022069, 22.41474081378001060, -5.969609727608100158 ) ) ;
#1174 = CARTESIAN_POINT ( 'NONE',  ( 109.1592201516379674, 0.006536841731953405704, -0.004368284148529032879 ) ) ;
#1175 = ORIENTED_EDGE ( 'NONE', *, *, #22436, .F. ) ;
#1176 = VERTEX_POINT ( 'NONE', #21727 ) ;
#1177 = CARTESIAN_POINT ( 'NONE',  ( 1.834118845439484335, -132.6369225636070155, -58.85894970555047934 ) ) ;
#1178 = B_SPLINE_CURVE_WITH_KNOTS ( 'NONE', 3,
 ( #4774, #26495, #24660, #13542, #6801, #20160, #9236 ),
 .UNSPECIFIED., .F., .F.,
 ( 4, 3, 4 ),
 ( 0.000000000000000000, 0.006568092053401771921, 0.02506242213020852885 ),
 .UNSPECIFIED. ) ;
#1179 = CARTESIAN_POINT ( 'NONE',  ( 32.73300124599735739, 28.19767303745605602, 114.2056417606549132 ) ) ;
#1180 = VERTEX_POINT ( 'NONE', #6066 ) ;
#1181 = EDGE_LOOP ( 'NONE', ( #27339, #25625, #20061, #18942 ) ) ;
#1182 = ORIENTED_EDGE ( 'NONE', *, *, #12882, .F. ) ;
#1183 = EDGE_CURVE ( 'NONE', #15497, #4557, #4435, .T. ) ;
#1184 =( BOUNDED_SURFACE ( )  B_SPLINE_SURFACE ( 3, 1, ( 
 ( #8102, #25655 ),
 ( #16871, #14689 ),
 ( #20131, #11358 ),
 ( #13516, #277 ) ),
 .UNSPECIFIED., .F., .F., .F. ) 
 B_SPLINE_SURFACE_WITH_KNOTS ( ( 4, 4 ),
 ( 2, 2 ),
 ( 0.000000000000000000, 1.000000000000000000 ),
 ( 0.000000000000000000, 1.000000000000000000 ),
 .UNSPECIFIED. ) 
 GEOMETRIC_REPRESENTATION_ITEM ( )  RATIONAL_B_SPLINE_SURFACE ( (
 ( 1.000000000000000000, 1.000000000000000000),
 ( 0.9960225298536222738, 0.9999952330161893110),
 ( 0.9960225298536222738, 0.9999952330161893110),
 ( 1.000000000000000000, 1.000000000000000000) ) ) 
 REPRESENTATION_ITEM ( '' )  SURFACE ( )  );
#1185 = DIRECTION ( 'NONE',  ( 0.000000000000000000, 5.223019709707975211E-21, -1.000000000000000000 ) ) ;
#1186 = DIRECTION ( 'NONE',  ( 0.000000000000000000, 0.000000000000000000, 1.000000000000000000 ) ) ;
#1187 = ADVANCED_FACE ( 'NONE', ( #8215 ), #23353, .F. ) ;
#1188 = CARTESIAN_POINT ( 'NONE',  ( -1.619063947482197729, -2.489035965909835557, 46.30105812165550816 ) ) ;
#1189 = EDGE_CURVE ( 'NONE', #25057, #6702, #19268, .T. ) ;
#1190 = CARTESIAN_POINT ( 'NONE',  ( -2.904412668506668016, 25.64203923793632356, 40.16685646686180178 ) ) ;
#1191 = CARTESIAN_POINT ( 'NONE',  ( 28.43349137099849955, 123.9292945876796352, 8.951033805645105090 ) ) ;
#1192 = CARTESIAN_POINT ( 'NONE',  ( 25.86096068574580897, 107.8247115223745993, -33.98552076022083668 ) ) ;
#1193 = CARTESIAN_POINT ( 'NONE',  ( 25.64692232868534560, 84.12764974008027252, 75.30916867847129481 ) ) ;
#1194 = CARTESIAN_POINT ( 'NONE',  ( -25.21435515916042647, 25.00736669481023355, -23.92354251275945742 ) ) ;
#1195 = CARTESIAN_POINT ( 'NONE',  ( 32.73300124599735739, -99.90245962373877830, 62.10906484417201767 ) ) ;
#1196 = CARTESIAN_POINT ( 'NONE',  ( 1.834118845439484335, 72.40084790867506115, -125.7578880615037491 ) ) ;
#1197 = CARTESIAN_POINT ( 'NONE',  ( -20.57838717382308147, -1.611677988432151709, 29.92853265176832878 ) ) ;
#1198 = CARTESIAN_POINT ( 'NONE',  ( 32.73300124599735739, -20.69176323058707823, 115.8010721414082980 ) ) ;
#1199 = CARTESIAN_POINT ( 'NONE',  ( 25.69398547355841700, -22.75551036952002804, 110.6264597420659612 ) ) ;
#1200 = CARTESIAN_POINT ( 'NONE',  ( -1.056502255334264895, -45.80535052436396626, 0.5104472526224692608 ) ) ;
#1201 = CARTESIAN_POINT ( 'NONE',  ( -1.539760825549689294, 16.63252404870416257, 43.19716078875421772 ) ) ;
#1202 = ORIENTED_EDGE ( 'NONE', *, *, #26611, .F. ) ;
#1203 = DIRECTION ( 'NONE',  ( 0.000000000000000000, 1.000000000000000000, 0.000000000000000000 ) ) ;
#1204 = ORIENTED_EDGE ( 'NONE', *, *, #10395, .T. ) ;
#1205 = CARTESIAN_POINT ( 'NONE',  ( -25.21435515916025594, 1.749597353048488237E-16, -4.373993382621220594E-17 ) ) ;
#1206 = DIRECTION ( 'NONE',  ( 0.000000000000000000, 0.000000000000000000, 1.000000000000000000 ) ) ;
#1207 = ORIENTED_EDGE ( 'NONE', *, *, #1389, .F. ) ;
#1208 = EDGE_CURVE ( 'NONE', #25606, #12851, #25348, .T. ) ;
#1209 = ORIENTED_EDGE ( 'NONE', *, *, #11374, .T. ) ;
#1210 = EDGE_LOOP ( 'NONE', ( #20866, #21982 ) ) ;
#1211 = ADVANCED_FACE ( 'NONE', ( #23632 ), #12805, .F. ) ;
#1212 = CARTESIAN_POINT ( 'NONE',  ( -1.031422197589711987, 15.60268798220698727, 43.06660437151290211 ) ) ;
#1213 = CARTESIAN_POINT ( 'NONE',  ( 109.1589550718175161, -0.002553077953680983961, -0.007132058561966975706 ) ) ;
#1214 = CARTESIAN_POINT ( 'NONE',  ( 26.04756280548352976, 107.9769918539640514, 33.91579348271552874 ) ) ;
#1215 = CARTESIAN_POINT ( 'NONE',  ( -1.031422197589716205, 28.14735071801795740, 36.13727897780097464 ) ) ;
#1216 = B_SPLINE_CURVE_WITH_KNOTS ( 'NONE', 3,
 ( #5483, #592, #20735, #27055 ),
 .UNSPECIFIED., .F., .F.,
 ( 4, 4 ),
 ( 3.314910864404112914E-16, 0.01077107486149839373 ),
 .UNSPECIFIED. ) ;
#1217 = CARTESIAN_POINT ( 'NONE',  ( 1.832998868059890096, 125.4013017422241063, -73.01698022778224129 ) ) ;
#1218 = CARTESIAN_POINT ( 'NONE',  ( -1.045287976400383290, -12.68782741917353185, -44.00138577190637079 ) ) ;
#1219 = CARTESIAN_POINT ( 'NONE',  ( -4.162674018437132695, -45.34593312138897403, -18.33413805792422124 ) ) ;
#1220 = ORIENTED_EDGE ( 'NONE', *, *, #1493, .F. ) ;
#1221 = ORIENTED_EDGE ( 'NONE', *, *, #16545, .T. ) ;
#1222 = CARTESIAN_POINT ( 'NONE',  ( 32.73300124599732186, 0.000000000000000000, 0.000000000000000000 ) ) ;
#1224 = DIRECTION ( 'NONE',  ( -0.7637818620346800147, 0.3617919495470713898, -0.5345501402766312804 ) ) ;
#1223 = CARTESIAN_POINT ( 'NONE',  ( 25.64703792032471696, 66.24710921678179432, -91.43447020678362946 ) ) ;
#1225 = CARTESIAN_POINT ( 'NONE',  ( 1.833838848569455893, -85.14939661881641086, 117.5008734796307976 ) ) ;
#1226 = CARTESIAN_POINT ( 'NONE',  ( 25.98552792386799837, 10.75254026142952135, -112.6247604222997438 ) ) ;
#1227 = CARTESIAN_POINT ( 'NONE',  ( -55.25719721206881729, 0.01079965405819524257, -0.002847566758684156023 ) ) ;
#1228 = ORIENTED_EDGE ( 'NONE', *, *, #25694, .F. ) ;
#1229 = CARTESIAN_POINT ( 'NONE',  ( -2.904412668506659578, -25.64203923793602868, -40.16685646686200073 ) ) ;
#1230 = CARTESIAN_POINT ( 'NONE',  ( -1.113548883309550375, 35.91246368318242332, 28.52482525634906096 ) ) ;
#1231 = CARTESIAN_POINT ( 'NONE',  ( -1.031422197589716205, 28.14735071801795740, 36.13727897780097464 ) ) ;
#1232 = ORIENTED_EDGE ( 'NONE', *, *, #28135, .F. ) ;
#1233 = FACE_OUTER_BOUND ( 'NONE', #15110, .T. ) ;
#1234 = CARTESIAN_POINT ( 'NONE',  ( -1.259972190295306715, -38.49631882650665204, -25.19627397134285474 ) ) ;
#1235 = EDGE_CURVE ( 'NONE', #5518, #15303, #12658, .T. ) ;
#1236 = ORIENTED_EDGE ( 'NONE', *, *, #3674, .T. ) ;
#1237 = EDGE_CURVE ( 'NONE', #8709, #10429, #1618, .T. ) ;
#1238 = ADVANCED_FACE ( 'NONE', ( #12793 ), #12841, .F. ) ;
#1239 = FACE_OUTER_BOUND ( 'NONE', #28366, .T. ) ;
#1240 = ORIENTED_EDGE ( 'NONE', *, *, #14373, .F. ) ;
#1241 = CARTESIAN_POINT ( 'NONE',  ( 25.64681081121879203, -45.54494737132156246, -103.3177883989783936 ) ) ;
#1242 = CARTESIAN_POINT ( 'NONE',  ( 10.93730112725972781, -71.28103789255033007, 133.3192575531796251 ) ) ;
#1243 = DIRECTION ( 'NONE',  ( -0.9415939028147867207, -0.3336691991819678016, -0.04545093727617131873 ) ) ;
#1244 = CARTESIAN_POINT ( 'NONE',  ( -1.583189561560252701, 11.94859433442964658, 44.83405390829658188 ) ) ;
#1245 = LINE ( 'NONE', #10043, #19404 ) ;
#1246 = CARTESIAN_POINT ( 'NONE',  ( -21.41430102051751305, 19.54553566814620069, 23.81424706376344247 ) ) ;
#1247 = EDGE_LOOP ( 'NONE', ( #20214, #9048, #11519, #1121 ) ) ;
#1249 = CARTESIAN_POINT ( 'NONE',  ( 109.1721716018069515, 0.003350975118860970506, 0.01673651515802105152 ) ) ;
#1248 = CARTESIAN_POINT ( 'NONE',  ( 1.833809397773856986, 85.43729755723308017, -117.2915757704548838 ) ) ;
#1250 = CARTESIAN_POINT ( 'NONE',  ( -25.21435515916025594, 1.749597353048488237E-16, -4.373993382621220594E-17 ) ) ;
#1251 = ORIENTED_EDGE ( 'NONE', *, *, #18700, .T. ) ;
#1252 = ORIENTED_EDGE ( 'NONE', *, *, #4451, .F. ) ;
#1253 = ORIENTED_EDGE ( 'NONE', *, *, #21125, .T. ) ;
#1254 = CARTESIAN_POINT ( 'NONE',  ( -20.20700224038492365, 8.199606986804329978, -28.44216453106539078 ) ) ;
#1255 = CARTESIAN_POINT ( 'NONE',  ( -24.53237795827028478, -30.86653739599989521, 14.09663893005617119 ) ) ;
#1257 = CARTESIAN_POINT ( 'NONE',  ( 10.93730112725978287, -140.0398180619114896, 56.95489579269701608 ) ) ;
#1256 = CARTESIAN_POINT ( 'NONE',  ( 1.833838850093452821, 107.8375672471895399, -97.09738632348927467 ) ) ;
#1258 = B_SPLINE_CURVE_WITH_KNOTS ( 'NONE', 3,
 ( #14134, #20912, #5818, #7697 ),
 .UNSPECIFIED., .F., .F.,
 ( 4, 4 ),
 ( 7.152448122690996019E-18, 0.008383560773332713809 ),
 .UNSPECIFIED. ) ;
#1259 = CARTESIAN_POINT ( 'NONE',  ( -20.47566338032527966, 27.87687989047307013, -10.72601609985035331 ) ) ;
#1260 = CARTESIAN_POINT ( 'NONE',  ( 1.833485406944057594, -132.7804117027884274, -58.53321471327013370 ) ) ;
#1261 = ORIENTED_EDGE ( 'NONE', *, *, #12602, .F. ) ;
#1262 = CARTESIAN_POINT ( 'NONE',  ( -55.24198130335446422, 0.006617369590169233477, 0.006527480770975859110 ) ) ;
#1263 = CARTESIAN_POINT ( 'NONE',  ( 25.64692872815577118, 46.21877827526699889, -103.0182448446669241 ) ) ;
#1264 = ORIENTED_EDGE ( 'NONE', *, *, #22425, .F. ) ;
#1265 = CARTESIAN_POINT ( 'NONE',  ( -20.20612091757422846, -29.57813639663779526, -1.137293889216260512 ) ) ;
#1266 = LINE ( 'NONE', #12347, #27185 ) ;
#1267 = CARTESIAN_POINT ( 'NONE',  ( -20.20700224038492721, 28.44216453106548315, 8.199606986804035103 ) ) ;
#1268 = EDGE_CURVE ( 'NONE', #14951, #7509, #6412, .T. ) ;
#1269 = CARTESIAN_POINT ( 'NONE',  ( 8.186469829614267724, -137.8131829164339024, 57.56191610809328552 ) ) ;
#1270 = CARTESIAN_POINT ( 'NONE',  ( 2.430230287190581429, -71.49654683843421310, -126.7388733285352345 ) ) ;
#1271 = CARTESIAN_POINT ( 'NONE',  ( -2.265401668238157473, 39.53028715828234851, -25.45016726748328040 ) ) ;
#1272 = CARTESIAN_POINT ( 'NONE',  ( 109.1778270068192853, -0.008236503545664842357, 0.004349865064712375717 ) ) ;
#1273 = ORIENTED_EDGE ( 'NONE', *, *, #7597, .T. ) ;
#1274 = CARTESIAN_POINT ( 'NONE',  ( -8.786685647604894456, -23.24040270374358030, 48.22796981442792230 ) ) ;
#1276 = EDGE_CURVE ( 'NONE', #8760, #14056, #5386, .T. ) ;
#1275 = CARTESIAN_POINT ( 'NONE',  ( -20.20700224038492721, -16.58740185276692358, 24.51628800869065827 ) ) ;
#1277 = CARTESIAN_POINT ( 'NONE',  ( -1.323830074806763957, 12.01461446423264690, 44.47857376182257383 ) ) ;
#1278 = EDGE_CURVE ( 'NONE', #2646, #3538, #13274, .T. ) ;
#1279 = ORIENTED_EDGE ( 'NONE', *, *, #11247, .F. ) ;
#1280 = CARTESIAN_POINT ( 'NONE',  ( -1.058197053496165552, -1.754224732379234153, 45.77356582045592859 ) ) ;
#1281 = DIRECTION ( 'NONE',  ( 1.000000000000000000, -6.938893903907226837E-18, 1.734723475976806709E-18 ) ) ;
#1282 = B_SPLINE_CURVE_WITH_KNOTS ( 'NONE', 3,
 ( #16754, #23098, #27675, #11850 ),
 .UNSPECIFIED., .F., .F.,
 ( 4, 4 ),
 ( 0.000000000000000000, 0.01077107196513874335 ),
 .UNSPECIFIED. ) ;
#1283 = CARTESIAN_POINT ( 'NONE',  ( -1.045287976400362417, -44.00138577190658395, -12.68782741917276446 ) ) ;
#1284 =( NAMED_UNIT ( * ) PLANE_ANGLE_UNIT ( ) SI_UNIT ( $, .RADIAN. ) );
#1285 = CARTESIAN_POINT ( 'NONE',  ( 25.64708010899966339, -23.42206246795081981, 110.4552579818684563 ) ) ;
#1286 = CARTESIAN_POINT ( 'NONE',  ( 1.833838850093452599, 138.0075846865486824, -44.84138612520948897 ) ) ;
#1287 = ORIENTED_EDGE ( 'NONE', *, *, #14329, .F. ) ;
#1288 = CARTESIAN_POINT ( 'NONE',  ( 28.37644542392838432, 89.64009552702908934, 86.16884085957975969 ) ) ;
#1289 = CARTESIAN_POINT ( 'NONE',  ( 1.833691583653537016, -125.4903330494893936, -72.86287859464719929 ) ) ;
#1290 = CARTESIAN_POINT ( 'NONE',  ( 25.64681081121879203, -35.28660243342623204, 107.2555980796239936 ) ) ;
#1291 = LINE ( 'NONE', #17250, #16391 ) ;
#1292 = VERTEX_POINT ( 'NONE', #4868 ) ;
#1293 = VERTEX_POINT ( 'NONE', #6897 ) ;
#1294 = CARTESIAN_POINT ( 'NONE',  ( 10.93730112725932635, 0.000000000000000000, 0.000000000000000000 ) ) ;
#1295 = CARTESIAN_POINT ( 'NONE',  ( -20.57838717382308147, -10.78122205917020437, -27.96569011373082603 ) ) ;
#1296 = CARTESIAN_POINT ( 'NONE',  ( 24.22246935314087324, 0.000000000000000000, 0.000000000000000000 ) ) ;
#1297 = CARTESIAN_POINT ( 'NONE',  ( 2.433796855181219243, 144.5536872373191670, 16.65276281464612396 ) ) ;
#1298 = CARTESIAN_POINT ( 'NONE',  ( 10.93730112726003156, 108.9902118373755684, -104.7670965581001781 ) ) ;
#1299 = CARTESIAN_POINT ( 'NONE',  ( -4.178947244162636743, 48.81675275154077553, -3.367451375481286036 ) ) ;
#1300 = CARTESIAN_POINT ( 'NONE',  ( -1.046936909428679119, -45.77873603877005593, 1.275306677858721649 ) ) ;
#1301 = VERTEX_POINT ( 'NONE', #15503 ) ;
#1302 = CARTESIAN_POINT ( 'NONE',  ( 1.833809397773891403, -144.3333383260367668, 14.99109763364097248 ) ) ;
#1303 = CARTESIAN_POINT ( 'NONE',  ( -1.048172774974290178, -1.020161070261438097, -45.78636862970792265 ) ) ;
#1304 = CARTESIAN_POINT ( 'NONE',  ( -20.57838717382308147, -28.96176188950224528, -7.715628353033566533 ) ) ;
#1305 = EDGE_CURVE ( 'NONE', #3709, #21873, #15309, .T. ) ;
#1306 = EDGE_CURVE ( 'NONE', #26104, #26383, #19462, .T. ) ;
#1307 = CARTESIAN_POINT ( 'NONE',  ( 109.1586900883932856, 0.0006456433529069069291, -0.007109207791180753924 ) ) ;
#1308 = ORIENTED_EDGE ( 'NONE', *, *, #24787, .F. ) ;
#1309 = VERTEX_POINT ( 'NONE', #26592 ) ;
#1311 = ADVANCED_FACE ( 'NONE', ( #24462 ), #27356, .F. ) ;
#1310 = CARTESIAN_POINT ( 'NONE',  ( 25.86096068574581253, 22.52859312382188861, 110.7864907291859424 ) ) ;
#1312 = CARTESIAN_POINT ( 'NONE',  ( 2.063896406836609909, -28.88716984836416657, 142.3682421260906779 ) ) ;
#1313 = ORIENTED_EDGE ( 'NONE', *, *, #20571, .F. ) ;
#1314 = EDGE_CURVE ( 'NONE', #18428, #3848, #22295, .T. ) ;
#1315 = ORIENTED_EDGE ( 'NONE', *, *, #6198, .F. ) ;
#1316 = VECTOR ( 'NONE', #10362, 1000.000000000000114 ) ;
#1317 = VERTEX_POINT ( 'NONE', #11066 ) ;
#1318 = B_SPLINE_CURVE_WITH_KNOTS ( 'NONE', 3,
 ( #28279, #19786, #15460, #15322 ),
 .UNSPECIFIED., .F., .F.,
 ( 4, 4 ),
 ( 0.000000000000000000, 0.008383560773332708604 ),
 .UNSPECIFIED. ) ;
#1319 = B_SPLINE_CURVE_WITH_KNOTS ( 'NONE', 3,
 ( #27351, #7664, #14399, #7361, #5191, #16423, #3046, #3324, #23209, #25207 ),
 .UNSPECIFIED., .F., .F.,
 ( 4, 2, 2, 2, 4 ),
 ( 2.877728285596781101E-16, 0.0003346187017559061659, 0.0006692374035115240425, 0.001003856105267141811, 0.001338474807022759687 ),
 .UNSPECIFIED. ) ;
#1320 = B_SPLINE_CURVE_WITH_KNOTS ( 'NONE', 3,
 ( #1056, #9415, #18168, #24823 ),
 .UNSPECIFIED., .F., .F.,
 ( 4, 4 ),
 ( 1.956780383866537384E-16, 0.001982023823822938111 ),
 .UNSPECIFIED. ) ;
#1321 = CARTESIAN_POINT ( 'NONE',  ( -55.25719721206881729, 0.01079965405819919254, 0.002847566758682530588 ) ) ;
#1322 = CARTESIAN_POINT ( 'NONE',  ( 1.833485406944043827, -132.7804117027891948, 58.53321471326832182 ) ) ;
#1323 = FACE_OUTER_BOUND ( 'NONE', #15025, .T. ) ;
#1324 = CARTESIAN_POINT ( 'NONE',  ( -20.47566262905010248, -1.586617686065349808, 29.82700878811085232 ) ) ;
#1325 = CARTESIAN_POINT ( 'NONE',  ( -1.259972190295304939, 2.243354636026407611, 45.95417440459613800 ) ) ;
#1326 = CARTESIAN_POINT ( 'NONE',  ( 10.93730112725932635, 0.000000000000000000, 0.000000000000000000 ) ) ;
#1327 = CARTESIAN_POINT ( 'NONE',  ( 5.340103579038201431, 47.74933483136881307, 139.5040934216401070 ) ) ;
#1328 = CARTESIAN_POINT ( 'NONE',  ( -20.20700224038492721, 24.51628800869048419, -16.58740185276719359 ) ) ;
#1329 = CARTESIAN_POINT ( 'NONE',  ( 16.05277956358213487, 48.70400867629093256, 134.7758735858403440 ) ) ;
#1330 = CARTESIAN_POINT ( 'NONE',  ( 109.1721716018069515, -0.01254847260354027827, -0.01157047143378750823 ) ) ;
#1331 = DIRECTION ( 'NONE',  ( -0.5946245182733607137, -0.6977579871484507201, -0.3994439555666302599 ) ) ;
#1332 = ADVANCED_FACE ( 'NONE', ( #15945 ), #26418, .F. ) ;
#1333 = CARTESIAN_POINT ( 'NONE',  ( -1.113548883309551485, -1.968251867498553409, 45.82026503946953255 ) ) ;
#1334 = CARTESIAN_POINT ( 'NONE',  ( 10.93730112725997294, 36.23586118136742584, -146.7718404940639516 ) ) ;
#1335 = CARTESIAN_POINT ( 'NONE',  ( 109.1586900883932856, -0.005833932871491344374, -0.004113747440992306104 ) ) ;
#1336 = CARTESIAN_POINT ( 'NONE',  ( 1.833750490713715209, -0.2669522761655517273, 145.1094586213657749 ) ) ;
#1337 = ORIENTED_EDGE ( 'NONE', *, *, #26697, .F. ) ;
#1338 = CARTESIAN_POINT ( 'NONE',  ( 109.1624594426973260, 0.01405141589343893681, -0.007576898892904924791 ) ) ;
#1339 = ORIENTED_EDGE ( 'NONE', *, *, #15826, .F. ) ;
#1341 = EDGE_CURVE ( 'NONE', #21070, #7362, #27726, .T. ) ;
#1340 = CARTESIAN_POINT ( 'NONE',  ( 26.11404676487259024, -22.43340081644844020, 110.9778746459746372 ) ) ;
#1343 = VERTEX_POINT ( 'NONE', #16675 ) ;
#1342 = LINE ( 'NONE', #14142, #24030 ) ;
#1344 = ORIENTED_EDGE ( 'NONE', *, *, #7073, .T. ) ;
#1345 =( BOUNDED_SURFACE ( )  B_SPLINE_SURFACE ( 3, 1, ( 
 ( #793, #25127 ),
 ( #18332, #20364 ),
 ( #9300, #7425 ),
 ( #4964, #13596 ) ),
 .UNSPECIFIED., .F., .F., .F. ) 
 B_SPLINE_SURFACE_WITH_KNOTS ( ( 4, 4 ),
 ( 2, 2 ),
 ( 0.000000000000000000, 1.000000000000000000 ),
 ( 0.000000000000000000, 1.000000000000000000 ),
 .UNSPECIFIED. ) 
 GEOMETRIC_REPRESENTATION_ITEM ( )  RATIONAL_B_SPLINE_SURFACE ( (
 ( 1.000000000000000000, 1.000000000000000000),
 ( 0.9960225298536222738, 0.9999952330161893110),
 ( 0.9960225298536222738, 0.9999952330161893110),
 ( 1.000000000000000000, 1.000000000000000000) ) ) 
 REPRESENTATION_ITEM ( '' )  SURFACE ( )  );
#1346 = ORIENTED_EDGE ( 'NONE', *, *, #9836, .F. ) ;
#1347 = EDGE_LOOP ( 'NONE', ( #5434, #21722, #24363, #12048 ) ) ;
#1348 = B_SPLINE_CURVE_WITH_KNOTS ( 'NONE', 3,
 ( #18015, #8682, #26804, #17869, #26515, #11406, #15424, #10990, #15565, #20326 ),
 .UNSPECIFIED., .F., .F.,
 ( 4, 2, 2, 2, 4 ),
 ( 2.913600445039318278E-16, 0.0003346187017559067080, 0.0006692374035115219826, 0.001003856105267137474, 0.001338474807022752748 ),
 .UNSPECIFIED. ) ;
#1349 = CARTESIAN_POINT ( 'NONE',  ( 2.433796855181233454, -118.5671979538051062, -84.34988187691051564 ) ) ;
#1350 = CARTESIAN_POINT ( 'NONE',  ( -1.031422197589711987, -43.06660437151296605, 15.60268798220683273 ) ) ;
#1351 = CARTESIAN_POINT ( 'NONE',  ( -22.23342874802668589, 24.24669006619402367, 20.31166691703097982 ) ) ;
#1352 = CARTESIAN_POINT ( 'NONE',  ( 2.430230287190581429, 13.76600171652644278, 144.8619874886007324 ) ) ;
#1353 = CARTESIAN_POINT ( 'NONE',  ( -20.57838717382308147, 29.92853265176831812, -1.611677988432464126 ) ) ;
#1354 = CARTESIAN_POINT ( 'NONE',  ( 55.79472521941426777, 68.96476385670665366, 23.17337251492787331 ) ) ;
#1355 = EDGE_LOOP ( 'NONE', ( #18978, #2999, #769, #14797 ) ) ;
#1356 = VERTEX_POINT ( 'NONE', #16376 ) ;
#1357 = CARTESIAN_POINT ( 'NONE',  ( 1.833485406944043827, -29.64752363041439764, -142.0485807715649003 ) ) ;
#1358 = B_SPLINE_CURVE_WITH_KNOTS ( 'NONE', 3,
 ( #21003, #1288, #1576, #3588, #14230, #14386, #5622 ),
 .UNSPECIFIED., .F., .F.,
 ( 4, 3, 4 ),
 ( 0.000000000000000000, 0.02398743853561353251, 0.04000277880656209761 ),
 .UNSPECIFIED. ) ;
#1360 = CARTESIAN_POINT ( 'NONE',  ( 25.64681081121879203, -91.10197563707990298, 66.70335573067838197 ) ) ;
#1359 = CARTESIAN_POINT ( 'NONE',  ( 1.893872463202038503, 144.4512189534319759, -14.22435552397860548 ) ) ;
#1361 = EDGE_CURVE ( 'NONE', #5981, #19211, #7343, .T. ) ;
#1362 = CARTESIAN_POINT ( 'NONE',  ( -2.911734481061404534, -17.36785190846011417, -44.38410240830297226 ) ) ;
#1363 = DIRECTION ( 'NONE',  ( 0.000000000000000000, 5.223019709708190374E-21, -1.000000000000000000 ) ) ;
#1364 = CARTESIAN_POINT ( 'NONE',  ( -55.25297051322618813, 0.01306918787467630481, -0.007247191603131783282 ) ) ;
#1365 = B_SPLINE_CURVE_WITH_KNOTS ( 'NONE', 3,
 ( #21938, #28258, #26530, #4092, #8558, #4376, #13429, #17324 ),
 .UNSPECIFIED., .F., .F.,
 ( 4, 2, 2, 4 ),
 ( 2.251264292202123005E-16, 0.002761568181852872006, 0.005523136363705519365, 0.01104627272741081322 ),
 .UNSPECIFIED. ) ;
#1366 = ORIENTED_EDGE ( 'NONE', *, *, #5235, .T. ) ;
#1367 = LINE ( 'NONE', #12307, #28094 ) ;
#1368 = AXIS2_PLACEMENT_3D ( 'NONE', #560, #24901, #18110 ) ;
#1369 = EDGE_CURVE ( 'NONE', #4903, #16481, #21061, .T. ) ;
#1370 = ORIENTED_EDGE ( 'NONE', *, *, #1908, .F. ) ;
#1371 = CARTESIAN_POINT ( 'NONE',  ( -4.473127245936434626, 12.17046501147516224, -47.80062405537804437 ) ) ;
#1372 = EDGE_CURVE ( 'NONE', #7217, #13229, #23622, .T. ) ;
#1373 = CARTESIAN_POINT ( 'NONE',  ( -1.113427685307002424, -38.22586258295212502, -25.34053733836516642 ) ) ;
#1374 = ORIENTED_EDGE ( 'NONE', *, *, #24628, .T. ) ;
#1375 = ORIENTED_EDGE ( 'NONE', *, *, #8006, .F. ) ;
#1376 = B_SPLINE_CURVE_WITH_KNOTS ( 'NONE', 3,
 ( #2464, #18147, #24801, #20166, #22491, #11117 ),
 .UNSPECIFIED., .F., .F.,
 ( 4, 2, 4 ),
 ( 2.168404344971008868E-18, 0.0006311636237756793446, 0.001262327247551356521 ),
 .UNSPECIFIED. ) ;
#1377 = EDGE_CURVE ( 'NONE', #1601, #19236, #20169, .T. ) ;
#1378 = CARTESIAN_POINT ( 'NONE',  ( 1.833603222531971610, 96.76619886578326657, 108.1346772638449920 ) ) ;
#1379 = ORIENTED_EDGE ( 'NONE', *, *, #19031, .T. ) ;
#1380 = CARTESIAN_POINT ( 'NONE',  ( -20.57838717382308147, 1.611677988432361097, -29.92853265176831812 ) ) ;
#1381 = CIRCLE ( 'NONE', #12420, 117.6351876552689504 ) ;
#1382 = LINE ( 'NONE', #3688, #374 ) ;
#1383 = CARTESIAN_POINT ( 'NONE',  ( -55.24728320129491266, -0.003868537197316565448, -0.01402509393918558236 ) ) ;
#1384 = CARTESIAN_POINT ( 'NONE',  ( 109.1592201516379674, 0.0005146241775907373474, -0.007845213074660002325 ) ) ;
#1385 = CARTESIAN_POINT ( 'NONE',  ( 2.433796855181233454, 138.8296532063088193, 43.58222566461690661 ) ) ;
#1386 = CARTESIAN_POINT ( 'NONE',  ( 1.833603222531971610, 0.4449221977539696282, -145.1089511853978422 ) ) ;
#1387 = CARTESIAN_POINT ( 'NONE',  ( 1.894214914920927528, -141.7768822502889066, 31.11059045489088959 ) ) ;
#1388 = ORIENTED_EDGE ( 'NONE', *, *, #13947, .T. ) ;
#1389 = EDGE_CURVE ( 'NONE', #18251, #1487, #10971, .T. ) ;
#1390 = CARTESIAN_POINT ( 'NONE',  ( 6.224689322667630975, -12.92299475786858842, -147.4941644018829265 ) ) ;
#1392 = CARTESIAN_POINT ( 'NONE',  ( 2.430230287190572103, 16.65331920325932202, -144.5585181921884157 ) ) ;
#1391 = CARTESIAN_POINT ( 'NONE',  ( 1.833485406944043827, 14.63699153649359452, 144.3694338680885778 ) ) ;
#1393 = DIRECTION ( 'NONE',  ( -0.7563875759206388771, -0.2351350468682952832, -0.6104009704506900835 ) ) ;
#1394 = EDGE_LOOP ( 'NONE', ( #26087, #3282, #16540, #13815 ) ) ;
#1395 = ORIENTED_EDGE ( 'NONE', *, *, #16762, .F. ) ;
#1396 = ORIENTED_EDGE ( 'NONE', *, *, #581, .F. ) ;
#1397 = CARTESIAN_POINT ( 'NONE',  ( -2.911734481061388990, -47.57875121082950898, 2.802366807346684308 ) ) ;
#1398 = CARTESIAN_POINT ( 'NONE',  ( 32.73300124599732186, 0.000000000000000000, 0.000000000000000000 ) ) ;
#1400 = DIRECTION ( 'NONE',  ( 1.000000000000000000, -6.938893903907226837E-18, 1.734723475976806709E-18 ) ) ;
#1399 = CARTESIAN_POINT ( 'NONE',  ( 10.93730112725932635, 0.000000000000000000, 0.000000000000000000 ) ) ;
#1401 = EDGE_CURVE ( 'NONE', #28403, #12613, #18443, .T. ) ;
#1402 = CARTESIAN_POINT ( 'NONE',  ( 1.833838848569454782, -132.6367525013572788, -58.85887272891319810 ) ) ;
#1403 = LINE ( 'NONE', #14504, #20757 ) ;
#1404 = CARTESIAN_POINT ( 'NONE',  ( -1.323830074806765289, -28.92190886481839129, 35.86387698262947055 ) ) ;
#1405 = VERTEX_POINT ( 'NONE', #3286 ) ;
#1406 = CARTESIAN_POINT ( 'NONE',  ( -20.20700224038492010, -10.08426345511570332, 27.82980252387829623 ) ) ;
#1407 = CARTESIAN_POINT ( 'NONE',  ( 30.59141879584313628, 14.83090566979595870, -115.2623358717303717 ) ) ;
#1408 = CARTESIAN_POINT ( 'NONE',  ( -1.048996300304495310, 13.42280206896976757, -43.78665266739842110 ) ) ;
#1409 = FACE_OUTER_BOUND ( 'NONE', #777, .T. ) ;
#1410 = CIRCLE ( 'NONE', #21621, 34.60786435723138510 ) ;
#1411 = CARTESIAN_POINT ( 'NONE',  ( -55.24390624410018802, -0.01027195578987734684, 0.001811362924359352471 ) ) ;
#1413 = VECTOR ( 'NONE', #12119, 1000.000000000000114 ) ;
#1412 = CARTESIAN_POINT ( 'NONE',  ( -4.162674018437148682, 41.48630000627055381, -25.90909455705125453 ) ) ;
#1414 = CARTESIAN_POINT ( 'NONE',  ( 30.58324630866352578, 112.0331114996534296, 45.56259622822393851 ) ) ;
#1415 = AXIS2_PLACEMENT_3D ( 'NONE', #17030, #21631, #21494 ) ;
#1416 = VERTEX_POINT ( 'NONE', #7914 ) ;
#1417 = CARTESIAN_POINT ( 'NONE',  ( 28.37644542392843405, 54.25112470585876423, -111.8804331835009691 ) ) ;
#1418 = CONICAL_SURFACE ( 'NONE', #26670, 117.6351876552689504, 0.9945805576725580410 ) ;
#1419 = CARTESIAN_POINT ( 'NONE',  ( 1.834118845439484335, 117.5010238212698823, 85.14950727125895469 ) ) ;
#1420 = CARTESIAN_POINT ( 'NONE',  ( 1.833206310202323053, -137.7753867363981044, 45.54896489827107331 ) ) ;
#1421 = VERTEX_POINT ( 'NONE', #27309 ) ;
#1422 = CARTESIAN_POINT ( 'NONE',  ( -1.583189561560252701, -11.94859433442933394, -44.83405390829668136 ) ) ;
#1423 = VERTEX_POINT ( 'NONE', #18543 ) ;
#1425 = B_SPLINE_CURVE_WITH_KNOTS ( 'NONE', 3,
 ( #17345, #8305, #6424, #12608, #28418, #8580, #11028, #21678, #26134, #15323 ),
 .UNSPECIFIED., .F., .F.,
 ( 4, 3, 3, 4 ),
 ( 5.003707553108401214E-17, 0.0002669559177086402351, 0.0005339118354150940680, 0.001067817517169129121 ),
 .UNSPECIFIED. ) ;
#1424 = CARTESIAN_POINT ( 'NONE',  ( 28.37599760073042532, -68.88138253892459772, 91.75439000741670270 ) ) ;
#1426 = CARTESIAN_POINT ( 'NONE',  ( -18.41936578851719730, -37.37524689996168803, 20.09935324538230006 ) ) ;
#1427 = B_SPLINE_CURVE_WITH_KNOTS ( 'NONE', 3,
 ( #875, #27056, #7364, #14244, #18274, #23068 ),
 .UNSPECIFIED., .F., .F.,
 ( 4, 2, 4 ),
 ( 3.903127820947815962E-18, 0.0006311636237756693699, 0.001262327247551335054 ),
 .UNSPECIFIED. ) ;
#1428 = SURFACE_STYLE_FILL_AREA ( #7790 ) ;
#1429 = VECTOR ( 'NONE', #12856, 1000.000000000000000 ) ;
#1430 = CARTESIAN_POINT ( 'NONE',  ( 10.93730112725943471, 125.1380233598475229, 84.82621002473483429 ) ) ;
#1431 = CARTESIAN_POINT ( 'NONE',  ( 19.66333377628719958, 136.4524620437343003, 18.85786579349995762 ) ) ;
#1432 = CIRCLE ( 'NONE', #11088, 117.6351876552689504 ) ;
#1433 = CARTESIAN_POINT ( 'NONE',  ( -7.711401346138400115, 38.61705198405368122, -35.51061203065540894 ) ) ;
#1434 = EDGE_CURVE ( 'NONE', #24791, #813, #8161, .T. ) ;
#1435 = DIRECTION ( 'NONE',  ( -1.000000000000000000, 6.938893903907226837E-18, -1.734723475976806709E-18 ) ) ;
#1436 = CARTESIAN_POINT ( 'NONE',  ( 1.833485406944043827, -15.69895494453482598, 144.2578170162062463 ) ) ;
#1437 = EDGE_LOOP ( 'NONE', ( #9079, #697, #16838, #10518 ) ) ;
#1438 = CIRCLE ( 'NONE', #12458, 117.6351876552689504 ) ;
#1439 = ADVANCED_FACE ( 'NONE', ( #9618 ), #16507, .F. ) ;
#1440 = ORIENTED_EDGE ( 'NONE', *, *, #23420, .F. ) ;
#1441 = CARTESIAN_POINT ( 'NONE',  ( -16.86833981943423666, 43.51541671545732726, 7.884812276281646604 ) ) ;
#1442 = CARTESIAN_POINT ( 'NONE',  ( 2.430230287190572103, -109.1043569252020831, 96.28466919684061054 ) ) ;
#1443 = CARTESIAN_POINT ( 'NONE',  ( 1.832998868059890096, 132.3466930259802439, -59.50898020732379479 ) ) ;
#1444 = PLANE ( 'NONE',  #8294 ) ;
#1445 = CARTESIAN_POINT ( 'NONE',  ( 25.69398547355839924, -91.80679989327096280, -65.78402800526257010 ) ) ;
#1446 = CARTESIAN_POINT ( 'NONE',  ( 1.833809397773874084, -138.0624841332890753, 44.67209459545020422 ) ) ;
#1447 = FACE_OUTER_BOUND ( 'NONE', #21884, .T. ) ;
#1448 = ORIENTED_EDGE ( 'NONE', *, *, #26567, .F. ) ;
#1449 = CARTESIAN_POINT ( 'NONE',  ( 2.433796855181205476, 57.85512797797890272, 133.5135467655520074 ) ) ;
#1450 = CARTESIAN_POINT ( 'NONE',  ( -1.019300379054419947, -45.76814864815092676, -2.023851374322514829 ) ) ;
#1451 = CARTESIAN_POINT ( 'NONE',  ( 25.73574536432414561, -11.00659994954073184, -112.4329083163019618 ) ) ;
#1452 = B_SPLINE_CURVE_WITH_KNOTS ( 'NONE', 3,
 ( #16150, #24955, #5215, #13989, #22799, #20610, #894 ),
 .UNSPECIFIED., .F., .F.,
 ( 4, 3, 4 ),
 ( 2.299948302575412283E-16, 0.009512539173626367167, 0.02506242213020821313 ),
 .UNSPECIFIED. ) ;
#1453 = CARTESIAN_POINT ( 'NONE',  ( -20.57838717382308147, -25.16001208503117326, -16.28767523336112433 ) ) ;
#1454 = CARTESIAN_POINT ( 'NONE',  ( 2.430230287190592531, 107.1617224697477297, -98.44218333480665706 ) ) ;
#1455 = ORIENTED_EDGE ( 'NONE', *, *, #12599, .T. ) ;
#1456 = AXIS2_PLACEMENT_3D ( 'NONE', #12266, #5805, #12682 ) ;
#1457 = CARTESIAN_POINT ( 'NONE',  ( 25.64699802086724034, -12.03888878460397649, -112.2675771984165607 ) ) ;
#1458 = ORIENTED_EDGE ( 'NONE', *, *, #25670, .F. ) ;
#1459 = PRESENTATION_LAYER_ASSIGNMENT (  '', '', ( #10212 ) ) ;
#1460 = ORIENTED_EDGE ( 'NONE', *, *, #20738, .T. ) ;
#1461 = VERTEX_POINT ( 'NONE', #14069 ) ;
#1462 = AXIS2_PLACEMENT_3D ( 'NONE', #2300, #22338, #22187 ) ;
#1463 = CARTESIAN_POINT ( 'NONE',  ( 2.263178113027036531, 28.85718369185711651, 142.5035404044874952 ) ) ;
#1464 = CARTESIAN_POINT ( 'NONE',  ( 109.1592201516379674, 0.007780772729118878156, 0.001127733110579607657 ) ) ;
#1465 = EDGE_CURVE ( 'NONE', #27866, #2646, #5439, .T. ) ;
#1466 = EDGE_CURVE ( 'NONE', #20633, #26751, #7143, .T. ) ;
#1467 = CARTESIAN_POINT ( 'NONE',  ( 1.893872463202069145, -132.9857054814983712, 58.16604752596676775 ) ) ;
#1468 = CARTESIAN_POINT ( 'NONE',  ( 55.49584447822657296, -54.09506550945592807, -48.34726110740042060 ) ) ;
#1469 = EDGE_CURVE ( 'NONE', #11691, #24126, #12925, .T. ) ;
#1470 = DIRECTION ( 'NONE',  ( -1.000000000000000000, -0.000000000000000000, -0.000000000000000000 ) ) ;
#1471 = CARTESIAN_POINT ( 'NONE',  ( 30.59141879584283430, -26.79785525806475377, 113.0806649571965465 ) ) ;
#1472 = CARTESIAN_POINT ( 'NONE',  ( -20.24419206586951603, 24.70913649113854049, 16.36655224501340555 ) ) ;
#1473 = EDGE_CURVE ( 'NONE', #21210, #26606, #26990, .T. ) ;
#1474 = CARTESIAN_POINT ( 'NONE',  ( 1.832998868059890096, 144.2584710144580242, 15.69902610990420122 ) ) ;
#1475 = CARTESIAN_POINT ( 'NONE',  ( 25.64708228042118421, -75.52311986517973708, -83.93578330383164143 ) ) ;
#1476 = CARTESIAN_POINT ( 'NONE',  ( 2.430230287190592531, 84.35270093935415048, -118.5711603495673074 ) ) ;
#1477 = CONICAL_SURFACE ( 'NONE', #24938, 34.60786435723138510, 0.8559913436420825139 ) ;
#1478 = CARTESIAN_POINT ( 'NONE',  ( 25.73574536432415272, -112.9674920590232716, -0.8061344836380949230 ) ) ;
#1479 = CARTESIAN_POINT ( 'NONE',  ( -55.25297051322618813, -0.01483298743814594547, 0.001818774723749421287 ) ) ;
#1480 = PLANE ( 'NONE',  #4389 ) ;
#1481 = CARTESIAN_POINT ( 'NONE',  ( 13.36082413113063083, 70.90215303572314554, -135.4964217943299900 ) ) ;
#1482 = CARTESIAN_POINT ( 'NONE',  ( 25.64670758986457955, 102.9458331681485532, 46.37945960491909148 ) ) ;
#1483 = ORIENTED_EDGE ( 'NONE', *, *, #25373, .T. ) ;
#1484 = VERTEX_POINT ( 'NONE', #10762 ) ;
#1485 = CARTESIAN_POINT ( 'NONE',  ( -1.239374126674604337, -16.50008610789269170, 42.99367564261294206 ) ) ;
#1487 = VERTEX_POINT ( 'NONE', #4124 ) ;
#1486 = CARTESIAN_POINT ( 'NONE',  ( -1.050229599974477290, 26.71319688967688322, 37.20249516760145525 ) ) ;
#1488 = ORIENTED_EDGE ( 'NONE', *, *, #1237, .F. ) ;
#1489 = ORIENTED_EDGE ( 'NONE', *, *, #16081, .F. ) ;
#1490 = VERTEX_POINT ( 'NONE', #19523 ) ;
#1491 = CONICAL_SURFACE ( 'NONE', #18480, 117.6351876552689504, 0.9945805576725580410 ) ;
#1492 = VECTOR ( 'NONE', #28184, 1000.000000000000114 ) ;
#1493 = EDGE_CURVE ( 'NONE', #26004, #9976, #25660, .T. ) ;
#1494 = CARTESIAN_POINT ( 'NONE',  ( -20.38016308990357217, 16.25718651464982045, -24.94368798801356490 ) ) ;
#1495 = DIRECTION ( 'NONE',  ( -1.000000000000000000, 6.938893903907226837E-18, -1.734723475976806709E-18 ) ) ;
#1496 = EDGE_CURVE ( 'NONE', #733, #1672, #24988, .T. ) ;
#1497 = CARTESIAN_POINT ( 'NONE',  ( -20.57838717382308147, 1.611677988432778319, 29.92853265176829325 ) ) ;
#1498 = DIRECTION ( 'NONE',  ( -1.000000000000000000, -0.000000000000000000, -0.000000000000000000 ) ) ;
#1499 = DIRECTION ( 'NONE',  ( -0.000000000000000000, 1.000000000000000000, -0.000000000000000000 ) ) ;
#1500 = CARTESIAN_POINT ( 'NONE',  ( -55.25297051322618813, 0.001818774723749745246, 0.01483298743814625079 ) ) ;
#1501 = CARTESIAN_POINT ( 'NONE',  ( -24.53237795827028123, -6.738475012719871593, 33.25734978085275628 ) ) ;
#1502 = ORIENTED_EDGE ( 'NONE', *, *, #19891, .T. ) ;
#1503 = VERTEX_POINT ( 'NONE', #9304 ) ;
#1504 = VECTOR ( 'NONE', #23787, 1000.000000000000114 ) ;
#1505 = CARTESIAN_POINT ( 'NONE',  ( -6.588769196390771299, 11.07780292579764847, 50.13301368233286581 ) ) ;
#1507 = CARTESIAN_POINT ( 'NONE',  ( -1.619063947482197729, -38.92136151114925724, -25.20140673341360227 ) ) ;
#1506 = CARTESIAN_POINT ( 'NONE',  ( 1.833485406944043827, 132.7804117027896211, -58.53321471326746916 ) ) ;
#1508 = B_SPLINE_CURVE_WITH_KNOTS ( 'NONE', 3,
 ( #7576, #3239, #14160, #14735, #12021, #23121 ),
 .UNSPECIFIED., .F., .F.,
 ( 4, 2, 4 ),
 ( 2.602085213965210642E-18, 0.0006311636237756765256, 0.001262327247551350666 ),
 .UNSPECIFIED. ) ;
#1509 = CARTESIAN_POINT ( 'NONE',  ( 10.93730112725972070, -26.59437931460858451, 148.8212007290659642 ) ) ;
#1510 = CARTESIAN_POINT ( 'NONE',  ( 109.1586900883932856, 0.006479576224403786264, 0.002995460350180832385 ) ) ;
#1511 = CARTESIAN_POINT ( 'NONE',  ( 26.11404676487257603, 33.91085499298520034, -108.0249973236464314 ) ) ;
#1513 =( BOUNDED_SURFACE ( )  B_SPLINE_SURFACE ( 3, 1, ( 
 ( #4474, #3570 ),
 ( #6038, #10223 ),
 ( #25616, #10486 ),
 ( #23031, #1138 ) ),
 .UNSPECIFIED., .F., .F., .F. ) 
 B_SPLINE_SURFACE_WITH_KNOTS ( ( 4, 4 ),
 ( 2, 2 ),
 ( 0.000000000000000000, 1.000000000000000000 ),
 ( 0.000000000000000000, 1.000000000000000000 ),
 .UNSPECIFIED. ) 
 GEOMETRIC_REPRESENTATION_ITEM ( )  RATIONAL_B_SPLINE_SURFACE ( (
 ( 1.000000000000000000, 1.000000000000000000),
 ( 0.7789835883360578528, 0.9689951854195403280),
 ( 0.7789835883360578528, 0.9689951854195403280),
 ( 1.000000000000000000, 1.000000000000000000) ) ) 
 REPRESENTATION_ITEM ( '' )  SURFACE ( )  );
#1512 = CONICAL_SURFACE ( 'NONE', #26330, 34.60786435723138510, 0.8559913436420825139 ) ;
#1514 = EDGE_LOOP ( 'NONE', ( #16978, #15733, #24881, #15385, #5827, #11832 ) ) ;
#1515 = CARTESIAN_POINT ( 'NONE',  ( -1.619063947482197729, -25.20140673341401438, -38.92136151114898723 ) ) ;
#1516 = CONICAL_SURFACE ( 'NONE', #12542, 34.60786435723138510, 0.8559913436420825139 ) ;
#1517 = CARTESIAN_POINT ( 'NONE',  ( -1.583189561560252701, -46.33203782964464068, -2.490696082059713046 ) ) ;
#1518 = CARTESIAN_POINT ( 'NONE',  ( -20.57838717382308502, 25.16001208503106668, -16.28767523336130196 ) ) ;
#1519 = ORIENTED_EDGE ( 'NONE', *, *, #10871, .T. ) ;
#1520 = ORIENTED_EDGE ( 'NONE', *, *, #2351, .T. ) ;
#1521 = FACE_OUTER_BOUND ( 'NONE', #17886, .T. ) ;
#1522 = ORIENTED_EDGE ( 'NONE', *, *, #2533, .F. ) ;
#1523 = VERTEX_POINT ( 'NONE', #15912 ) ;
#1524 = VECTOR ( 'NONE', #8411, 1000.000000000000341 ) ;
#1525 = CARTESIAN_POINT ( 'NONE',  ( 30.58324630866343696, 95.47492154584260504, -74.24222250960141878 ) ) ;
#1526 = ORIENTED_EDGE ( 'NONE', *, *, #25692, .T. ) ;
#1527 = CARTESIAN_POINT ( 'NONE',  ( 1.834118845439484335, -144.2964192726483361, 15.34511559672636238 ) ) ;
#1528 = DIRECTION ( 'NONE',  ( 0.000000000000000000, 0.000000000000000000, 1.000000000000000000 ) ) ;
#1529 = EDGE_CURVE ( 'NONE', #7265, #5626, #3649, .T. ) ;
#1530 = AXIS2_PLACEMENT_3D ( 'NONE', #12824, #19308, #6236 ) ;
#1531 = CARTESIAN_POINT ( 'NONE',  ( -1.045287976400379737, 44.00138577190644185, -12.68782741917337198 ) ) ;
#1532 = AXIS2_PLACEMENT_3D ( 'NONE', #8845, #27889, #10356 ) ;
#1533 = EDGE_CURVE ( 'NONE', #6666, #21211, #6780, .T. ) ;
#1534 = CARTESIAN_POINT ( 'NONE',  ( 109.1624594426973260, 0.01263706729758982267, 0.009754804742273323268 ) ) ;
#1535 = CARTESIAN_POINT ( 'NONE',  ( 32.73300124599735028, 110.6325518752274206, 39.98094346392350218 ) ) ;
#1536 = EDGE_CURVE ( 'NONE', #18316, #12676, #798, .T. ) ;
#1537 = CARTESIAN_POINT ( 'NONE',  ( 109.1778270068192853, 0.006682187084648908565, -0.006489198140359554549 ) ) ;
#1538 = FACE_OUTER_BOUND ( 'NONE', #5157, .T. ) ;
#1539 = LINE ( 'NONE', #14775, #20543 ) ;
#1540 = ORIENTED_EDGE ( 'NONE', *, *, #10596, .T. ) ;
#1541 = ORIENTED_EDGE ( 'NONE', *, *, #14828, .T. ) ;
#1542 = CARTESIAN_POINT ( 'NONE',  ( -22.34422965417122953, 6.759368364654329220, -37.30738373203623581 ) ) ;
#1543 = CARTESIAN_POINT ( 'NONE',  ( -12.94347594948482083, -33.69581619287849605, 35.22469990145643948 ) ) ;
#1544 = FACE_OUTER_BOUND ( 'NONE', #24260, .T. ) ;
#1545 = CARTESIAN_POINT ( 'NONE',  ( -20.57838717382308147, -7.715628353033481268, 28.96176188950225949 ) ) ;
#1546 = B_SPLINE_CURVE_WITH_KNOTS ( 'NONE', 3,
 ( #19880, #13249, #168, #4623, #4772, #14211 ),
 .UNSPECIFIED., .F., .F.,
 ( 4, 2, 4 ),
 ( 0.000000000000000000, 0.0004335184443140242989, 0.0008670368886280485979 ),
 .UNSPECIFIED. ) ;
#1547 = CARTESIAN_POINT ( 'NONE',  ( 10.93730112725971892, -10.89264110825104837, 150.7858122213660863 ) ) ;
#1548 = ORIENTED_EDGE ( 'NONE', *, *, #348, .T. ) ;
#1549 = LINE ( 'NONE', #14785, #11108 ) ;
#1550 = CARTESIAN_POINT ( 'NONE',  ( -25.21435515916025594, 1.749597353048488237E-16, -4.373993382621220594E-17 ) ) ;
#1551 = ORIENTED_EDGE ( 'NONE', *, *, #5562, .T. ) ;
#1552 = CARTESIAN_POINT ( 'NONE',  ( -18.41936578851709783, 37.37524689996197935, -20.09935324538209045 ) ) ;
#1553 = CARTESIAN_POINT ( 'NONE',  ( 99.22246935314079508, 90.00000000000005684, 39.99999999999999289 ) ) ;
#1554 =( BOUNDED_SURFACE ( )  B_SPLINE_SURFACE ( 3, 1, ( 
 ( #14884, #23547 ),
 ( #5983, #18783 ),
 ( #8276, #27556 ),
 ( #16631, #1641 ) ),
 .UNSPECIFIED., .F., .F., .F. ) 
 B_SPLINE_SURFACE_WITH_KNOTS ( ( 4, 4 ),
 ( 2, 2 ),
 ( 0.000000000000000000, 1.000000000000000000 ),
 ( 0.000000000000000000, 1.000000000000000000 ),
 .UNSPECIFIED. ) 
 GEOMETRIC_REPRESENTATION_ITEM ( )  RATIONAL_B_SPLINE_SURFACE ( (
 ( 1.000000000000000000, 1.000000000000000000),
 ( 0.9960225298536222738, 0.9999952330161893110),
 ( 0.9960225298536222738, 0.9999952330161893110),
 ( 1.000000000000000000, 1.000000000000000000) ) ) 
 REPRESENTATION_ITEM ( '' )  SURFACE ( )  );
#1555 = CARTESIAN_POINT ( 'NONE',  ( 109.1586059443104944, -0.004524147648825598347, 0.005438258427231118172 ) ) ;
#1556 = CARTESIAN_POINT ( 'NONE',  ( 25.64670758986456889, 75.18147256662052769, 84.24158725144647519 ) ) ;
#1557 = CARTESIAN_POINT ( 'NONE',  ( 25.64670758986457955, -110.5460908981863355, 22.98827151089250620 ) ) ;
#1558 = CARTESIAN_POINT ( 'NONE',  ( -6.574463467970655728, 34.08059230520098737, 38.37705091668339463 ) ) ;
#1559 = EDGE_LOOP ( 'NONE', ( #15507, #13669, #15161, #23910 ) ) ;
#1560 = CARTESIAN_POINT ( 'NONE',  ( -55.25719721206881729, -0.006045473558784038998, 0.009391134844733136505 ) ) ;
#1561 = CARTESIAN_POINT ( 'NONE',  ( -23.79248802219731473, -16.82188324679459868, 28.61009539422402881 ) ) ;
#1562 = EDGE_CURVE ( 'NONE', #10623, #9334, #17413, .T. ) ;
#1563 = CARTESIAN_POINT ( 'NONE',  ( 109.1624594426973118, 0.004489871836309348475, -0.01531968460306870790 ) ) ;
#1564 = ORIENTED_EDGE ( 'NONE', *, *, #24628, .F. ) ;
#1565 = EDGE_CURVE ( 'NONE', #9768, #14537, #9530, .T. ) ;
#1566 = DIRECTION ( 'NONE',  ( 0.7637818620346800147, -0.1788995134688871336, -0.6201872550346648749 ) ) ;
#1567 = B_SPLINE_CURVE_WITH_KNOTS ( 'NONE', 3,
 ( #1677, #15049, #6579, #12755, #4402, #8591, #19656 ),
 .UNSPECIFIED., .F., .F.,
 ( 4, 3, 4 ),
 ( 0.000000000000000000, 0.02398743853561352557, 0.04000277880656212537 ),
 .UNSPECIFIED. ) ;
#1568 = B_SPLINE_CURVE_WITH_KNOTS ( 'NONE', 3,
 ( #15627, #5140, #20244, #13629 ),
 .UNSPECIFIED., .F., .F.,
 ( 4, 4 ),
 ( 0.000000000000000000, 0.008383560773332734625 ),
 .UNSPECIFIED. ) ;
#1569 = ADVANCED_FACE ( 'NONE', ( #12171 ), #3820, .F. ) ;
#1570 = CARTESIAN_POINT ( 'NONE',  ( -1.464342487929843006, -11.94843286121887438, 44.64187261869788870 ) ) ;
#1571 = CARTESIAN_POINT ( 'NONE',  ( -1.049817751779889008, -43.39729912094389874, -14.63752841325032250 ) ) ;
#1572 = EDGE_CURVE ( 'NONE', #23165, #26, #27367, .T. ) ;
#1573 = CARTESIAN_POINT ( 'NONE',  ( -21.41427618760446450, 1.815001260755841450, -30.75468365310879193 ) ) ;
#1574 = CARTESIAN_POINT ( 'NONE',  ( -28.41354790283022069, -12.60397206714818097, 19.47297445639563307 ) ) ;
#1575 = CARTESIAN_POINT ( 'NONE',  ( 26.11404676487257603, -107.3263591096427945, -36.06104232266560672 ) ) ;
#1576 = CARTESIAN_POINT ( 'NONE',  ( 24.01988960052055333, 94.47404045191640876, 90.81495976423825311 ) ) ;
#1577 = B_SPLINE_CURVE_WITH_KNOTS ( 'NONE', 3,
 ( #19975, #15364, #8911, #22290, #15496, #4571, #17528, #2550 ),
 .UNSPECIFIED., .F., .F.,
 ( 4, 2, 2, 4 ),
 ( 3.469446951953614189E-18, 0.0002429592666046673818, 0.0004859185332093312942, 0.0009718370664186931629 ),
 .UNSPECIFIED. ) ;
#1578 = CARTESIAN_POINT ( 'NONE',  ( -1.058197053496163109, -28.32422455455050425, 36.00048521498983689 ) ) ;
#1579 = CARTESIAN_POINT ( 'NONE',  ( 10.93730112725932635, 0.000000000000000000, 0.000000000000000000 ) ) ;
#1580 = CARTESIAN_POINT ( 'NONE',  ( -1.113427685306995318, 28.52429901637220411, 35.91272432484627330 ) ) ;
#1581 = VERTEX_POINT ( 'NONE', #5113 ) ;
#1582 = ORIENTED_EDGE ( 'NONE', *, *, #26831, .T. ) ;
#1583 = CARTESIAN_POINT ( 'NONE',  ( 25.64670758986457955, -97.53391148296633162, -56.88615781331589716 ) ) ;
#1584 = FACE_OUTER_BOUND ( 'NONE', #1559, .T. ) ;
#1585 = CARTESIAN_POINT ( 'NONE',  ( 16.05277956358202474, -87.96830019103585130, -113.1291064380272218 ) ) ;
#1586 = CARTESIAN_POINT ( 'NONE',  ( -1.113427685307000203, 12.28784199929934751, -44.18561238466741514 ) ) ;
#1587 = CARTESIAN_POINT ( 'NONE',  ( -1.155001620486242553, 42.97366440495935080, 16.13799328198379257 ) ) ;
#1588 = CARTESIAN_POINT ( 'NONE',  ( 1.833485406944043827, -144.2578170162061895, -15.69895494453532869 ) ) ;
#1589 = CARTESIAN_POINT ( 'NONE',  ( 26.28373643307403640, -48.05579805965621176, 118.1623717393434418 ) ) ;
#1590 = EDGE_LOOP ( 'NONE', ( #5054, #21491, #20191, #21560 ) ) ;
#1591 = DIRECTION ( 'NONE',  ( -1.000000000000000000, -0.000000000000000000, -0.000000000000000000 ) ) ;
#1592 = CARTESIAN_POINT ( 'NONE',  ( -55.24340739397742084, 0.0007387096945740994529, -0.01010924026184336841 ) ) ;
#1593 = CARTESIAN_POINT ( 'NONE',  ( -1.463510566862833207, -25.15876608740840936, -38.76366072687767428 ) ) ;
#1594 = CARTESIAN_POINT ( 'NONE',  ( 109.1586059443104944, -0.001198897580748387297, -0.006971743774738781672 ) ) ;
#1595 = CARTESIAN_POINT ( 'NONE',  ( 25.64700659047696973, 0.2275682798802720064, -112.9110011064639565 ) ) ;
#1596 = ORIENTED_EDGE ( 'NONE', *, *, #11628, .T. ) ;
#1597 = CARTESIAN_POINT ( 'NONE',  ( 25.64703792032466012, -45.78915563622635432, 103.2099561461823214 ) ) ;
#1598 = CARTESIAN_POINT ( 'NONE',  ( -8.259864102781671491, -9.986657004933254811, 52.06232470801721490 ) ) ;
#1599 = ORIENTED_EDGE ( 'NONE', *, *, #21466, .F. ) ;
#1600 =( BOUNDED_SURFACE ( )  B_SPLINE_SURFACE ( 3, 1, ( 
 ( #22171, #2437 ),
 ( #14978, #6638 ),
 ( #28347, #6225 ),
 ( #1876, #15391 ) ),
 .UNSPECIFIED., .F., .F., .F. ) 
 B_SPLINE_SURFACE_WITH_KNOTS ( ( 4, 4 ),
 ( 2, 2 ),
 ( 0.000000000000000000, 1.000000000000000000 ),
 ( 0.000000000000000000, 1.000000000000000000 ),
 .UNSPECIFIED. ) 
 GEOMETRIC_REPRESENTATION_ITEM ( )  RATIONAL_B_SPLINE_SURFACE ( (
 ( 1.000000000000000000, 1.000000000000000000),
 ( 0.9934239774497838349, 0.8357310067453913582),
 ( 0.9934239774497838349, 0.8357310067453913582),
 ( 1.000000000000000000, 1.000000000000000000) ) ) 
 REPRESENTATION_ITEM ( '' )  SURFACE ( )  );
#1601 = VERTEX_POINT ( 'NONE', #1090 ) ;
#1602 = EDGE_CURVE ( 'NONE', #11658, #27831, #4011, .T. ) ;
#1603 = ORIENTED_EDGE ( 'NONE', *, *, #15318, .F. ) ;
#1604 = EDGE_CURVE ( 'NONE', #15835, #16671, #25426, .T. ) ;
#1605 = CARTESIAN_POINT ( 'NONE',  ( 1.833206308920109606, 29.44113170198547635, 142.0914675761164006 ) ) ;
#1606 = CARTESIAN_POINT ( 'NONE',  ( -20.20700224038492365, 10.08426345511628597, 27.82980252387807951 ) ) ;
#1607 = CARTESIAN_POINT ( 'NONE',  ( 10.93730112725932635, 0.000000000000000000, 0.000000000000000000 ) ) ;
#1608 = CARTESIAN_POINT ( 'NONE',  ( -1.031422197589711764, 12.69107518035563587, 44.01264471863832739 ) ) ;
#1609 = VERTEX_POINT ( 'NONE', #3105 ) ;
#1610 = CARTESIAN_POINT ( 'NONE',  ( 1.833603222531972277, -58.61467103263656497, -132.7445893798463601 ) ) ;
#1611 = DIRECTION ( 'NONE',  ( -1.000000000000000000, -0.000000000000000000, -0.000000000000000000 ) ) ;
#1612 = CARTESIAN_POINT ( 'NONE',  ( -1.323439229708139875, 46.01398008004444762, -2.317790194799894010 ) ) ;
#1613 = CARTESIAN_POINT ( 'NONE',  ( -16.86833981943423311, 19.19877306373907189, 39.83928801320569590 ) ) ;
#1614 = CARTESIAN_POINT ( 'NONE',  ( 1.833485406944043827, -141.8265699653865113, -30.69200235379080510 ) ) ;
#1615 = B_SPLINE_CURVE_WITH_KNOTS ( 'NONE', 3,
 ( #3684, #1108, #8036, #21095, #18951, #10336, #3269, #27435 ),
 .UNSPECIFIED., .F., .F.,
 ( 4, 2, 2, 4 ),
 ( 0.000000000000000000, 0.0002429592666046676800, 0.0004859185332093353600, 0.0009718370664186789598 ),
 .UNSPECIFIED. ) ;
#1616 = CARTESIAN_POINT ( 'NONE',  ( 1.832998868059858122, 73.01698022778532504, -125.4013017422223299 ) ) ;
#1617 = CARTESIAN_POINT ( 'NONE',  ( -55.24390624410018802, -0.007503127514277506058, -0.007245494385991484328 ) ) ;
#1618 = B_SPLINE_CURVE_WITH_KNOTS ( 'NONE', 3,
 ( #14954, #6472, #4306, #19282 ),
 .UNSPECIFIED., .F., .F.,
 ( 4, 4 ),
 ( 1.734723475976807094E-17, 0.008383560773332727686 ),
 .UNSPECIFIED. ) ;
#1619 = FACE_OUTER_BOUND ( 'NONE', #12979, .T. ) ;
#1620 = CARTESIAN_POINT ( 'NONE',  ( 109.1589550718174877, -0.0005685167901298913409, -0.007553890059312244956 ) ) ;
#1621 = CARTESIAN_POINT ( 'NONE',  ( 28.43349137099835744, -122.3147591366315510, -21.85613782299105878 ) ) ;
#1622 = VECTOR ( 'NONE', #7177, 1000.000000000000114 ) ;
#1623 = ORIENTED_EDGE ( 'NONE', *, *, #10544, .F. ) ;
#1624 = EDGE_CURVE ( 'NONE', #20099, #11885, #2254, .T. ) ;
#1625 = ORIENTED_EDGE ( 'NONE', *, *, #10400, .F. ) ;
#1626 = CARTESIAN_POINT ( 'NONE',  ( -6.574463467970653952, -51.07975593197902953, 5.014313797967556496 ) ) ;
#1628 = ORIENTED_EDGE ( 'NONE', *, *, #24073, .T. ) ;
#1627 = CARTESIAN_POINT ( 'NONE',  ( -1.045287976400365970, 45.76855895860943235, -1.530335034934267258 ) ) ;
#1629 = EDGE_LOOP ( 'NONE', ( #27024, #6614, #11939, #20985 ) ) ;
#1630 = ORIENTED_EDGE ( 'NONE', *, *, #16544, .T. ) ;
#1631 = ORIENTED_EDGE ( 'NONE', *, *, #28355, .T. ) ;
#1632 = EDGE_CURVE ( 'NONE', #13229, #18707, #8018, .T. ) ;
#1633 = EDGE_CURVE ( 'NONE', #21599, #9317, #25567, .T. ) ;
#1634 = FACE_OUTER_BOUND ( 'NONE', #4278, .T. ) ;
#1635 = LINE ( 'NONE', #26097, #10715 ) ;
#1636 = CARTESIAN_POINT ( 'NONE',  ( 32.73300124599737160, -117.5726003567929610, 3.836798148478423265 ) ) ;
#1637 = CARTESIAN_POINT ( 'NONE',  ( 28.37599760073042532, 55.80522390574119385, 100.2461467136612328 ) ) ;
#1638 = CARTESIAN_POINT ( 'NONE',  ( 25.69398547355839924, 102.8740393624600955, -46.61500694509545184 ) ) ;
#1639 = VERTEX_POINT ( 'NONE', #25837 ) ;
#1640 = EDGE_LOOP ( 'NONE', ( #17197, #15813, #14446, #14411 ) ) ;
#1642 = CARTESIAN_POINT ( 'NONE',  ( 32.73300124599735739, 32.68291970228236920, 113.0038235389603472 ) ) ;
#1641 = CARTESIAN_POINT ( 'NONE',  ( 1.832998868059890096, -29.64765804469973531, -142.0492247521725631 ) ) ;
#1643 = CARTESIAN_POINT ( 'NONE',  ( -21.81686047589429833, -6.867757412720954413, -37.90526371014254892 ) ) ;
#1644 =( NAMED_UNIT ( * ) SI_UNIT ( $, .STERADIAN. ) SOLID_ANGLE_UNIT ( ) );
#1645 = CARTESIAN_POINT ( 'NONE',  ( 25.86096068574580897, 112.5344699600050404, -10.82483750674488832 ) ) ;
#1646 = VERTEX_POINT ( 'NONE', #17185 ) ;
#1647 = CARTESIAN_POINT ( 'NONE',  ( 25.64708010899962787, 91.31497827399827827, -66.41183455464044982 ) ) ;
#1648 = EDGE_CURVE ( 'NONE', #10148, #21175, #1778, .T. ) ;
#1649 = CARTESIAN_POINT ( 'NONE',  ( -20.20700224038492721, -27.82980252387812570, 10.08426345511618649 ) ) ;
#1650 = CARTESIAN_POINT ( 'NONE',  ( -55.24271866751342941, -0.001425019990778747699, -0.009388511352200236415 ) ) ;
#1651 = ORIENTED_EDGE ( 'NONE', *, *, #11503, .F. ) ;
#1652 = ORIENTED_EDGE ( 'NONE', *, *, #17166, .F. ) ;
#1653 = ADVANCED_FACE ( 'NONE', ( #15015, #8421 ), #23548, .F. ) ;
#1654 = CARTESIAN_POINT ( 'NONE',  ( -1.058473599757826511, -38.06357893967446415, -25.48501014712384816 ) ) ;
#1655 = ORIENTED_EDGE ( 'NONE', *, *, #22704, .F. ) ;
#1656 = ORIENTED_EDGE ( 'NONE', *, *, #19589, .F. ) ;
#1657 = ADVANCED_FACE ( 'NONE', ( #14603 ), #1783, .F. ) ;
#1658 = CARTESIAN_POINT ( 'NONE',  ( 55.49584447822657296, -42.86099773636581034, 58.53775398922241635 ) ) ;
#1659 = ORIENTED_EDGE ( 'NONE', *, *, #13520, .T. ) ;
#1660 =( BOUNDED_SURFACE ( )  B_SPLINE_SURFACE ( 3, 1, ( 
 ( #1910, #10566 ),
 ( #15135, #8412 ),
 ( #4216, #14728 ),
 ( #21361, #12998 ) ),
 .UNSPECIFIED., .F., .F., .F. ) 
 B_SPLINE_SURFACE_WITH_KNOTS ( ( 4, 4 ),
 ( 2, 2 ),
 ( 0.000000000000000000, 1.000000000000000000 ),
 ( 0.000000000000000000, 1.000000000000000000 ),
 .UNSPECIFIED. ) 
 GEOMETRIC_REPRESENTATION_ITEM ( )  RATIONAL_B_SPLINE_SURFACE ( (
 ( 1.000000000000000000, 1.000000000000000000),
 ( 0.9956975270656955868, 0.8568959468854907557),
 ( 0.9956975270656955868, 0.8568959468854907557),
 ( 1.000000000000000000, 1.000000000000000000) ) ) 
 REPRESENTATION_ITEM ( '' )  SURFACE ( )  );
#1661 = CARTESIAN_POINT ( 'NONE',  ( -1.031422197589711987, 15.60268798220698727, 43.06660437151290211 ) ) ;
#1662 = CARTESIAN_POINT ( 'NONE',  ( 25.64681081121879203, 0.4157506337727869816, 112.9102952884414464 ) ) ;
#1663 = CARTESIAN_POINT ( 'NONE',  ( 1.833206310202337930, 138.2356391007182879, 44.13245377365679190 ) ) ;
#1664 = CARTESIAN_POINT ( 'NONE',  ( 109.1587776205901577, 0.006995903587858427232, -0.002185517590245281139 ) ) ;
#1665 = LINE ( 'NONE', #10752, #19759 ) ;
#1666 =( BOUNDED_SURFACE ( )  B_SPLINE_SURFACE ( 3, 1, ( 
 ( #19392, #8329 ),
 ( #22120, #26565 ),
 ( #239, #24289 ),
 ( #26021, #19806 ) ),
 .UNSPECIFIED., .F., .F., .F. ) 
 B_SPLINE_SURFACE_WITH_KNOTS ( ( 4, 4 ),
 ( 2, 2 ),
 ( 0.000000000000000000, 1.000000000000000000 ),
 ( 0.000000000000000000, 1.000000000000000000 ),
 .UNSPECIFIED. ) 
 GEOMETRIC_REPRESENTATION_ITEM ( )  RATIONAL_B_SPLINE_SURFACE ( (
 ( 1.000000000000000000, 1.000000000000000000),
 ( 0.7789835883360576307, 0.9689951854195403280),
 ( 0.7789835883360576307, 0.9689951854195403280),
 ( 1.000000000000000000, 1.000000000000000000) ) ) 
 REPRESENTATION_ITEM ( '' )  SURFACE ( )  );
#1667 = LINE ( 'NONE', #19231, #10299 ) ;
#1669 = CARTESIAN_POINT ( 'NONE',  ( 32.73300124599732186, 0.000000000000000000, 0.000000000000000000 ) ) ;
#1668 = FACE_OUTER_BOUND ( 'NONE', #27616, .T. ) ;
#1670 = CARTESIAN_POINT ( 'NONE',  ( -1.619063947482197729, 44.80407745103800465, 11.94059994246113021 ) ) ;
#1671 = ORIENTED_EDGE ( 'NONE', *, *, #23458, .F. ) ;
#1672 = VERTEX_POINT ( 'NONE', #1507 ) ;
#1673 = CARTESIAN_POINT ( 'NONE',  ( 2.433796855181233454, -46.34326152018648060, -137.9325382748289996 ) ) ;
#1674 = B_SPLINE_CURVE_WITH_KNOTS ( 'NONE', 3,
 ( #17267, #10528, #2009, #17404, #26057, #15099, #3761, #25929, #19160, #23917 ),
 .UNSPECIFIED., .F., .F.,
 ( 4, 3, 3, 4 ),
 ( 1.040834085586084257E-17, 0.0002669560319015720925, 0.0005492286108966365748, 0.0008315040496093422957 ),
 .UNSPECIFIED. ) ;
#1675 = CARTESIAN_POINT ( 'NONE',  ( 1.834118845439484335, -15.34511559672778347, 144.2964192726481372 ) ) ;
#1676 = DIRECTION ( 'NONE',  ( 1.000000000000000000, 0.000000000000000000, 0.000000000000000000 ) ) ;
#1677 = CARTESIAN_POINT ( 'NONE',  ( 32.73300124599735739, 55.46353551262010484, 103.7392577722178260 ) ) ;
#1678 = FACE_OUTER_BOUND ( 'NONE', #5902, .T. ) ;
#1679 = EDGE_LOOP ( 'NONE', ( #25564, #11319, #22717, #13689 ) ) ;
#1680 = CARTESIAN_POINT ( 'NONE',  ( -22.34422965417125440, -16.46028608106132651, -34.15536449444082479 ) ) ;
#1681 = CARTESIAN_POINT ( 'NONE',  ( 25.64681081121880624, -75.86069728268932977, -83.63051021305977883 ) ) ;
#1682 = ORIENTED_EDGE ( 'NONE', *, *, #26728, .F. ) ;
#1683 = CARTESIAN_POINT ( 'NONE',  ( -25.21435515916043713, 4.655591116594827383, 34.29329011225949841 ) ) ;
#1684 = CARTESIAN_POINT ( 'NONE',  ( 109.1586059443104944, -0.007001002073871752558, -0.001014167950280760828 ) ) ;
#1685 = PLANE ( 'NONE',  #21136 ) ;
#1686 = CARTESIAN_POINT ( 'NONE',  ( 25.64681081121879203, 107.2555980796241215, 35.28660243342585545 ) ) ;
#1687 = CARTESIAN_POINT ( 'NONE',  ( 2.433796855181233454, -107.1581411821792216, 98.43889364293823974 ) ) ;
#1688 = CARTESIAN_POINT ( 'NONE',  ( 25.64681081121879203, -91.59071981940525120, -66.03065707439029097 ) ) ;
#1689 = EDGE_CURVE ( 'NONE', #21619, #8934, #6086, .T. ) ;
#1690 = VERTEX_POINT ( 'NONE', #8148 ) ;
#1691 = B_SPLINE_CURVE_WITH_KNOTS ( 'NONE', 3,
 ( #26699, #8593, #19952, #6581, #17356, #15188, #9020, #24010 ),
 .UNSPECIFIED., .F., .F.,
 ( 4, 2, 2, 4 ),
 ( 0.000000000000000000, 0.0002429592666046731823, 0.0004859185332093463646, 0.0009718370664186793935 ),
 .UNSPECIFIED. ) ;
#1693 = CARTESIAN_POINT ( 'NONE',  ( 13.36082413113061307, 25.56125765253451831, 150.7747251079862849 ) ) ;
#1692 = B_SPLINE_CURVE_WITH_KNOTS ( 'NONE', 3,
 ( #11741, #26695, #24576, #4833, #7726, #1505, #12973, #12300 ),
 .UNSPECIFIED., .F., .F.,
 ( 4, 2, 2, 4 ),
 ( 2.237231151233565423E-16, 0.002761568181852865501, 0.005523136363705507222, 0.01104627272741080454 ),
 .UNSPECIFIED. ) ;
#1694 = ADVANCED_FACE ( 'NONE', ( #5984 ), #18525, .F. ) ;
#1695 = CARTESIAN_POINT ( 'NONE',  ( 10.93730112725996229, -10.89264110824889364, -150.7858122213663989 ) ) ;
#1696 = EDGE_CURVE ( 'NONE', #6748, #24062, #22902, .T. ) ;
#1697 = ORIENTED_EDGE ( 'NONE', *, *, #12105, .T. ) ;
#1698 = CARTESIAN_POINT ( 'NONE',  ( -55.25297051322618813, 0.01354497706059544504, -0.006313402748432239003 ) ) ;
#1699 = ORIENTED_EDGE ( 'NONE', *, *, #12262, .F. ) ;
#1700 = CARTESIAN_POINT ( 'NONE',  ( -25.21435515916043713, -4.655591116594118617, 34.29329011225960500 ) ) ;
#1701 = CARTESIAN_POINT ( 'NONE',  ( -1.619063947482197729, -11.94059994246129008, 44.80407745103795492 ) ) ;
#1702 = CARTESIAN_POINT ( 'NONE',  ( 1.832998868059890096, 30.69214149074206688, -141.8272129421605712 ) ) ;
#1703 = CARTESIAN_POINT ( 'NONE',  ( -1.044556982611274831, 36.05793013899099719, -28.22896456560681600 ) ) ;
#1704 = CARTESIAN_POINT ( 'NONE',  ( 2.433796855181219243, 28.83182736670734059, -142.6247129145645829 ) ) ;
#1705 = CARTESIAN_POINT ( 'NONE',  ( -4.473127245936431073, 41.70021447285055416, -26.34600523034553277 ) ) ;
#1706 = CARTESIAN_POINT ( 'NONE',  ( 25.64681081121879203, 75.24277141833607629, -84.18689316039970549 ) ) ;
#1707 = CARTESIAN_POINT ( 'NONE',  ( 10.93730112725991077, -79.81734490845832397, -128.3908183996600201 ) ) ;
#1708 = CARTESIAN_POINT ( 'NONE',  ( 109.1592201516379674, -0.007566779963325582538, -0.002134489919768117836 ) ) ;
#1709 = CARTESIAN_POINT ( 'NONE',  ( 109.1624594426973118, -0.01531968460306872698, -0.004489871836309295566 ) ) ;
#1710 = CARTESIAN_POINT ( 'NONE',  ( -1.539760825549688850, 29.16712717142812039, 35.94320866319458219 ) ) ;
#1711 = ORIENTED_EDGE ( 'NONE', *, *, #10237, .F. ) ;
#1712 =( BOUNDED_SURFACE ( )  B_SPLINE_SURFACE ( 3, 1, ( 
 ( #8468, #17503 ),
 ( #19664, #19956 ),
 ( #24147, #4548 ),
 ( #21973, #3991 ) ),
 .UNSPECIFIED., .F., .F., .F. ) 
 B_SPLINE_SURFACE_WITH_KNOTS ( ( 4, 4 ),
 ( 2, 2 ),
 ( 0.000000000000000000, 1.000000000000000000 ),
 ( 0.000000000000000000, 1.000000000000000000 ),
 .UNSPECIFIED. ) 
 GEOMETRIC_REPRESENTATION_ITEM ( )  RATIONAL_B_SPLINE_SURFACE ( (
 ( 1.000000000000000000, 1.000000000000000000),
 ( 0.9934239774497838349, 0.8357310067453913582),
 ( 0.9934239774497838349, 0.8357310067453913582),
 ( 1.000000000000000000, 1.000000000000000000) ) ) 
 REPRESENTATION_ITEM ( '' )  SURFACE ( )  );
#1713 = ORIENTED_EDGE ( 'NONE', *, *, #16291, .F. ) ;
#1714 = ORIENTED_EDGE ( 'NONE', *, *, #16181, .T. ) ;
#1715 = DIRECTION ( 'NONE',  ( 0.5946245182733608248, -0.5994612328333251972, 0.5357871896547391488 ) ) ;
#1716 = CARTESIAN_POINT ( 'NONE',  ( 2.063896406836609909, 144.6078654718901646, 13.84738934186238524 ) ) ;
#1717 = CARTESIAN_POINT ( 'NONE',  ( 1.894214914920977266, -97.83100278581332532, -107.2270864706600122 ) ) ;
#1718 = CARTESIAN_POINT ( 'NONE',  ( -1.619063947482201282, 43.26576862488434472, -16.67502769180576649 ) ) ;
#1719 = CARTESIAN_POINT ( 'NONE',  ( 28.37603512858447630, -84.05169593519779880, 78.09501335733563110 ) ) ;
#1720 = DIRECTION ( 'NONE',  ( 0.5914120900931444380, -0.7333565075147354673, -0.3352908775637181149 ) ) ;
#1721 = ORIENTED_EDGE ( 'NONE', *, *, #6154, .T. ) ;
#1722 = CARTESIAN_POINT ( 'NONE',  ( 32.73300124599739291, 89.94078864464164269, -75.82012867748392182 ) ) ;
#1723 = CARTESIAN_POINT ( 'NONE',  ( -55.24390624410018802, 0.001811362924362862900, -0.01027195578988028025 ) ) ;
#1724 = CARTESIAN_POINT ( 'NONE',  ( 1.833838850093452599, 117.3962623502786187, -85.29338149487099940 ) ) ;
#1725 = B_SPLINE_CURVE_WITH_KNOTS ( 'NONE', 3,
 ( #7037, #2842, #24879, #15795, #27150, #5141 ),
 .UNSPECIFIED., .F., .F.,
 ( 4, 2, 4 ),
 ( 0.000000000000000000, 0.003570751334075635691, 0.007141502668151271382 ),
 .UNSPECIFIED. ) ;
#1726 = EDGE_CURVE ( 'NONE', #15408, #20144, #16349, .T. ) ;
#1727 = DIRECTION ( 'NONE',  ( -0.5946245182733607137, -0.1700465163848142724, -0.7858154137795737570 ) ) ;
#1728 = B_SPLINE_CURVE_WITH_KNOTS ( 'NONE', 3,
 ( #11036, #4406, #9021, #15472, #26287, #21834, #2231, #19798, #22264, #17911 ),
 .UNSPECIFIED., .F., .F.,
 ( 4, 3, 3, 4 ),
 ( 6.938893903907228378E-18, 0.0002669560319015785977, 0.0005492286108966380927, 0.0008315040496093435967 ),
 .UNSPECIFIED. ) ;
#1729 = ORIENTED_EDGE ( 'NONE', *, *, #10485, .F. ) ;
#1730 = CARTESIAN_POINT ( 'NONE',  ( -7.733045908741324581, 35.49239760110675945, -38.67583825854160295 ) ) ;
#1731 = EDGE_CURVE ( 'NONE', #11830, #18479, #26633, .T. ) ;
#1732 = CARTESIAN_POINT ( 'NONE',  ( 25.64660436782539676, -97.49251393956821232, 56.95711784271951217 ) ) ;
#1733 = ORIENTED_EDGE ( 'NONE', *, *, #7695, .T. ) ;
#1734 = EDGE_LOOP ( 'NONE', ( #20934, #15080, #4778, #23923 ) ) ;
#1735 = ORIENTED_EDGE ( 'NONE', *, *, #27850, .T. ) ;
#1736 = CARTESIAN_POINT ( 'NONE',  ( 25.64708010899964918, -110.4552579818683853, -23.42206246795119995 ) ) ;
#1737 = CARTESIAN_POINT ( 'NONE',  ( 24.01988960052042898, -103.4492499592080463, -80.44223964539959582 ) ) ;
#1738 = CARTESIAN_POINT ( 'NONE',  ( 1.833838848569416591, 29.99593366454950782, -141.9757689770218860 ) ) ;
#1739 = B_SPLINE_CURVE_WITH_KNOTS ( 'NONE', 3,
 ( #25007, #26980, #22552, #22703, #14316, #20941 ),
 .UNSPECIFIED., .F., .F.,
 ( 4, 2, 4 ),
 ( 4.653458371169123007E-16, 0.003576372551511270217, 0.007152745103022075529 ),
 .UNSPECIFIED. ) ;
#1740 = CARTESIAN_POINT ( 'NONE',  ( 32.73300124599734318, 99.90245962373836619, 62.10906484417276374 ) ) ;
#1741 = ORIENTED_EDGE ( 'NONE', *, *, #23367, .T. ) ;
#1742 = CARTESIAN_POINT ( 'NONE',  ( -55.24390624410018802, -0.01027195578987978239, -0.001811362924362686826 ) ) ;
#1743 = FACE_OUTER_BOUND ( 'NONE', #27486, .T. ) ;
#1744 = CARTESIAN_POINT ( 'NONE',  ( 1.833485406944043827, 84.86072343962726450, -117.7091014914941809 ) ) ;
#1745 = EDGE_CURVE ( 'NONE', #15398, #12444, #11416, .T. ) ;
#1746 = CARTESIAN_POINT ( 'NONE',  ( -1.048172774974279076, 45.78636862970795107, -1.020161070261278224 ) ) ;
#1747 = CARTESIAN_POINT ( 'NONE',  ( 1.833691583653536572, 97.36155720551622039, -107.5990239011816527 ) ) ;
#1748 = CARTESIAN_POINT ( 'NONE',  ( 6.224689322667647851, 84.93872395423136368, -121.2721959030529462 ) ) ;
#1749 = EDGE_CURVE ( 'NONE', #14867, #6575, #24262, .T. ) ;
#1750 = ADVANCED_FACE ( 'NONE', ( #11138 ), #7711, .F. ) ;
#1751 = CARTESIAN_POINT ( 'NONE',  ( -1.045287976400362417, 25.66401692419989899, -37.92705037016767733 ) ) ;
#1752 = CARTESIAN_POINT ( 'NONE',  ( -40.00000000000000000, 0.000000000000000000, -37.50000000000002132 ) ) ;
#1753 =( BOUNDED_SURFACE ( )  B_SPLINE_SURFACE ( 3, 1, ( 
 ( #11437, #14806 ),
 ( #26030, #6321 ),
 ( #497, #12644 ),
 ( #12915, #1702 ) ),
 .UNSPECIFIED., .F., .F., .F. ) 
 B_SPLINE_SURFACE_WITH_KNOTS ( ( 4, 4 ),
 ( 2, 2 ),
 ( 0.000000000000000000, 1.000000000000000000 ),
 ( 0.000000000000000000, 1.000000000000000000 ),
 .UNSPECIFIED. ) 
 GEOMETRIC_REPRESENTATION_ITEM ( )  RATIONAL_B_SPLINE_SURFACE ( (
 ( 1.000000000000000000, 1.000000000000000000),
 ( 0.9960225298536222738, 0.9999952330161893110),
 ( 0.9960225298536222738, 0.9999952330161893110),
 ( 1.000000000000000000, 1.000000000000000000) ) ) 
 REPRESENTATION_ITEM ( '' )  SURFACE ( )  );
#1754 = ORIENTED_EDGE ( 'NONE', *, *, #19850, .T. ) ;
#1755 = VECTOR ( 'NONE', #27643, 1000.000000000000114 ) ;
#1756 = ORIENTED_EDGE ( 'NONE', *, *, #11864, .T. ) ;
#1757 = CARTESIAN_POINT ( 'NONE',  ( 25.81918753295377300, -24.41190151229177729, -110.3582118788979756 ) ) ;
#1758 = ORIENTED_EDGE ( 'NONE', *, *, #17002, .T. ) ;
#1759 = EDGE_LOOP ( 'NONE', ( #21545, #6302, #17364, #18495 ) ) ;
#1760 = ORIENTED_EDGE ( 'NONE', *, *, #24696, .F. ) ;
#1761 = ORIENTED_EDGE ( 'NONE', *, *, #25590, .T. ) ;
#1762 = CARTESIAN_POINT ( 'NONE',  ( -20.57838717382308147, -7.715628353033481268, 28.96176188950225949 ) ) ;
#1763 = CARTESIAN_POINT ( 'NONE',  ( -1.619063947482197729, -43.26576862488421682, 16.67502769180607203 ) ) ;
#1764 = CARTESIAN_POINT ( 'NONE',  ( 1.833206308920072081, -73.19872517709806914, 125.2945011813203848 ) ) ;
#1765 = B_SPLINE_CURVE_WITH_KNOTS ( 'NONE', 3,
 ( #5159, #18243, #9625, #18388, #1135, #5597 ),
 .UNSPECIFIED., .F., .F.,
 ( 4, 2, 4 ),
 ( 3.469446951953613804E-18, 0.0004335184443139973023, 0.0008670368886279911352 ),
 .UNSPECIFIED. ) ;
#1766 = CARTESIAN_POINT ( 'NONE',  ( 10.93730112726003156, 108.9902118373755684, -104.7670965581001781 ) ) ;
#1767 = EDGE_CURVE ( 'NONE', #9334, #7451, #20526, .T. ) ;
#1768 = CARTESIAN_POINT ( 'NONE',  ( 32.73300124599738581, 75.82012867748602503, -89.94078864463983791 ) ) ;
#1769 = CARTESIAN_POINT ( 'NONE',  ( 30.59138290137884653, -66.10404757334126202, 95.58039132682505112 ) ) ;
#1770 = ADVANCED_FACE ( 'NONE', ( #22513 ), #16698, .F. ) ;
#1771 = CARTESIAN_POINT ( 'NONE',  ( 26.04756280548354042, 102.9366382251199497, -47.04636360340725076 ) ) ;
#1772 = FACE_OUTER_BOUND ( 'NONE', #15985, .T. ) ;
#1773 = CARTESIAN_POINT ( 'NONE',  ( 1.833485406944085350, 132.3460930279899515, -59.50871042846091541 ) ) ;
#1774 = EDGE_CURVE ( 'NONE', #20441, #17039, #8864, .T. ) ;
#1775 = ORIENTED_EDGE ( 'NONE', *, *, #12128, .F. ) ;
#1776 = ORIENTED_EDGE ( 'NONE', *, *, #14718, .T. ) ;
#1778 = LINE ( 'NONE', #18934, #2677 ) ;
#1777 = CARTESIAN_POINT ( 'NONE',  ( -2.911734481061364566, -40.13920818157090054, -25.69892591260251535 ) ) ;
#1779 = CARTESIAN_POINT ( 'NONE',  ( -55.24728320129491266, 0.009072670231978626973, -0.01137345571547102377 ) ) ;
#1780 = CARTESIAN_POINT ( 'NONE',  ( 25.64681081121880624, -112.2483031020014295, 12.21581276189770904 ) ) ;
#1781 = CARTESIAN_POINT ( 'NONE',  ( -20.20612092514784308, -16.46550332780508796, 24.59769888281551786 ) ) ;
#1782 = ORIENTED_EDGE ( 'NONE', *, *, #5338, .F. ) ;
#1783 =( BOUNDED_SURFACE ( )  B_SPLINE_SURFACE ( 3, 1, ( 
 ( #27852, #14743 ),
 ( #21229, #23406 ),
 ( #23699, #8277 ),
 ( #6263, #10444 ) ),
 .UNSPECIFIED., .F., .F., .F. ) 
 B_SPLINE_SURFACE_WITH_KNOTS ( ( 4, 4 ),
 ( 2, 2 ),
 ( 0.000000000000000000, 1.000000000000000000 ),
 ( 0.000000000000000000, 1.000000000000000000 ),
 .UNSPECIFIED. ) 
 GEOMETRIC_REPRESENTATION_ITEM ( )  RATIONAL_B_SPLINE_SURFACE ( (
 ( 1.000000000000000000, 1.000000000000000000),
 ( 0.6386103224230316178, 0.9954351624131538845),
 ( 0.6386103224230316178, 0.9954351624131538845),
 ( 1.000000000000000000, 1.000000000000000000) ) ) 
 REPRESENTATION_ITEM ( '' )  SURFACE ( )  );
#1784 = B_SPLINE_CURVE_WITH_KNOTS ( 'NONE', 3,
 ( #16588, #756, #5660, #14423, #23232, #3483, #21035 ),
 .UNSPECIFIED., .F., .F.,
 ( 4, 3, 4 ),
 ( 0.000000000000000000, 0.006568092053401769319, 0.02506242213020846987 ),
 .UNSPECIFIED. ) ;
#1785 = CARTESIAN_POINT ( 'NONE',  ( -25.21435515916043713, 6.169479169075932745, 34.05351380035326514 ) ) ;
#1786 = CARTESIAN_POINT ( 'NONE',  ( -55.24271866751342941, 0.001425019990779439203, 0.009388511352200054269 ) ) ;
#1787 = ORIENTED_EDGE ( 'NONE', *, *, #8404, .F. ) ;
#1788 = VERTEX_POINT ( 'NONE', #4371 ) ;
#1789 = CARTESIAN_POINT ( 'NONE',  ( 8.186469777910904355, -131.0413692044507172, -71.65198614410340383 ) ) ;
#1790 = ORIENTED_EDGE ( 'NONE', *, *, #15453, .F. ) ;
#1791 = ORIENTED_EDGE ( 'NONE', *, *, #18888, .F. ) ;
#1792 = CARTESIAN_POINT ( 'NONE',  ( 32.73300124599739291, 92.86301839380121237, -72.21147546950456331 ) ) ;
#1793 = ORIENTED_EDGE ( 'NONE', *, *, #5865, .T. ) ;
#1794 = CARTESIAN_POINT ( 'NONE',  ( 32.73300124599734318, 114.2056417606548706, 28.19767303745648945 ) ) ;
#1795 = CARTESIAN_POINT ( 'NONE',  ( 13.84597867724971287, -90.05293531772709059, 115.8103190066270258 ) ) ;
#1796 = ADVANCED_FACE ( 'NONE', ( #13144 ), #20366, .F. ) ;
#1797 = FACE_OUTER_BOUND ( 'NONE', #5905, .T. ) ;
#1798 = CARTESIAN_POINT ( 'NONE',  ( -1.583189561560255143, 46.33203782964461936, 2.490696082060026573 ) ) ;
#1799 = CARTESIAN_POINT ( 'NONE',  ( 109.1624594426973118, -0.004489871836309242657, 0.01531968460306874259 ) ) ;
#1800 = CARTESIAN_POINT ( 'NONE',  ( 28.37599760073042532, -111.8383885143453256, -25.60640155549280550 ) ) ;
#1801 = EDGE_CURVE ( 'NONE', #211, #8086, #12986, .T. ) ;
#1802 = B_SPLINE_CURVE_WITH_KNOTS ( 'NONE', 3,
 ( #12381, #16568, #5636, #14404, #10104, #8097 ),
 .UNSPECIFIED., .F., .F.,
 ( 4, 2, 4 ),
 ( 4.906538933386797396E-18, 0.0004335151646191519543, 0.0008670303292382989212 ),
 .UNSPECIFIED. ) ;
#1803 = CARTESIAN_POINT ( 'NONE',  ( -20.20700224038492010, 8.199606986804733211, 28.44216453106527709 ) ) ;
#1804 = CARTESIAN_POINT ( 'NONE',  ( -20.24399999263416561, 24.70869149526203401, -16.36687688782867411 ) ) ;
#1805 = CARTESIAN_POINT ( 'NONE',  ( 25.65782528836479770, -102.9197507294672818, -46.45532072021288172 ) ) ;
#1806 = EDGE_CURVE ( 'NONE', #4100, #22982, #26685, .T. ) ;
#1807 = VERTEX_POINT ( 'NONE', #2779 ) ;
#1808 = ORIENTED_EDGE ( 'NONE', *, *, #2764, .F. ) ;
#1809 = CARTESIAN_POINT ( 'NONE',  ( 2.433796855181219243, -137.9325382748288291, 46.34326152018696376 ) ) ;
#1810 = CARTESIAN_POINT ( 'NONE',  ( -1.539763995773685945, 25.17088606276602647, 38.84665165401036546 ) ) ;
#1812 = CARTESIAN_POINT ( 'NONE',  ( 1.833485406944043827, 45.34878176254236593, 137.8414413349087511 ) ) ;
#1811 = LINE ( 'NONE', #23439, #11618 ) ;
#1813 = CARTESIAN_POINT ( 'NONE',  ( -1.045287976400383290, -44.00138577190632816, 12.68782741917368106 ) ) ;
#1814 = CARTESIAN_POINT ( 'NONE',  ( 9.884929003653626367, 78.87917189084909353, 128.2151425008044328 ) ) ;
#1815 = CARTESIAN_POINT ( 'NONE',  ( 55.79472521941428198, -37.00555938668216527, -62.63970324008300139 ) ) ;
#1816 = EDGE_CURVE ( 'NONE', #6924, #23596, #26389, .T. ) ;
#1817 = ORIENTED_EDGE ( 'NONE', *, *, #25192, .F. ) ;
#1818 = CARTESIAN_POINT ( 'NONE',  ( 25.64692232868535982, -112.2580042965358160, 12.12735788170774320 ) ) ;
#1819 = CARTESIAN_POINT ( 'NONE',  ( -1.019300379054419947, -38.21680004809145714, 25.26451264419685572 ) ) ;
#1820 = DIRECTION ( 'NONE',  ( 0.000000000000000000, 0.000000000000000000, 1.000000000000000000 ) ) ;
#1821 = CARTESIAN_POINT ( 'NONE',  ( 1.833603222531973387, 117.1340888386549750, 85.65285110156177950 ) ) ;
#1822 = ORIENTED_EDGE ( 'NONE', *, *, #19278, .T. ) ;
#1823 = CARTESIAN_POINT ( 'NONE',  ( 32.73300124599735739, -28.19767303745682341, 114.2056417606547285 ) ) ;
#1824 =( BOUNDED_SURFACE ( )  B_SPLINE_SURFACE ( 3, 1, ( 
 ( #19112, #23304 ),
 ( #27750, #12754 ),
 ( #28013, #21686 ),
 ( #3702, #14500 ) ),
 .UNSPECIFIED., .F., .F., .F. ) 
 B_SPLINE_SURFACE_WITH_KNOTS ( ( 4, 4 ),
 ( 2, 2 ),
 ( 0.000000000000000000, 1.000000000000000000 ),
 ( 0.000000000000000000, 1.000000000000000000 ),
 .UNSPECIFIED. ) 
 GEOMETRIC_REPRESENTATION_ITEM ( )  RATIONAL_B_SPLINE_SURFACE ( (
 ( 1.000000000000000000, 1.000000000000000000),
 ( 0.9956975270656954757, 0.8568959468854893125),
 ( 0.9956975270656954757, 0.8568959468854893125),
 ( 1.000000000000000000, 1.000000000000000000) ) ) 
 REPRESENTATION_ITEM ( '' )  SURFACE ( )  );
#1825 = CARTESIAN_POINT ( 'NONE',  ( 6.224689322667630975, -148.0369967195762513, -2.565137105445306709 ) ) ;
#1826 = CIRCLE ( 'NONE', #4605, 53.53553390275978785 ) ;
#1827 = ORIENTED_EDGE ( 'NONE', *, *, #3412, .F. ) ;
#1828 = DIRECTION ( 'NONE',  ( 0.000000000000000000, -1.000000000000000000, 0.000000000000000000 ) ) ;
#1829 = ORIENTED_EDGE ( 'NONE', *, *, #16621, .F. ) ;
#1830 = B_SPLINE_CURVE_WITH_KNOTS ( 'NONE', 3,
 ( #3651, #21635, #25696, #10712, #4073, #6386 ),
 .UNSPECIFIED., .F., .F.,
 ( 4, 2, 4 ),
 ( 1.734723475976807094E-18, 0.0004335184443140231605, 0.0008670368886280445863 ),
 .UNSPECIFIED. ) ;
#1831 = CARTESIAN_POINT ( 'NONE',  ( 26.11404676487257603, 92.25884714080409310, 65.63269960453273200 ) ) ;
#1832 = DIRECTION ( 'NONE',  ( -1.000000000000000000, -0.000000000000000000, -0.000000000000000000 ) ) ;
#1833 = CARTESIAN_POINT ( 'NONE',  ( 2.433796855181219243, -116.8607839509062671, 86.69855925933937613 ) ) ;
#1834 =( BOUNDED_SURFACE ( )  B_SPLINE_SURFACE ( 3, 1, ( 
 ( #4226, #10724 ),
 ( #1920, #22071 ),
 ( #13009, #11282 ),
 ( #15017, #24392 ) ),
 .UNSPECIFIED., .F., .F., .F. ) 
 B_SPLINE_SURFACE_WITH_KNOTS ( ( 4, 4 ),
 ( 2, 2 ),
 ( 0.000000000000000000, 1.000000000000000000 ),
 ( 0.000000000000000000, 1.000000000000000000 ),
 .UNSPECIFIED. ) 
 GEOMETRIC_REPRESENTATION_ITEM ( )  RATIONAL_B_SPLINE_SURFACE ( (
 ( 1.000000000000000000, 1.000000000000000000),
 ( 0.6386103224230302855, 0.9954351624131538845),
 ( 0.6386103224230302855, 0.9954351624131538845),
 ( 1.000000000000000000, 1.000000000000000000) ) ) 
 REPRESENTATION_ITEM ( '' )  SURFACE ( )  );
#1835 = CARTESIAN_POINT ( 'NONE',  ( -1.050229599974481065, 36.90196321294333615, 27.12684363859215608 ) ) ;
#1836 = LINE ( 'NONE', #8344, #47 ) ;
#1837 = FACE_OUTER_BOUND ( 'NONE', #20975, .T. ) ;
#1838 = DIRECTION ( 'NONE',  ( 0.000000000000000000, 5.223019709707975211E-21, -1.000000000000000000 ) ) ;
#1839 = DIRECTION ( 'NONE',  ( 0.000000000000000000, 0.000000000000000000, 1.000000000000000000 ) ) ;
#1840 = EDGE_CURVE ( 'NONE', #7314, #2342, #25244, .T. ) ;
#1841 = CARTESIAN_POINT ( 'NONE',  ( 1.831572820252009626, 45.77972211429817406, 137.7011124121618764 ) ) ;
#1842 = CARTESIAN_POINT ( 'NONE',  ( -8.786685647604890903, -25.35688121747466184, 47.14957014837381166 ) ) ;
#1843 = CARTESIAN_POINT ( 'NONE',  ( 25.81918753295378011, -46.82320532096449739, -102.8711004511197729 ) ) ;
#1844 = CARTESIAN_POINT ( 'NONE',  ( -20.20700224038492721, -10.08426345511609235, -27.82980252387815767 ) ) ;
#1845 = ORIENTED_EDGE ( 'NONE', *, *, #19157, .F. ) ;
#1846 = EDGE_CURVE ( 'NONE', #12851, #15769, #22664, .T. ) ;
#1847 = AXIS2_PLACEMENT_3D ( 'NONE', #23932, #8656, #24077 ) ;
#1848 = ORIENTED_EDGE ( 'NONE', *, *, #16071, .T. ) ;
#1849 = AXIS2_PLACEMENT_3D ( 'NONE', #14685, #5485, #12524 ) ;
#1850 = CARTESIAN_POINT ( 'NONE',  ( -1.044556982611267948, -43.01635920718339179, 15.70482750345280820 ) ) ;
#1851 = CARTESIAN_POINT ( 'NONE',  ( 16.05277956358205316, -128.9466020665978760, 62.52511797226075174 ) ) ;
#1852 = CARTESIAN_POINT ( 'NONE',  ( 109.1592201516379674, 0.003476928926134712113, 0.007051465909552774060 ) ) ;
#1853 = AXIS2_PLACEMENT_3D ( 'NONE', #18213, #7302, #16351 ) ;
#1854 = CARTESIAN_POINT ( 'NONE',  ( -20.57838717382308502, 27.96569011373086866, -10.78122205917010135 ) ) ;
#1855 = CARTESIAN_POINT ( 'NONE',  ( -55.24340739397742794, 0.009842732675349290250, 0.002421372372456403153 ) ) ;
#1856 = CARTESIAN_POINT ( 'NONE',  ( 28.37644542392831681, 65.64862111872214712, -105.5967537682337394 ) ) ;
#1857 = CARTESIAN_POINT ( 'NONE',  ( -55.24390624410018802, 0.004572280736702236288, 0.009374879212970765180 ) ) ;
#1858 = ORIENTED_EDGE ( 'NONE', *, *, #9631, .F. ) ;
#1859 = CARTESIAN_POINT ( 'NONE',  ( 10.93730112725969938, 56.95489579269752767, 140.0398180619111770 ) ) ;
#1860 = CARTESIAN_POINT ( 'NONE',  ( -1.056502255334264895, -13.66916755949820583, 43.72121397317236102 ) ) ;
#1861 = VECTOR ( 'NONE', #11403, 1000.000000000000114 ) ;
#1862 = CARTESIAN_POINT ( 'NONE',  ( -1.048996300304505747, -37.49570739463903379, -26.29666317565288480 ) ) ;
#1863 = B_SPLINE_CURVE_WITH_KNOTS ( 'NONE', 3,
 ( #471, #5221, #27080, #13419, #17871, #13564, #7255 ),
 .UNSPECIFIED., .F., .F.,
 ( 4, 3, 4 ),
 ( 1.430489624538199204E-17, 0.009512539173626433087, 0.02506242213020844906 ),
 .UNSPECIFIED. ) ;
#1864 = CARTESIAN_POINT ( 'NONE',  ( 119.2224693531408803, -90.00000000000005684, -20.00000000000001066 ) ) ;
#1865 = ORIENTED_EDGE ( 'NONE', *, *, #6707, .F. ) ;
#1866 = CARTESIAN_POINT ( 'NONE',  ( -4.780792508754315051, -37.74278713234418348, -32.07473752860764904 ) ) ;
#1867 = CARTESIAN_POINT ( 'NONE',  ( 25.64681081121879203, 112.2483031020015147, -12.21581276189692211 ) ) ;
#1868 = VERTEX_POINT ( 'NONE', #9991 ) ;
#1869 = B_SPLINE_CURVE_WITH_KNOTS ( 'NONE', 3,
 ( #1021, #1168, #27201, #9816, #18582, #21013, #25510, #16562 ),
 .UNSPECIFIED., .F., .F.,
 ( 4, 2, 2, 4 ),
 ( 2.223105199230524488E-16, 0.002761568181852866802, 0.005523136363705516763, 0.01104627272741080628 ),
 .UNSPECIFIED. ) ;
#1870 = ORIENTED_EDGE ( 'NONE', *, *, #23849, .T. ) ;
#1871 = ORIENTED_EDGE ( 'NONE', *, *, #18220, .F. ) ;
#1872 = VECTOR ( 'NONE', #11255, 1000.000000000000114 ) ;
#1873 = B_SPLINE_CURVE_WITH_KNOTS ( 'NONE', 3,
 ( #1722, #14401, #23212, #8095, #16864, #3752, #4029 ),
 .UNSPECIFIED., .F., .F.,
 ( 4, 3, 4 ),
 ( 0.000000000000000000, 0.02398743853561338332, 0.04000277880656218782 ),
 .UNSPECIFIED. ) ;
#1874 = CIRCLE ( 'NONE', #17479, 151.1787379149930359 ) ;
#1875 = CARTESIAN_POINT ( 'NONE',  ( 55.49584447822657296, -22.67407039687288872, 68.91748907713581218 ) ) ;
#1876 = CARTESIAN_POINT ( 'NONE',  ( -55.24390624410018802, -0.01032895241566962087, 0.001451500391950532459 ) ) ;
#1878 = AXIS2_PLACEMENT_3D ( 'NONE', #6192, #15353, #12916 ) ;
#1877 =( BOUNDED_SURFACE ( )  B_SPLINE_SURFACE ( 3, 1, ( 
 ( #28336, #26187 ),
 ( #6480, #4312 ),
 ( #24184, #21875 ),
 ( #2269, #2131 ) ),
 .UNSPECIFIED., .F., .F., .F. ) 
 B_SPLINE_SURFACE_WITH_KNOTS ( ( 4, 4 ),
 ( 2, 2 ),
 ( 0.000000000000000000, 1.000000000000000000 ),
 ( 0.000000000000000000, 1.000000000000000000 ),
 .UNSPECIFIED. ) 
 GEOMETRIC_REPRESENTATION_ITEM ( )  RATIONAL_B_SPLINE_SURFACE ( (
 ( 1.000000000000000000, 1.000000000000000000),
 ( 0.6386103224230302855, 0.9954351624131538845),
 ( 0.6386103224230302855, 0.9954351624131538845),
 ( 1.000000000000000000, 1.000000000000000000) ) ) 
 REPRESENTATION_ITEM ( '' )  SURFACE ( )  );
#1879 = CARTESIAN_POINT ( 'NONE',  ( -1.031422197589716205, -36.13727897780147202, -28.14735071801731792 ) ) ;
#1880 = ADVANCED_FACE ( 'NONE', ( #3209 ), #15745, .F. ) ;
#1881 = CARTESIAN_POINT ( 'NONE',  ( 32.73300124599738581, 75.82012867748602503, -89.94078864463983791 ) ) ;
#1882 = ORIENTED_EDGE ( 'NONE', *, *, #17781, .F. ) ;
#1883 = EDGE_CURVE ( 'NONE', #20968, #8074, #1320, .T. ) ;
#1884 = CARTESIAN_POINT ( 'NONE',  ( 1.833750490713743853, 59.26520711750040249, -132.4555075118561547 ) ) ;
#1885 = EDGE_CURVE ( 'NONE', #10927, #1116, #8216, .T. ) ;
#1886 = CARTESIAN_POINT ( 'NONE',  ( 25.64692872815573921, 56.17679456083801881, 97.94438212068848770 ) ) ;
#1887 = CARTESIAN_POINT ( 'NONE',  ( 1.893872463202044054, -138.3372034345894690, 43.94661640105973532 ) ) ;
#1888 = CARTESIAN_POINT ( 'NONE',  ( -20.57838717382308147, -29.92853265176830746, 1.611677988432673070 ) ) ;
#1889 = VECTOR ( 'NONE', #17665, 1000.000000000000000 ) ;
#1890 = CIRCLE ( 'NONE', #9712, 151.1787379149930359 ) ;
#1891 = CARTESIAN_POINT ( 'NONE',  ( -1.619063947482197729, -16.67502769180532596, 43.26576862488450104 ) ) ;
#1892 = CARTESIAN_POINT ( 'NONE',  ( 55.49584447822657296, -22.67407039687194015, -68.91748907713612482 ) ) ;
#1893 = B_SPLINE_CURVE_WITH_KNOTS ( 'NONE', 3,
 ( #6727, #21551, #10902, #6866, #4409, #26562, #6588, #19389, #8735, #15473 ),
 .UNSPECIFIED., .F., .F.,
 ( 4, 3, 3, 4 ),
 ( 1.040834085586084257E-17, 0.0002669560319015743151, 0.0005492286108966349485, 0.0008315040496093406694 ),
 .UNSPECIFIED. ) ;
#1894 = CARTESIAN_POINT ( 'NONE',  ( 2.063896406836609909, 73.79559738457753326, 125.1295119249441683 ) ) ;
#1895 = CARTESIAN_POINT ( 'NONE',  ( 109.1592201516379674, -0.002913740842103232798, 0.007302213399787543455 ) ) ;
#1896 = VERTEX_POINT ( 'NONE', #18613 ) ;
#1897 = AXIS2_PLACEMENT_3D ( 'NONE', #14466, #3955, #10029 ) ;
#1898 = VERTEX_POINT ( 'NONE', #7548 ) ;
#1899 = CARTESIAN_POINT ( 'NONE',  ( -1.045287976400365970, 15.59869763335156101, 43.05558670614217931 ) ) ;
#1900 = CARTESIAN_POINT ( 'NONE',  ( -1.050230346682680560, 45.79907861045643358, 0.0006945978177289460027 ) ) ;
#1901 = VERTEX_POINT ( 'NONE', #27383 ) ;
#1902 = ADVANCED_FACE ( 'NONE', ( #628 ), #21467, .F. ) ;
#1903 = EDGE_LOOP ( 'NONE', ( #25085, #10046, #18799, #3743 ) ) ;
#1904 = EDGE_LOOP ( 'NONE', ( #15098, #13288, #13142, #27561 ) ) ;
#1905 = EDGE_CURVE ( 'NONE', #20917, #20493, #3359, .T. ) ;
#1906 = CARTESIAN_POINT ( 'NONE',  ( 1.894214914920991921, -145.1469726764544532, 0.9536781033354796433 ) ) ;
#1907 = CARTESIAN_POINT ( 'NONE',  ( -55.24300891470650754, 0.009439835024159288004, 0.002702093572893217704 ) ) ;
#1908 = EDGE_CURVE ( 'NONE', #25971, #27431, #21556, .T. ) ;
#1909 = CARTESIAN_POINT ( 'NONE',  ( -1.046936909428682672, 43.93225665392633061, 12.93351869073227611 ) ) ;
#1910 = CARTESIAN_POINT ( 'NONE',  ( 109.1586900883932856, -0.006479576224403807948, -0.002995460350180787282 ) ) ;
#1911 = CARTESIAN_POINT ( 'NONE',  ( -12.82751273423880711, 35.32125660155448088, -33.78816682541299343 ) ) ;
#1912 = CARTESIAN_POINT ( 'NONE',  ( -7.733045908741344121, 38.67583825854200086, 35.49239760110631181 ) ) ;
#1913 =( BOUNDED_SURFACE ( )  B_SPLINE_SURFACE ( 3, 1, ( 
 ( #2922, #11838 ),
 ( #11699, #18157 ),
 ( #16147, #892 ),
 ( #5212, #24951 ) ),
 .UNSPECIFIED., .F., .F., .F. ) 
 B_SPLINE_SURFACE_WITH_KNOTS ( ( 4, 4 ),
 ( 2, 2 ),
 ( 0.000000000000000000, 1.000000000000000000 ),
 ( 0.000000000000000000, 1.000000000000000000 ),
 .UNSPECIFIED. ) 
 GEOMETRIC_REPRESENTATION_ITEM ( )  RATIONAL_B_SPLINE_SURFACE ( (
 ( 1.000000000000000000, 1.000000000000000000),
 ( 0.9956975270656955868, 0.8568959468854907557),
 ( 0.9956975270656955868, 0.8568959468854907557),
 ( 1.000000000000000000, 1.000000000000000000) ) ) 
 REPRESENTATION_ITEM ( '' )  SURFACE ( )  );
#1914 = DIRECTION ( 'NONE',  ( 0.000000000000000000, 0.000000000000000000, 1.000000000000000000 ) ) ;
#1915 = CARTESIAN_POINT ( 'NONE',  ( -1.050231094221226291, 36.90262059116464854, -27.12595454131517769 ) ) ;
#1916 = ORIENTED_EDGE ( 'NONE', *, *, #4191, .T. ) ;
#1918 = CARTESIAN_POINT ( 'NONE',  ( 10.93730112725970827, 42.00474393596263667, 145.2260730187401236 ) ) ;
#1917 = CARTESIAN_POINT ( 'NONE',  ( 32.73300124599741423, 117.3295799645430435, -8.473903470904879498 ) ) ;
#1919 = CARTESIAN_POINT ( 'NONE',  ( 26.04756280548354397, 22.44333019059152079, -110.9306483680200301 ) ) ;
#1920 = CARTESIAN_POINT ( 'NONE',  ( 109.1624594426973118, 0.01405141589344814472, 0.007576898892907140901 ) ) ;
#1921 = CARTESIAN_POINT ( 'NONE',  ( -1.583189561560253589, 29.24830400313217638, 36.01941156322755688 ) ) ;
#1922 = ORIENTED_EDGE ( 'NONE', *, *, #22807, .F. ) ;
#1923 = CARTESIAN_POINT ( 'NONE',  ( 25.64681081121879203, 97.99105938548001404, -56.09509703373240797 ) ) ;
#1924 = CARTESIAN_POINT ( 'NONE',  ( -4.178947244162637631, -31.41809272265950170, -37.51424432987639079 ) ) ;
#1926 = VECTOR ( 'NONE', #17137, 1000.000000000000341 ) ;
#1925 = CARTESIAN_POINT ( 'NONE',  ( -1.046935749539995353, -36.28605774377782467, -27.93995161054682441 ) ) ;
#1927 = EDGE_LOOP ( 'NONE', ( #17824, #15062, #17328, #17776 ) ) ;
#1928 = ORIENTED_EDGE ( 'NONE', *, *, #23656, .T. ) ;
#1929 = B_SPLINE_CURVE_WITH_KNOTS ( 'NONE', 3,
 ( #27527, #5508, #5814, #8116 ),
 .UNSPECIFIED., .F., .F.,
 ( 4, 4 ),
 ( 0.0009910334943225120648, 0.001982023823822943315 ),
 .UNSPECIFIED. ) ;
#1930 = CARTESIAN_POINT ( 'NONE',  ( -1.058197053496165108, -15.81317659443655721, 42.99116279335168400 ) ) ;
#1931 = AXIS2_PLACEMENT_3D ( 'NONE', #3378, #6929, #18534 ) ;
#1932 = EDGE_CURVE ( 'NONE', #27476, #19810, #14132, .T. ) ;
#1933 = CARTESIAN_POINT ( 'NONE',  ( 25.86096068574579832, 107.2082119295153149, 35.88291140783953637 ) ) ;
#1934 = CONICAL_SURFACE ( 'NONE', #18012, 34.60786435723138510, 0.8559913436420825139 ) ;
#1935 = ORIENTED_EDGE ( 'NONE', *, *, #21425, .T. ) ;
#1936 = CARTESIAN_POINT ( 'NONE',  ( -20.20700224038492721, 0.9908225410482660589, 29.58392382092671724 ) ) ;
#1937 = EDGE_CURVE ( 'NONE', #21184, #14114, #9893, .T. ) ;
#1938 = ADVANCED_FACE ( 'NONE', ( #11076 ), #8605, .F. ) ;
#1939 = EDGE_LOOP ( 'NONE', ( #21151, #2756, #7592, #26841 ) ) ;
#1940 = CARTESIAN_POINT ( 'NONE',  ( -55.24340739397742794, -0.009386184976284812215, 0.003826481709800012669 ) ) ;
#1941 = CARTESIAN_POINT ( 'NONE',  ( 109.1624594426973118, -0.01476644236456993789, -0.006066618937910856803 ) ) ;
#1942 = CARTESIAN_POINT ( 'NONE',  ( 6.224689322667630975, -129.4863684118292326, 71.79702446228257884 ) ) ;
#1943 = CARTESIAN_POINT ( 'NONE',  ( -55.24271866751342941, 0.008488649505346579707, -0.004256484107793386679 ) ) ;
#1944 = CARTESIAN_POINT ( 'NONE',  ( 109.1721716018069515, 0.008358834333178081361, 0.01488186354165287398 ) ) ;
#1945 = CARTESIAN_POINT ( 'NONE',  ( 25.70243777736188306, 55.83795591307134742, 98.18050844655094522 ) ) ;
#1946 = CARTESIAN_POINT ( 'NONE',  ( 24.01988960052066346, -9.440825210282529412, -130.7041393974934635 ) ) ;
#1947 = CIRCLE ( 'NONE', #3344, 117.6351876552689504 ) ;
#1948 = CARTESIAN_POINT ( 'NONE',  ( 2.433796855181205476, -98.43889364293931976, 107.1581411821782268 ) ) ;
#1949 = CARTESIAN_POINT ( 'NONE',  ( 2.430230287190581429, -31.67257033707599589, 142.0258656395020864 ) ) ;
#1950 = CARTESIAN_POINT ( 'NONE',  ( 25.64681081121880624, -112.2483031020014295, 12.21581276189770904 ) ) ;
#1952 =( BOUNDED_SURFACE ( )  B_SPLINE_SURFACE ( 3, 1, ( 
 ( #11016, #6280 ),
 ( #10744, #17553 ),
 ( #13661, #9210 ),
 ( #26476, #6781 ) ),
 .UNSPECIFIED., .F., .F., .F. ) 
 B_SPLINE_SURFACE_WITH_KNOTS ( ( 4, 4 ),
 ( 2, 2 ),
 ( 0.000000000000000000, 1.000000000000000000 ),
 ( 0.000000000000000000, 1.000000000000000000 ),
 .UNSPECIFIED. ) 
 GEOMETRIC_REPRESENTATION_ITEM ( )  RATIONAL_B_SPLINE_SURFACE ( (
 ( 1.000000000000000000, 1.000000000000000000),
 ( 0.9934239774497837239, 0.8357310067453919133),
 ( 0.9934239774497837239, 0.8357310067453919133),
 ( 1.000000000000000000, 1.000000000000000000) ) ) 
 REPRESENTATION_ITEM ( '' )  SURFACE ( )  );
#1951 = VECTOR ( 'NONE', #21579, 1000.000000000000227 ) ;
#1953 = ORIENTED_EDGE ( 'NONE', *, *, #9934, .T. ) ;
#1954 = CARTESIAN_POINT ( 'NONE',  ( 2.433796855181205476, -13.76554153471595043, -144.8571464219890572 ) ) ;
#1955 = CARTESIAN_POINT ( 'NONE',  ( 1.833838848569429469, -72.40075357737740092, 125.7577269771229851 ) ) ;
#1957 = CARTESIAN_POINT ( 'NONE',  ( 16.05277956358223435, 19.61822947416006357, 141.9568301782832975 ) ) ;
#1956 = CARTESIAN_POINT ( 'NONE',  ( -15.02187109954783217, 40.82269973458240031, -21.95370994985588098 ) ) ;
#1958 = CARTESIAN_POINT ( 'NONE',  ( -1.050229599974472627, -43.63650726458052986, 13.90955673306172002 ) ) ;
#1959 = CARTESIAN_POINT ( 'NONE',  ( 2.108393763691202683, 84.36147263237569405, 118.2927144690661692 ) ) ;
#1960 = EDGE_CURVE ( 'NONE', #13141, #17999, #5816, .T. ) ;
#1961 = CARTESIAN_POINT ( 'NONE',  ( -20.21097721712959938, 9.464413111084745367, -28.05863618200111986 ) ) ;
#1962 = ORIENTED_EDGE ( 'NONE', *, *, #19230, .F. ) ;
#1963 = CARTESIAN_POINT ( 'NONE',  ( -1.239374126674604337, -2.406737988130801309, 45.98822239537608425 ) ) ;
#1964 = FACE_OUTER_BOUND ( 'NONE', #20797, .T. ) ;
#1965 = FACE_OUTER_BOUND ( 'NONE', #24649, .T. ) ;
#1966 = FACE_OUTER_BOUND ( 'NONE', #27353, .T. ) ;
#1967 = EDGE_LOOP ( 'NONE', ( #3766, #28122, #10032, #6877 ) ) ;
#1968 = B_SPLINE_CURVE_WITH_KNOTS ( 'NONE', 3,
 ( #15373, #20261, #7052, #11070, #9351, #6762, #17811 ),
 .UNSPECIFIED., .F., .F.,
 ( 4, 3, 4 ),
 ( 0.000000000000000000, 0.006568092053401806615, 0.02506242213020846293 ),
 .UNSPECIFIED. ) ;
#1969 = CARTESIAN_POINT ( 'NONE',  ( 6.224689322667630975, -136.2818611715194663, 57.86870174583380333 ) ) ;
#1970 = ADVANCED_FACE ( 'NONE', ( #13091 ), #18705, .F. ) ;
#1971 = EDGE_CURVE ( 'NONE', #26248, #15804, #14000, .T. ) ;
#1972 = CONICAL_SURFACE ( 'NONE', #4276, 34.60786435723138510, 0.8559913436420825139 ) ;
#1973 = ORIENTED_EDGE ( 'NONE', *, *, #8707, .T. ) ;
#1974 = CARTESIAN_POINT ( 'NONE',  ( 24.01988960052063504, -84.46375358746846018, -100.1926921796492280 ) ) ;
#1975 = AXIS2_PLACEMENT_3D ( 'NONE', #8904, #21713, #1984 ) ;
#1976 = EDGE_CURVE ( 'NONE', #27143, #8890, #4314, .T. ) ;
#1977 = ORIENTED_EDGE ( 'NONE', *, *, #10816, .T. ) ;
#1978 = CARTESIAN_POINT ( 'NONE',  ( -28.41354790283022069, 1.249099604787400564, 23.16239616762929288 ) ) ;
#1979 = CARTESIAN_POINT ( 'NONE',  ( 1.833206310202332379, 108.3342540861879257, 96.54250248081029895 ) ) ;
#1980 = CARTESIAN_POINT ( 'NONE',  ( 1.894214914920994586, -71.74757687370546932, 126.1778046718833082 ) ) ;
#1981 = CARTESIAN_POINT ( 'NONE',  ( 32.73300124599732186, 0.000000000000000000, 0.000000000000000000 ) ) ;
#1982 = EDGE_CURVE ( 'NONE', #17730, #13364, #17120, .T. ) ;
#1983 = CARTESIAN_POINT ( 'NONE',  ( 55.79472521941428198, 0.7279028900793619306, 72.75035398477136539 ) ) ;
#1984 = DIRECTION ( 'NONE',  ( 0.000000000000000000, 0.000000000000000000, 1.000000000000000000 ) ) ;
#1985 = CARTESIAN_POINT ( 'NONE',  ( 25.64692232868534560, 23.79507962493625328, 110.3753891203787134 ) ) ;
#1986 = FACE_BOUND ( 'NONE', #22565, .T. ) ;
#1987 = CARTESIAN_POINT ( 'NONE',  ( -7.733045908741336127, 5.980865481988145937, -52.15131830128824220 ) ) ;
#1988 = FACE_OUTER_BOUND ( 'NONE', #11900, .T. ) ;
#1989 = AXIS2_PLACEMENT_3D ( 'NONE', #20453, #15990, #3186 ) ;
#1990 = DIRECTION ( 'NONE',  ( 1.000000000000000000, -6.938893903907226837E-18, 1.734723475976806709E-18 ) ) ;
#1991 = DIRECTION ( 'NONE',  ( 0.000000000000000000, -6.938893903907228378E-16, -1.000000000000000000 ) ) ;
#1992 = CARTESIAN_POINT ( 'NONE',  ( 30.59138290137868665, 115.8270707793589054, 9.457588828075607523 ) ) ;
#1993 = VERTEX_POINT ( 'NONE', #21338 ) ;
#1994 = ORIENTED_EDGE ( 'NONE', *, *, #23288, .F. ) ;
#1995 = CARTESIAN_POINT ( 'NONE',  ( -1.045287976400383290, -44.00138577190632816, 12.68782741917368106 ) ) ;
#1996 = CARTESIAN_POINT ( 'NONE',  ( -1.058473599757814521, 15.81436910992580991, 42.99101666105212161 ) ) ;
#1997 = CARTESIAN_POINT ( 'NONE',  ( -2.904412668506649808, -30.27712468694961956, 36.79926976721486653 ) ) ;
#1998 = CARTESIAN_POINT ( 'NONE',  ( -8.786685647604890903, -52.67761315067279781, 9.545808661481174795 ) ) ;
#1999 = CARTESIAN_POINT ( 'NONE',  ( -1.044556982611281493, 43.01635920718349126, -15.70482750345250267 ) ) ;
#2000 = CARTESIAN_POINT ( 'NONE',  ( 13.84597867724958853, 77.45414123936396322, -124.5889929031781520 ) ) ;
#2001 = CARTESIAN_POINT ( 'NONE',  ( 32.73300124599736449, -117.3295799645430435, 8.473903470905730373 ) ) ;
#2002 = ORIENTED_EDGE ( 'NONE', *, *, #26446, .T. ) ;
#2003 = FACE_OUTER_BOUND ( 'NONE', #18739, .T. ) ;
#2004 = CARTESIAN_POINT ( 'NONE',  ( 28.37599760073043242, 91.75439000741693008, 68.88138253892428509 ) ) ;
#2005 = CARTESIAN_POINT ( 'NONE',  ( 109.1592201516379674, 0.006044422199831473233, 0.005027640251764405217 ) ) ;
#2006 = CARTESIAN_POINT ( 'NONE',  ( -1.058473599757810746, -42.99101666105219977, 15.81436910992565004 ) ) ;
#2007 = ADVANCED_FACE ( 'NONE', ( #12553 ), #21629, .F. ) ;
#2008 = EDGE_LOOP ( 'NONE', ( #17015, #9500, #22791, #8704 ) ) ;
#2009 = CARTESIAN_POINT ( 'NONE',  ( 25.64699802086725455, -112.3172869996024588, -11.56593161917429846 ) ) ;
#2010 = CARTESIAN_POINT ( 'NONE',  ( -1.049817751779889008, 0.5106138415326839652, -45.79652915392414769 ) ) ;
#2011 = ORIENTED_EDGE ( 'NONE', *, *, #8618, .F. ) ;
#2012 = ADVANCED_FACE ( 'NONE', ( #6626 ), #15558, .F. ) ;
#2013 =( BOUNDED_SURFACE ( )  B_SPLINE_SURFACE ( 3, 1, ( 
 ( #14369, #27608 ),
 ( #12766, #23187 ),
 ( #20986, #23749 ),
 ( #1560, #25748 ) ),
 .UNSPECIFIED., .F., .F., .F. ) 
 B_SPLINE_SURFACE_WITH_KNOTS ( ( 4, 4 ),
 ( 2, 2 ),
 ( 0.000000000000000000, 1.000000000000000000 ),
 ( 0.000000000000000000, 1.000000000000000000 ),
 .UNSPECIFIED. ) 
 GEOMETRIC_REPRESENTATION_ITEM ( )  RATIONAL_B_SPLINE_SURFACE ( (
 ( 1.000000000000000000, 1.000000000000000000),
 ( 0.7789835883360576307, 0.9689951854195403280),
 ( 0.7789835883360576307, 0.9689951854195403280),
 ( 1.000000000000000000, 1.000000000000000000) ) ) 
 REPRESENTATION_ITEM ( '' )  SURFACE ( )  );
#2014 = ORIENTED_EDGE ( 'NONE', *, *, #11773, .T. ) ;
#2015 = ORIENTED_EDGE ( 'NONE', *, *, #25109, .T. ) ;
#2016 = ADVANCED_FACE ( 'NONE', ( #18245 ), #24600, .F. ) ;
#2017 = CARTESIAN_POINT ( 'NONE',  ( 1.832998868059858122, 96.70023740551269498, -108.1944082009147508 ) ) ;
#2018 = CARTESIAN_POINT ( 'NONE',  ( 26.11404676487257603, 57.58742681967449784, 97.48350837663630841 ) ) ;
#2019 = CARTESIAN_POINT ( 'NONE',  ( 1.833750490713712322, 72.32354185792559065, 125.8019536335922339 ) ) ;
#2020 = B_SPLINE_CURVE_WITH_KNOTS ( 'NONE', 3,
 ( #28244, #4074, #15136, #6124, #14876, #25697, #14730 ),
 .UNSPECIFIED., .F., .F.,
 ( 4, 3, 4 ),
 ( 0.000000000000000000, 0.006568092053401771921, 0.02506242213020852885 ),
 .UNSPECIFIED. ) ;
#2021 = CARTESIAN_POINT ( 'NONE',  ( -55.24300891470648622, -0.007734635432132420246, -0.006048736206180634067 ) ) ;
#2022 = ORIENTED_EDGE ( 'NONE', *, *, #13546, .T. ) ;
#2023 = EDGE_LOOP ( 'NONE', ( #1520, #20808, #18081, #14758 ) ) ;
#2024 = CARTESIAN_POINT ( 'NONE',  ( -25.21435515916043713, 34.05351380035342146, 6.169479169075106739 ) ) ;
#2025 = DIRECTION ( 'NONE',  ( 0.000000000000000000, 0.000000000000000000, 1.000000000000000000 ) ) ;
#2026 = DIRECTION ( 'NONE',  ( 1.000000000000000000, -6.938893903907226837E-18, 1.734723475976806709E-18 ) ) ;
#2027 = CARTESIAN_POINT ( 'NONE',  ( -25.21435515916043357, 6.169479169075458458, -34.05351380035335751 ) ) ;
#2028 = CARTESIAN_POINT ( 'NONE',  ( -1.044556982611269058, -36.05793013899078403, 28.22896456560707534 ) ) ;
#2029 = CARTESIAN_POINT ( 'NONE',  ( -1.050230346682680560, -26.92058491724839797, 37.05182464822011923 ) ) ;
#2030 = CARTESIAN_POINT ( 'NONE',  ( -1.113548883309563253, -44.18588492042580640, 12.28732181966563886 ) ) ;
#2031 = CARTESIAN_POINT ( 'NONE',  ( -25.21435515916043713, -6.169479169075696490, -34.05351380035330777 ) ) ;
#2032 = CARTESIAN_POINT ( 'NONE',  ( 25.81918753295377300, -0.9336804662319195813, -113.0221398901142180 ) ) ;
#2033 = ORIENTED_EDGE ( 'NONE', *, *, #26992, .T. ) ;
#2034 = ORIENTED_EDGE ( 'NONE', *, *, #24362, .T. ) ;
#2035 = CARTESIAN_POINT ( 'NONE',  ( 1.832998868059890096, -142.0492247521724494, 29.64765804470029664 ) ) ;
#2036 = CARTESIAN_POINT ( 'NONE',  ( -25.21435515916043713, -31.17620025257598471, -15.02493970636134613 ) ) ;
#2037 = ORIENTED_EDGE ( 'NONE', *, *, #16578, .T. ) ;
#2038 = EDGE_CURVE ( 'NONE', #20677, #20045, #958, .T. ) ;
#2039 = VERTEX_POINT ( 'NONE', #412 ) ;
#2040 = ORIENTED_EDGE ( 'NONE', *, *, #20635, .F. ) ;
#2041 =( BOUNDED_SURFACE ( )  B_SPLINE_SURFACE ( 3, 1, ( 
 ( #12791, #27916 ),
 ( #19420, #8087 ),
 ( #12243, #21301 ),
 ( #12373, #23343 ) ),
 .UNSPECIFIED., .F., .F., .F. ) 
 B_SPLINE_SURFACE_WITH_KNOTS ( ( 4, 4 ),
 ( 2, 2 ),
 ( 0.000000000000000000, 1.000000000000000000 ),
 ( 0.000000000000000000, 1.000000000000000000 ),
 .UNSPECIFIED. ) 
 GEOMETRIC_REPRESENTATION_ITEM ( )  RATIONAL_B_SPLINE_SURFACE ( (
 ( 1.000000000000000000, 1.000000000000000000),
 ( 0.9960225298536222738, 0.9999952330161893110),
 ( 0.9960225298536222738, 0.9999952330161893110),
 ( 1.000000000000000000, 1.000000000000000000) ) ) 
 REPRESENTATION_ITEM ( '' )  SURFACE ( )  );
#2042 = EDGE_CURVE ( 'NONE', #7528, #10527, #3721, .T. ) ;
#2043 = ADVANCED_FACE ( 'NONE', ( #26602 ), #27516, .F. ) ;
#2044 = CARTESIAN_POINT ( 'NONE',  ( 1.833838850855486369, 137.9800888515323152, 44.92600961247709535 ) ) ;
#2045 = CARTESIAN_POINT ( 'NONE',  ( 109.1586900883932856, -0.0008465529156546283815, 0.007088091345232576390 ) ) ;
#2046 = B_SPLINE_CURVE_WITH_KNOTS ( 'NONE', 3,
 ( #25557, #23398, #27975, #5975 ),
 .UNSPECIFIED., .F., .F.,
 ( 4, 4 ),
 ( 0.000000000000000000, 0.01077107196513895325 ),
 .UNSPECIFIED. ) ;
#2047 = CARTESIAN_POINT ( 'NONE',  ( -1.048996300304498419, 43.78665266739856321, 13.42280206896931638 ) ) ;
#2048 = DIRECTION ( 'NONE',  ( -0.7071067811865485719, 0.000000000000000000, -0.7071067811865465735 ) ) ;
#2049 = LINE ( 'NONE', #16905, #26727 ) ;
#2050 = CARTESIAN_POINT ( 'NONE',  ( -23.77929240705206482, 17.17389748746964173, -31.93650644494346835 ) ) ;
#2051 = CARTESIAN_POINT ( 'NONE',  ( 13.36082413113061307, 148.1362653801002978, 37.97423473099346580 ) ) ;
#2052 = CARTESIAN_POINT ( 'NONE',  ( 1.832998868059858122, -59.50898020732424953, -132.3466930259799597 ) ) ;
#2053 = VERTEX_POINT ( 'NONE', #15656 ) ;
#2054 = ORIENTED_EDGE ( 'NONE', *, *, #18217, .F. ) ;
#2056 = CARTESIAN_POINT ( 'NONE',  ( -28.41354790283022069, -5.969609727608182759, -22.41474081377998218 ) ) ;
#2055 = LINE ( 'NONE', #10858, #3816 ) ;
#2057 = CARTESIAN_POINT ( 'NONE',  ( -4.473127245936434626, 31.51789735524247504, 37.94261489385684882 ) ) ;
#2058 = DIRECTION ( 'NONE',  ( 0.000000000000000000, 0.000000000000000000, 1.000000000000000000 ) ) ;
#2059 = CARTESIAN_POINT ( 'NONE',  ( 2.430230287190572103, 133.5180086894999363, -57.85706160874012483 ) ) ;
#2060 = CARTESIAN_POINT ( 'NONE',  ( 26.11404676487257603, 107.3263591096430218, 36.06104232266487486 ) ) ;
#2061 = ORIENTED_EDGE ( 'NONE', *, *, #18923, .T. ) ;
#2062 = CARTESIAN_POINT ( 'NONE',  ( -8.259864102781671491, -36.24929574824938783, -38.68084189741935575 ) ) ;
#2063 = CARTESIAN_POINT ( 'NONE',  ( -1.048172774974284405, -27.73787987941035027, -36.44231470008705998 ) ) ;
#2064 = ORIENTED_EDGE ( 'NONE', *, *, #7038, .F. ) ;
#2065 = VERTEX_POINT ( 'NONE', #24762 ) ;
#2066 = ADVANCED_FACE ( 'NONE', ( #15817 ), #21690, .F. ) ;
#2067 = CARTESIAN_POINT ( 'NONE',  ( -7.733045908741340568, -10.42750254442575120, -51.44704017882771296 ) ) ;
#2068 = CARTESIAN_POINT ( 'NONE',  ( 25.70243777736189728, 107.1912711514954850, 35.59945151684112830 ) ) ;
#2069 = ORIENTED_EDGE ( 'NONE', *, *, #12705, .F. ) ;
#2070 = CARTESIAN_POINT ( 'NONE',  ( 2.108393763691202238, -125.1820217068190857, -73.75286979200589599 ) ) ;
#2071 = CIRCLE ( 'NONE', #22344, 151.1787379149930359 ) ;
#2072 = ORIENTED_EDGE ( 'NONE', *, *, #22683, .T. ) ;
#2073 =( BOUNDED_SURFACE ( )  B_SPLINE_SURFACE ( 3, 1, ( 
 ( #17109, #12781 ),
 ( #8348, #25905 ),
 ( #15490, #21570 ),
 ( #12922, #13198 ) ),
 .UNSPECIFIED., .F., .F., .F. ) 
 B_SPLINE_SURFACE_WITH_KNOTS ( ( 4, 4 ),
 ( 2, 2 ),
 ( 0.000000000000000000, 1.000000000000000000 ),
 ( 0.000000000000000000, 1.000000000000000000 ),
 .UNSPECIFIED. ) 
 GEOMETRIC_REPRESENTATION_ITEM ( )  RATIONAL_B_SPLINE_SURFACE ( (
 ( 1.000000000000000000, 1.000000000000000000),
 ( 0.7789835883360576307, 0.9689951854195403280),
 ( 0.7789835883360576307, 0.9689951854195403280),
 ( 1.000000000000000000, 1.000000000000000000) ) ) 
 REPRESENTATION_ITEM ( '' )  SURFACE ( )  );
#2074 = CARTESIAN_POINT ( 'NONE',  ( 6.224689322667630975, -18.02516478984242809, 146.9579047224769113 ) ) ;
#2075 = CARTESIAN_POINT ( 'NONE',  ( 109.1592201516379674, -0.001934867487021774525, -0.007620268632971101234 ) ) ;
#2076 = CARTESIAN_POINT ( 'NONE',  ( 1.832998868059858122, 14.63705790014199692, -144.3700883710215521 ) ) ;
#2077 = CARTESIAN_POINT ( 'NONE',  ( 55.79472521941428198, 72.27573336313963637, -8.328398066091017071 ) ) ;
#2078 = CARTESIAN_POINT ( 'NONE',  ( 55.49584447822657296, 36.50733923851286278, -62.69727227546362514 ) ) ;
#2079 = LINE ( 'NONE', #23725, #3685 ) ;
#2080 = ADVANCED_FACE ( 'NONE', ( #7332, #24624 ), #16096, .T. ) ;
#2081 = B_SPLINE_CURVE_WITH_KNOTS ( 'NONE', 3,
 ( #27281, #7593, #7739, #10033 ),
 .UNSPECIFIED., .F., .F.,
 ( 4, 4 ),
 ( 1.977889076651310254E-16, 0.001982023823822932906 ),
 .UNSPECIFIED. ) ;
#2082 = CARTESIAN_POINT ( 'NONE',  ( -20.37983603106074426, 7.753708011498974706, 28.74620395171554321 ) ) ;
#2083 = PRODUCT ( 'pinion 3', 'pinion 3', '', ( #5724 ) ) ;
#2085 = CARTESIAN_POINT ( 'NONE',  ( -21.41427618760446450, -30.75468365310881325, -1.815001260755733536 ) ) ;
#2084 = CARTESIAN_POINT ( 'NONE',  ( 109.1592201516379674, 0.004867031887019543715, 0.006174480289199423509 ) ) ;
#2086 = DIRECTION ( 'NONE',  ( -0.000000000000000000, 1.000000000000000000, -0.000000000000000000 ) ) ;
#2087 = VERTEX_POINT ( 'NONE', #26890 ) ;
#2088 = EDGE_LOOP ( 'NONE', ( #25991, #17783, #19091, #7467 ) ) ;
#2089 = CARTESIAN_POINT ( 'NONE',  ( 5.340103556456540446, -13.12023871801021180, -146.8647350107030718 ) ) ;
#2090 = CARTESIAN_POINT ( 'NONE',  ( 109.1592201516379674, 0.0005146241775982810093, 0.007845213074654433863 ) ) ;
#2091 = CARTESIAN_POINT ( 'NONE',  ( -55.24271866751342941, -0.008433070970613520956, 0.004365563123935277227 ) ) ;
#2092 = CARTESIAN_POINT ( 'NONE',  ( -6.574463467970653063, -47.03022655117387529, 20.55340846381182018 ) ) ;
#2093 = CARTESIAN_POINT ( 'NONE',  ( 26.11404676487257603, 97.48350837663606683, 57.58742681967482469 ) ) ;
#2094 = CARTESIAN_POINT ( 'NONE',  ( -2.904412668506665351, 17.42365698954698061, -44.35433137608945486 ) ) ;
#2095 = ADVANCED_FACE ( 'NONE', ( #15954 ), #28259, .F. ) ;
#2096 = EDGE_LOOP ( 'NONE', ( #28233, #26782, #28214, #17757 ) ) ;
#2097 = CARTESIAN_POINT ( 'NONE',  ( -55.24300891470648622, -0.005486913146696059326, -0.008142823778062177609 ) ) ;
#2098 = CARTESIAN_POINT ( 'NONE',  ( -4.780792508754321268, 25.98388465890140964, 42.16805077400930202 ) ) ;
#2099 = EDGE_CURVE ( 'NONE', #342, #23477, #6369, .T. ) ;
#2100 = CARTESIAN_POINT ( 'NONE',  ( 25.86096068574579476, -92.04529103340814800, 65.64181925268293583 ) ) ;
#2101 = CARTESIAN_POINT ( 'NONE',  ( -2.911734481061400537, 30.23325065583413718, 36.84482841982617884 ) ) ;
#2103 = ADVANCED_FACE ( 'NONE', ( #1409 ), #18552, .F. ) ;
#2102 = ORIENTED_EDGE ( 'NONE', *, *, #21324, .F. ) ;
#2104 = CARTESIAN_POINT ( 'NONE',  ( -8.786685647604890903, -9.545808661480982948, -52.67761315067281913 ) ) ;
#2105 = ORIENTED_EDGE ( 'NONE', *, *, #20102, .F. ) ;
#2106 = DIRECTION ( 'NONE',  ( 0.000000000000000000, 0.000000000000000000, 1.000000000000000000 ) ) ;
#2107 = CARTESIAN_POINT ( 'NONE',  ( 25.87036335909426299, 65.65170964736253723, -92.04585932622704547 ) ) ;
#2108 = ORIENTED_EDGE ( 'NONE', *, *, #24654, .T. ) ;
#2109 = CARTESIAN_POINT ( 'NONE',  ( -23.79223135445719706, -22.01133905265668034, 24.83942264280426926 ) ) ;
#2110 = CARTESIAN_POINT ( 'NONE',  ( -55.24300891470650754, -0.006048736206179085827, -0.007734635432136639961 ) ) ;
#2111 = DIRECTION ( 'NONE',  ( 0.000000000000000000, 5.223019709707975211E-21, -1.000000000000000000 ) ) ;
#2112 = CARTESIAN_POINT ( 'NONE',  ( 1.833485406944043827, 142.0485807715649571, -29.64752363041402816 ) ) ;
#2113 = CARTESIAN_POINT ( 'NONE',  ( 109.1778270068192853, 0.008236503545664811132, -0.004349865064712430361 ) ) ;
#2114 = CARTESIAN_POINT ( 'NONE',  ( -25.21435515916025594, 1.749597353048488237E-16, -4.373993382621220594E-17 ) ) ;
#2115 = CARTESIAN_POINT ( 'NONE',  ( -1.046935749539985583, -1.275486069320154847, 45.77872888003168583 ) ) ;
#2116 = CARTESIAN_POINT ( 'NONE',  ( 109.1587776205901577, 8.330235397644728467E-05, -0.007328861771496577443 ) ) ;
#2117 = FACE_OUTER_BOUND ( 'NONE', #27397, .T. ) ;
#2118 = CARTESIAN_POINT ( 'NONE',  ( 10.93730112725978287, -125.1380233598484182, 84.82621002473399585 ) ) ;
#2119 = CARTESIAN_POINT ( 'NONE',  ( -1.056502255334265339, -43.72121397317214786, 13.66916755949895546 ) ) ;
#2120 = VERTEX_POINT ( 'NONE', #12490 ) ;
#2121 = EDGE_CURVE ( 'NONE', #1001, #14400, #21914, .T. ) ;
#2122 = ORIENTED_EDGE ( 'NONE', *, *, #2933, .T. ) ;
#2123 = CARTESIAN_POINT ( 'NONE',  ( -25.21435515916025594, 34.29329011225976842, -4.655591116594504086 ) ) ;
#2124 = CARTESIAN_POINT ( 'NONE',  ( -20.47566262905009893, -28.85746289809572218, 7.708089517695493775 ) ) ;
#2125 = CARTESIAN_POINT ( 'NONE',  ( 13.36082413113063083, -147.2768864064165086, -41.18148072373763569 ) ) ;
#2126 = CARTESIAN_POINT ( 'NONE',  ( 1.833603222531973165, 72.93978951866159832, -125.4455769441935047 ) ) ;
#2127 = DIRECTION ( 'NONE',  ( 0.7637818620346801257, 0.02150485345384395286, -0.6451161201712182214 ) ) ;
#2128 = CARTESIAN_POINT ( 'NONE',  ( -21.41427618760457463, -23.81423075802597111, -19.54551635498120277 ) ) ;
#2129 = ORIENTED_EDGE ( 'NONE', *, *, #3415, .F. ) ;
#2130 = CARTESIAN_POINT ( 'NONE',  ( 28.37599760073042887, 113.9023239246302808, 13.77583212279370350 ) ) ;
#2131 = CARTESIAN_POINT ( 'NONE',  ( 13.36082413113061307, 56.35051087434963080, 142.1654513177089996 ) ) ;
#2132 = CARTESIAN_POINT ( 'NONE',  ( 25.64681081121880624, 23.06870491922473931, -110.5293738517606243 ) ) ;
#2133 = CARTESIAN_POINT ( 'NONE',  ( -55.24271866751342941, 0.004256484107795918508, -0.008488649505343059953 ) ) ;
#2134 = EDGE_CURVE ( 'NONE', #21234, #11951, #11610, .T. ) ;
#2135 = B_SPLINE_CURVE_WITH_KNOTS ( 'NONE', 3,
 ( #14058, #6163, #28281, #21530 ),
 .UNSPECIFIED., .F., .F.,
 ( 4, 4 ),
 ( 0.000000000000000000, 0.008383560773332719013 ),
 .UNSPECIFIED. ) ;
#2136 = B_SPLINE_CURVE_WITH_KNOTS ( 'NONE', 3,
 ( #3890, #13081, #25914, #19691, #24044, #6617, #19421 ),
 .UNSPECIFIED., .F., .F.,
 ( 4, 3, 4 ),
 ( 0.000000000000000000, 0.006568092053401751972, 0.02506242213020840742 ),
 .UNSPECIFIED. ) ;
#2137 = CARTESIAN_POINT ( 'NONE',  ( -2.911734481061404090, 40.13920818157116344, 25.69892591260225245 ) ) ;
#2138 = ORIENTED_EDGE ( 'NONE', *, *, #2285, .T. ) ;
#2139 = CARTESIAN_POINT ( 'NONE',  ( -20.20700224038492721, 18.19058640100257662, 23.35150625415638714 ) ) ;
#2140 = ORIENTED_EDGE ( 'NONE', *, *, #27157, .T. ) ;
#2141 = ORIENTED_EDGE ( 'NONE', *, *, #20467, .F. ) ;
#2142 = EDGE_LOOP ( 'NONE', ( #9932, #6346, #22327, #5320 ) ) ;
#2143 = CARTESIAN_POINT ( 'NONE',  ( 26.11404676487259024, 24.64483677385001315, -110.5078194225158654 ) ) ;
#2144 = CARTESIAN_POINT ( 'NONE',  ( -24.53237795827032031, -16.68575684089471878, 29.54731592868582979 ) ) ;
#2145 = FACE_OUTER_BOUND ( 'NONE', #853, .T. ) ;
#2146 = B_SPLINE_CURVE_WITH_KNOTS ( 'NONE', 3,
 ( #12838, #314, #11123, #10982, #15557, #2044, #15130, #33, #24524, #15706 ),
 .UNSPECIFIED., .F., .F.,
 ( 4, 3, 3, 4 ),
 ( 2.775557561562891351E-17, 0.0002669559177086200147, 0.0005339118354151127163, 0.001067817517169171622 ),
 .UNSPECIFIED. ) ;
#2147 = ORIENTED_EDGE ( 'NONE', *, *, #6401, .T. ) ;
#2148 = CARTESIAN_POINT ( 'NONE',  ( 1.833485406944043827, 73.01664920992966756, 125.4007332306548221 ) ) ;
#2149 = CARTESIAN_POINT ( 'NONE',  ( -6.588769196390773963, 47.06982923582537381, 20.50531526814514294 ) ) ;
#2150 = ORIENTED_EDGE ( 'NONE', *, *, #14062, .F. ) ;
#2151 = EDGE_CURVE ( 'NONE', #19236, #27960, #23321, .T. ) ;
#2152 = CARTESIAN_POINT ( 'NONE',  ( 26.11404676487257603, 92.25884714080409310, 65.63269960453273200 ) ) ;
#2153 = ORIENTED_EDGE ( 'NONE', *, *, #19990, .F. ) ;
#2154 = CARTESIAN_POINT ( 'NONE',  ( 2.108985857320916146, 126.4634971826984469, 71.53406810961526219 ) ) ;
#2155 = EDGE_CURVE ( 'NONE', #4790, #27931, #5601, .T. ) ;
#2156 = B_SPLINE_CURVE_WITH_KNOTS ( 'NONE', 3,
 ( #15816, #22448, #13935, #20266, #4877, #15953, #24623, #13789, #27019, #15655 ),
 .UNSPECIFIED., .F., .F.,
 ( 4, 3, 3, 4 ),
 ( 3.393552799879628878E-17, 0.0002669559177086209363, 0.0005339118354151020911, 0.001067817517169162515 ),
 .UNSPECIFIED. ) ;
#2157 = CARTESIAN_POINT ( 'NONE',  ( 2.263178113027050742, -1.401567040889206917, 145.3892419963351017 ) ) ;
#2158 = DIRECTION ( 'NONE',  ( 0.5914120900931444380, 0.6476200150380150289, 0.4804373588864832567 ) ) ;
#2159 = CARTESIAN_POINT ( 'NONE',  ( -1.619063947482197729, -2.489035965910479486, -46.30105812165547974 ) ) ;
#2160 = CARTESIAN_POINT ( 'NONE',  ( -55.24390624410018802, 0.007503127514282199352, -0.007245494385991655198 ) ) ;
#2161 = FACE_OUTER_BOUND ( 'NONE', #13939, .T. ) ;
#2162 = EDGE_CURVE ( 'NONE', #10634, #24113, #8232, .T. ) ;
#2163 = CARTESIAN_POINT ( 'NONE',  ( 55.49584447822657296, -0.2676470673951589219, -72.55110015779771970 ) ) ;
#2164 = FACE_OUTER_BOUND ( 'NONE', #24804, .T. ) ;
#2165 = ADVANCED_FACE ( 'NONE', ( #25049 ), #9704, .F. ) ;
#2166 = ORIENTED_EDGE ( 'NONE', *, *, #1305, .F. ) ;
#2167 = ORIENTED_EDGE ( 'NONE', *, *, #10704, .T. ) ;
#2168 = CARTESIAN_POINT ( 'NONE',  ( -1.539760825549679080, 38.84664866728813593, 25.17088484262099612 ) ) ;
#2169 = CARTESIAN_POINT ( 'NONE',  ( 30.58324630866341209, 33.60235057864129260, -116.1819705588610105 ) ) ;
#2170 = ORIENTED_EDGE ( 'NONE', *, *, #26446, .F. ) ;
#2171 = ORIENTED_EDGE ( 'NONE', *, *, #20137, .T. ) ;
#2172 = ORIENTED_EDGE ( 'NONE', *, *, #6808, .T. ) ;
#2173 = LINE ( 'NONE', #8967, #137 ) ;
#2174 = DIRECTION ( 'NONE',  ( 0.000000000000000000, 0.000000000000000000, -1.000000000000000000 ) ) ;
#2175 = CARTESIAN_POINT ( 'NONE',  ( 2.108985857320901491, -144.3577886602087119, 16.46110181986639986 ) ) ;
#2176 = CARTESIAN_POINT ( 'NONE',  ( 55.49584447822657296, 58.85239198729244947, -42.42793568432897189 ) ) ;
#2177 = CARTESIAN_POINT ( 'NONE',  ( -1.259920593601975058, -45.95412615877143026, -2.243284667987618608 ) ) ;
#2178 = CARTESIAN_POINT ( 'NONE',  ( 109.1586900883932856, 0.006561743627143330412, -0.002810909342011619870 ) ) ;
#2179 = CARTESIAN_POINT ( 'NONE',  ( -55.25297051322618813, 0.01483298743814672610, -0.001818774723749509541 ) ) ;
#2180 = CARTESIAN_POINT ( 'NONE',  ( 2.433796855181219243, -132.3327394885235435, 60.50726454507858421 ) ) ;
#2181 = ADVANCED_FACE ( 'NONE', ( #14362 ), #4741, .F. ) ;
#2182 = DIRECTION ( 'NONE',  ( 0.5914120900931444380, 0.7333565075147332468, 0.3352908775637229444 ) ) ;
#2183 = CARTESIAN_POINT ( 'NONE',  ( 25.64660436782557440, -65.89729635302973065, 91.68669413043116379 ) ) ;
#2184 = CARTESIAN_POINT ( 'NONE',  ( -1.050230346682680560, 26.91946103437159721, 37.05264119692660785 ) ) ;
#2185 = CARTESIAN_POINT ( 'NONE',  ( -20.20700224038492721, -23.35150625415671755, -18.19058640100215385 ) ) ;
#2187 = ORIENTED_EDGE ( 'NONE', *, *, #15179, .T. ) ;
#2186 = EDGE_CURVE ( 'NONE', #21439, #4100, #15730, .T. ) ;
#2188 = ORIENTED_EDGE ( 'NONE', *, *, #8930, .T. ) ;
#2190 = CARTESIAN_POINT ( 'NONE',  ( 109.1624594426973260, 0.002863932759303830771, 0.01570508117119675390 ) ) ;
#2189 = CARTESIAN_POINT ( 'NONE',  ( -25.21435515916025594, 1.749597353048488237E-16, -4.373993382621220594E-17 ) ) ;
#2191 = CARTESIAN_POINT ( 'NONE',  ( 1.833838850093439943, -144.3148369740567603, -15.16809710532209721 ) ) ;
#2192 = CARTESIAN_POINT ( 'NONE',  ( -1.259920593601978833, -28.82601305773628297, 35.85909937955954518 ) ) ;
#2193 = CARTESIAN_POINT ( 'NONE',  ( -55.24198130335446422, 0.009170435128245573234, 0.001516807524708093389 ) ) ;
#2194 = CARTESIAN_POINT ( 'NONE',  ( -1.583189561560252701, 36.01941156322829585, 29.24830400313125978 ) ) ;
#2195 = DIRECTION ( 'NONE',  ( 0.000000000000000000, 0.000000000000000000, 1.000000000000000000 ) ) ;
#2196 = ORIENTED_EDGE ( 'NONE', *, *, #7772, .T. ) ;
#2197 = CARTESIAN_POINT ( 'NONE',  ( 25.64699802086724034, 97.66487797954091832, -56.66140964017631632 ) ) ;
#2198 = DIRECTION ( 'NONE',  ( 0.000000000000000000, 0.000000000000000000, 1.000000000000000000 ) ) ;
#2199 = CARTESIAN_POINT ( 'NONE',  ( -1.045287976400365970, -37.92705037016778391, -25.66401692419976399 ) ) ;
#2200 = ORIENTED_EDGE ( 'NONE', *, *, #13155, .F. ) ;
#2201 = B_SPLINE_CURVE_WITH_KNOTS ( 'NONE', 3,
 ( #24292, #26709, #17652, #241, #7019, #26432 ),
 .UNSPECIFIED., .F., .F.,
 ( 4, 2, 4 ),
 ( 0.000000000000000000, 0.003570751334075635691, 0.007141502668151271382 ),
 .UNSPECIFIED. ) ;
#2202 = ORIENTED_EDGE ( 'NONE', *, *, #1466, .T. ) ;
#2203 = CARTESIAN_POINT ( 'NONE',  ( 5.340103579038255610, -128.8311297206837480, -71.72120379026158332 ) ) ;
#2204 = ORIENTED_EDGE ( 'NONE', *, *, #8746, .F. ) ;
#2205 = CARTESIAN_POINT ( 'NONE',  ( -22.23342874802667879, -2.180636882146296696, 31.55488258420093572 ) ) ;
#2206 = ORIENTED_EDGE ( 'NONE', *, *, #3536, .F. ) ;
#2207 = B_SPLINE_CURVE_WITH_KNOTS ( 'NONE', 3,
 ( #22732, #5432, #13922, #7464, #20401, #20544, #826 ),
 .UNSPECIFIED., .F., .F.,
 ( 4, 3, 4 ),
 ( 0.000000000000000000, 0.02398743853561317169, 0.04000277880656214619 ),
 .UNSPECIFIED. ) ;
#2208 = CARTESIAN_POINT ( 'NONE',  ( -22.23226125620943705, 16.78323347921918796, -26.80886670319641851 ) ) ;
#2209 = AXIS2_PLACEMENT_3D ( 'NONE', #2489, #21800, #2195 ) ;
#2210 = ORIENTED_EDGE ( 'NONE', *, *, #21590, .T. ) ;
#2211 = CARTESIAN_POINT ( 'NONE',  ( -1.155001620486251213, 2.068551059060327546, -45.85729774065935516 ) ) ;
#2212 = CARTESIAN_POINT ( 'NONE',  ( -28.41354790283022069, -19.47297445639558333, -12.60397206714825558 ) ) ;
#2213 = FACE_OUTER_BOUND ( 'NONE', #12790, .T. ) ;
#2214 = CARTESIAN_POINT ( 'NONE',  ( -1.048171036023497704, 13.17819047681665090, 43.86077206077055735 ) ) ;
#2215 = FACE_OUTER_BOUND ( 'NONE', #13923, .T. ) ;
#2216 = CARTESIAN_POINT ( 'NONE',  ( 25.65782528836479770, 55.95807498711486971, 98.07785559018897459 ) ) ;
#2217 = CARTESIAN_POINT ( 'NONE',  ( 13.84597867724975373, -4.782757490006857459, 146.6243035057531472 ) ) ;
#2218 = ADVANCED_FACE ( 'NONE', ( #23601 ), #16949, .T. ) ;
#2219 = CARTESIAN_POINT ( 'NONE',  ( 26.11404676487259024, 103.8885755249569485, 45.01677474591446781 ) ) ;
#2220 = CARTESIAN_POINT ( 'NONE',  ( 25.64681081121879203, -11.38886654529750331, 112.3352186517030447 ) ) ;
#2221 = CARTESIAN_POINT ( 'NONE',  ( -1.583189561560255143, 38.94740041318295454, -25.21827308671246470 ) ) ;
#2222 = EDGE_CURVE ( 'NONE', #19171, #20839, #16953, .T. ) ;
#2223 = ORIENTED_EDGE ( 'NONE', *, *, #12506, .T. ) ;
#2224 = DIRECTION ( 'NONE',  ( 0.000000000000000000, 5.223019709707975211E-21, -1.000000000000000000 ) ) ;
#2226 = CARTESIAN_POINT ( 'NONE',  ( -8.259864102781506290, -46.42816643551554989, -25.58601832199090609 ) ) ;
#2225 = CARTESIAN_POINT ( 'NONE',  ( -1.056502255334264895, 45.80535052436397336, -0.5104472526221494055 ) ) ;
#2227 = ADVANCED_FACE ( 'NONE', ( #14791 ), #1685, .F. ) ;
#2228 = DIRECTION ( 'NONE',  ( 1.000000000000000000, -6.938893903907226837E-18, 1.734723475976806709E-18 ) ) ;
#2229 = CARTESIAN_POINT ( 'NONE',  ( 13.84597867724972708, 144.4146018799366118, -25.80666409311425369 ) ) ;
#2230 = CARTESIAN_POINT ( 'NONE',  ( -55.24390624410018802, -0.009209468562450790971, 0.004896917417127758312 ) ) ;
#2231 = CARTESIAN_POINT ( 'NONE',  ( 25.64704443564076897, -34.76451658509458298, -107.4261196778966365 ) ) ;
#2232 = CARTESIAN_POINT ( 'NONE',  ( 109.1586900883932856, 0.001582822706024254473, -0.006960773163856035471 ) ) ;
#2233 = DIRECTION ( 'NONE',  ( -1.000000000000000000, -0.000000000000000000, -0.000000000000000000 ) ) ;
#2234 = CARTESIAN_POINT ( 'NONE',  ( 8.186469777910911461, -90.56875928602647718, -118.7566730872910767 ) ) ;
#2235 = ORIENTED_EDGE ( 'NONE', *, *, #12128, .T. ) ;
#2236 = B_SPLINE_CURVE_WITH_KNOTS ( 'NONE', 3,
 ( #1547, #10353, #19115, #27887, #8184, #18545, #16946 ),
 .UNSPECIFIED., .F., .F.,
 ( 4, 3, 4 ),
 ( 4.358266177795834884E-16, 0.02816610861753242670, 0.04000277880656261803 ),
 .UNSPECIFIED. ) ;
#2237 = EDGE_CURVE ( 'NONE', #10703, #14908, #23718, .T. ) ;
#2238 = CARTESIAN_POINT ( 'NONE',  ( 109.1624594426973118, -0.002129375066974356807, -0.01582142368019175474 ) ) ;
#2239 = CARTESIAN_POINT ( 'NONE',  ( -1.045287976400362417, -12.68782741917263657, 44.00138577190661948 ) ) ;
#2240 =( BOUNDED_SURFACE ( )  B_SPLINE_SURFACE ( 3, 1, ( 
 ( #12545, #20790 ),
 ( #7574, #5391 ),
 ( #27262, #25799 ),
 ( #14849, #17152 ) ),
 .UNSPECIFIED., .F., .F., .F. ) 
 B_SPLINE_SURFACE_WITH_KNOTS ( ( 4, 4 ),
 ( 2, 2 ),
 ( 0.000000000000000000, 1.000000000000000000 ),
 ( 0.000000000000000000, 1.000000000000000000 ),
 .UNSPECIFIED. ) 
 GEOMETRIC_REPRESENTATION_ITEM ( )  RATIONAL_B_SPLINE_SURFACE ( (
 ( 1.000000000000000000, 1.000000000000000000),
 ( 0.9956975270656955868, 0.8568959468854907557),
 ( 0.9956975270656955868, 0.8568959468854907557),
 ( 1.000000000000000000, 1.000000000000000000) ) ) 
 REPRESENTATION_ITEM ( '' )  SURFACE ( )  );
#2241 = ORIENTED_EDGE ( 'NONE', *, *, #144, .T. ) ;
#2242 = DIRECTION ( 'NONE',  ( 0.000000000000000000, 0.000000000000000000, 1.000000000000000000 ) ) ;
#2243 = CARTESIAN_POINT ( 'NONE',  ( 30.59141879584293378, -92.40465812955496006, -70.47510900703881020 ) ) ;
#2244 = CARTESIAN_POINT ( 'NONE',  ( 109.1586900883932856, 0.003656351050331851926, 0.006130969560687375870 ) ) ;
#2245 = VERTEX_POINT ( 'NONE', #6009 ) ;
#2246 = CARTESIAN_POINT ( 'NONE',  ( -55.24728320129491266, -0.003868537197316542463, 0.01402509393918130107 ) ) ;
#2247 = EDGE_CURVE ( 'NONE', #3848, #23708, #12632, .T. ) ;
#2248 = DIRECTION ( 'NONE',  ( 0.7563875759206388771, 0.1685564395263429993, 0.6320336713238481341 ) ) ;
#2249 = CARTESIAN_POINT ( 'NONE',  ( -16.86833981943425087, -31.95666732167541113, 30.57013526701953054 ) ) ;
#2250 = CARTESIAN_POINT ( 'NONE',  ( -1.583189561560255143, -43.29471907393753582, -16.68617981233685299 ) ) ;
#2251 = DIRECTION ( 'NONE',  ( 0.000000000000000000, 5.223019709708233256E-21, -1.000000000000000000 ) ) ;
#2252 = CARTESIAN_POINT ( 'NONE',  ( 109.1778270068192853, -0.004106684808172176952, 0.008360410075186655923 ) ) ;
#2253 = EDGE_CURVE ( 'NONE', #26396, #17575, #1382, .T. ) ;
#2254 = B_SPLINE_CURVE_WITH_KNOTS ( 'NONE', 3,
 ( #1360, #10167, #20511, #11881, #941, #9730, #18499, #27273, #4086, #6132 ),
 .UNSPECIFIED., .F., .F.,
 ( 4, 3, 3, 4 ),
 ( 1.387778780781445676E-17, 0.0002669560319015683520, 0.0005492286108966489347, 0.0008315040496093463072 ),
 .UNSPECIFIED. ) ;
#2255 = CARTESIAN_POINT ( 'NONE',  ( 25.64660436782558151, 110.5628080555245845, 22.90783756890889578 ) ) ;
#2256 = CARTESIAN_POINT ( 'NONE',  ( 32.73300124599734318, 81.52272205837205377, 84.80615050150403533 ) ) ;
#2257 = CARTESIAN_POINT ( 'NONE',  ( 2.433796855181205476, 13.76554153471693454, 144.8571464219890004 ) ) ;
#2258 = CARTESIAN_POINT ( 'NONE',  ( -21.81686047589425925, 34.70276904128910189, 16.72402253294277230 ) ) ;
#2259 = ORIENTED_EDGE ( 'NONE', *, *, #28204, .T. ) ;
#2260 = ORIENTED_EDGE ( 'NONE', *, *, #2387, .F. ) ;
#2261 = CARTESIAN_POINT ( 'NONE',  ( -20.57838717382308147, -29.92853265176830746, 1.611677988432673070 ) ) ;
#2262 = CARTESIAN_POINT ( 'NONE',  ( -1.583189561560252701, -25.21827308671259615, -38.94740041318285506 ) ) ;
#2263 = CARTESIAN_POINT ( 'NONE',  ( -55.25719721206881729, -0.01079965405819840671, -0.002847566758682798602 ) ) ;
#2264 = CARTESIAN_POINT ( 'NONE',  ( 2.263178113027036531, -141.9207360579559634, -31.59906256848430672 ) ) ;
#2265 = CARTESIAN_POINT ( 'NONE',  ( 2.433796855181205476, 126.7346379669265843, -71.49415740224942795 ) ) ;
#2266 = CARTESIAN_POINT ( 'NONE',  ( 25.64708010899965629, -91.37928813995122823, -66.32331961783478391 ) ) ;
#2267 = ORIENTED_EDGE ( 'NONE', *, *, #1937, .F. ) ;
#2268 = CARTESIAN_POINT ( 'NONE',  ( -55.24271866751342941, 0.006671293903668402275, 0.006757859501010043089 ) ) ;
#2269 = CARTESIAN_POINT ( 'NONE',  ( 109.1778270068192853, -0.004349865064721190715, 0.008236503545668676096 ) ) ;
#2270 = LINE ( 'NONE', #17400, #10620 ) ;
#2271 = CARTESIAN_POINT ( 'NONE',  ( 8.186469777910879486, -149.3111477498017621, 3.468244369821378292 ) ) ;
#2272 = CARTESIAN_POINT ( 'NONE',  ( 2.430230287190572103, 74.01081053031275303, -125.2872625092154522 ) ) ;
#2273 = CARTESIAN_POINT ( 'NONE',  ( 30.59141879584315404, 49.72305007553607226, -105.0379937202710323 ) ) ;
#2274 = CARTESIAN_POINT ( 'NONE',  ( 1.833721034905664737, -107.5990973104329385, 97.36162733017677340 ) ) ;
#2275 = CARTESIAN_POINT ( 'NONE',  ( -1.031422197589716205, -15.60268798220668174, -43.06660437151303711 ) ) ;
#2276 = ORIENTED_EDGE ( 'NONE', *, *, #12388, .F. ) ;
#2277 = B_SPLINE_CURVE_WITH_KNOTS ( 'NONE', 3,
 ( #12442, #16917, #18936, #10320 ),
 .UNSPECIFIED., .F., .F.,
 ( 4, 4 ),
 ( 1.892757412642747523E-16, 0.001982023823822945917 ),
 .UNSPECIFIED. ) ;
#2278 = ORIENTED_EDGE ( 'NONE', *, *, #13597, .T. ) ;
#2279 = ORIENTED_EDGE ( 'NONE', *, *, #28227, .F. ) ;
#2280 =( BOUNDED_SURFACE ( )  B_SPLINE_SURFACE ( 3, 1, ( 
 ( #26852, #8889 ),
 ( #17649, #22558 ),
 ( #4549, #15474 ),
 ( #15773, #2827 ) ),
 .UNSPECIFIED., .F., .F., .F. ) 
 B_SPLINE_SURFACE_WITH_KNOTS ( ( 4, 4 ),
 ( 2, 2 ),
 ( 0.000000000000000000, 1.000000000000000000 ),
 ( 0.000000000000000000, 1.000000000000000000 ),
 .UNSPECIFIED. ) 
 GEOMETRIC_REPRESENTATION_ITEM ( )  RATIONAL_B_SPLINE_SURFACE ( (
 ( 1.000000000000000000, 1.000000000000000000),
 ( 0.9960225298536222738, 0.9999952330161893110),
 ( 0.9960225298536222738, 0.9999952330161893110),
 ( 1.000000000000000000, 1.000000000000000000) ) ) 
 REPRESENTATION_ITEM ( '' )  SURFACE ( )  );
#2281 = CARTESIAN_POINT ( 'NONE',  ( -20.21097721712958872, 28.26295595852185727, -8.835581498567558256 ) ) ;
#2282 = CARTESIAN_POINT ( 'NONE',  ( 9.884929003653626367, 128.2151425008052570, -78.87917189084775771 ) ) ;
#2283 = EDGE_CURVE ( 'NONE', #17335, #15244, #2681, .T. ) ;
#2284 = CARTESIAN_POINT ( 'NONE',  ( 13.36082413113061307, 143.3553710183989551, 53.25066407421853398 ) ) ;
#2285 = EDGE_CURVE ( 'NONE', #18662, #27008, #14480, .T. ) ;
#2286 = AXIS2_PLACEMENT_3D ( 'NONE', #25208, #23065, #12110 ) ;
#2287 = ORIENTED_EDGE ( 'NONE', *, *, #21230, .F. ) ;
#2288 = CARTESIAN_POINT ( 'NONE',  ( -19.53423201713129842, 1.355459634611817431E-16, -3.388649086529543578E-17 ) ) ;
#2289 = AXIS2_PLACEMENT_3D ( 'NONE', #22998, #9598, #18215 ) ;
#2290 = B_SPLINE_CURVE_WITH_KNOTS ( 'NONE', 3,
 ( #24397, #26533, #22522, #24551, #4814, #16171 ),
 .UNSPECIFIED., .F., .F.,
 ( 4, 2, 4 ),
 ( 3.469446951953613804E-18, 0.0004335184443139973023, 0.0008670368886279911352 ),
 .UNSPECIFIED. ) ;
#2291 = CARTESIAN_POINT ( 'NONE',  ( -1.619063947482201282, -11.94059994246191359, -44.80407745103779860 ) ) ;
#2292 = ORIENTED_EDGE ( 'NONE', *, *, #6506, .F. ) ;
#2293 = CARTESIAN_POINT ( 'NONE',  ( -21.41427618760446094, 30.75468365310879193, 1.815001260755948254 ) ) ;
#2294 = ORIENTED_EDGE ( 'NONE', *, *, #14119, .T. ) ;
#2295 = CARTESIAN_POINT ( 'NONE',  ( 2.433796855181219243, 31.67151202413165478, -142.0211193075552956 ) ) ;
#2296 = CARTESIAN_POINT ( 'NONE',  ( -1.155031165708881202, -12.20332162035433576, 44.25214473648924951 ) ) ;
#2297 = CARTESIAN_POINT ( 'NONE',  ( 21.16825799904904670, -71.50503315297801521, -115.0183107335396642 ) ) ;
#2298 = CARTESIAN_POINT ( 'NONE',  ( 55.79472521941426777, -21.78881894124655716, -69.41463258328535346 ) ) ;
#2299 = CARTESIAN_POINT ( 'NONE',  ( 109.1778270068192853, 0.002542344697966444390, -0.008960903982066569656 ) ) ;
#2300 = CARTESIAN_POINT ( 'NONE',  ( 32.73300124599732186, 0.000000000000000000, 0.000000000000000000 ) ) ;
#2301 = CARTESIAN_POINT ( 'NONE',  ( 8.186469829614226867, -3.468244397268101853, 149.3111477833937784 ) ) ;
#2302 = CARTESIAN_POINT ( 'NONE',  ( -20.20700224038492010, -18.19058640100240254, -23.35150625415651859 ) ) ;
#2303 = CARTESIAN_POINT ( 'NONE',  ( -20.57838717382308502, 27.96569011373086866, -10.78122205917010135 ) ) ;
#2304 = CARTESIAN_POINT ( 'NONE',  ( 6.224689322667630975, -144.2687111683192995, -33.28770499679482953 ) ) ;
#2305 = ORIENTED_EDGE ( 'NONE', *, *, #27, .F. ) ;
#2306 = VERTEX_POINT ( 'NONE', #22086 ) ;
#2307 = FACE_OUTER_BOUND ( 'NONE', #25115, .T. ) ;
#2308 = AXIS2_PLACEMENT_3D ( 'NONE', #25916, #6209, #24046 ) ;
#2309 = CARTESIAN_POINT ( 'NONE',  ( 25.81918753295380142, 107.2019194967340496, -35.81374485821504550 ) ) ;
#2310 = B_SPLINE_CURVE_WITH_KNOTS ( 'NONE', 3,
 ( #16928, #25443, #12318, #28136, #10184, #18800 ),
 .UNSPECIFIED., .F., .F.,
 ( 4, 2, 4 ),
 ( 2.168404344971008868E-19, 0.0006311571484586057891, 0.001262314296917211361 ),
 .UNSPECIFIED. ) ;
#2311 = ORIENTED_EDGE ( 'NONE', *, *, #7679, .T. ) ;
#2312 = VECTOR ( 'NONE', #7939, 1000.000000000000000 ) ;
#2313 = EDGE_LOOP ( 'NONE', ( #14788, #4286, #662, #16977 ) ) ;
#2314 = ORIENTED_EDGE ( 'NONE', *, *, #27127, .T. ) ;
#2315 = PRESENTATION_LAYER_ASSIGNMENT (  '', '', ( #11074 ) ) ;
#2316 = DIRECTION ( 'NONE',  ( 0.000000000000000000, 0.000000000000000000, 1.000000000000000000 ) ) ;
#2317 = ADVANCED_FACE ( 'NONE', ( #6559 ), #1952, .F. ) ;
#2318 = EDGE_CURVE ( 'NONE', #26396, #15398, #7863, .T. ) ;
#2319 = EDGE_CURVE ( 'NONE', #13547, #14642, #10272, .T. ) ;
#2320 = B_SPLINE_CURVE_WITH_KNOTS ( 'NONE', 3,
 ( #3342, #23657, #12541, #1467, #3914, #1322 ),
 .UNSPECIFIED., .F., .F.,
 ( 4, 2, 4 ),
 ( 1.257674520083185143E-17, 0.0006311636237756764172, 0.001262327247551340475 ),
 .UNSPECIFIED. ) ;
#2321 = CARTESIAN_POINT ( 'NONE',  ( 25.64681081121880624, 11.38886654529674303, 112.3352186517031157 ) ) ;
#2322 = CARTESIAN_POINT ( 'NONE',  ( 2.063896406836609909, -145.2631347824382999, 1.344106060019858884 ) ) ;
#2323 = ADVANCED_FACE ( 'NONE', ( #17970 ), #12784, .T. ) ;
#2324 = CARTESIAN_POINT ( 'NONE',  ( 2.108985857320889945, 43.67763756616835735, -138.5727354014053390 ) ) ;
#2325 = CARTESIAN_POINT ( 'NONE',  ( -16.86833981943422600, -7.884812276281804699, 43.51541671545733436 ) ) ;
#2326 = CARTESIAN_POINT ( 'NONE',  ( 32.73300124599739291, -66.00340565729273123, -97.37344512919924000 ) ) ;
#2327 = AXIS2_PLACEMENT_3D ( 'NONE', #17394, #14956, #19284 ) ;
#2328 = CARTESIAN_POINT ( 'NONE',  ( 25.65782528836479770, 24.04194111109019616, -110.3293115225704781 ) ) ;
#2329 = LINE ( 'NONE', #20182, #19916 ) ;
#2330 = DIRECTION ( 'NONE',  ( 0.000000000000000000, 0.000000000000000000, 1.000000000000000000 ) ) ;
#2331 = CARTESIAN_POINT ( 'NONE',  ( -1.048171036023513247, 26.08692787913922473, 37.64178826568577563 ) ) ;
#2332 = CARTESIAN_POINT ( 'NONE',  ( 1.833838850093452599, -117.3962623502780218, 85.29338149487179521 ) ) ;
#2333 = VECTOR ( 'NONE', #11479, 1000.000000000000114 ) ;
#2334 = ORIENTED_EDGE ( 'NONE', *, *, #2356, .F. ) ;
#2335 = ORIENTED_EDGE ( 'NONE', *, *, #27227, .F. ) ;
#2336 = CARTESIAN_POINT ( 'NONE',  ( -1.056502255334265339, 37.35734037467636171, -26.51074901220517432 ) ) ;
#2337 = CARTESIAN_POINT ( 'NONE',  ( 30.59141879584320023, 79.74795589902169013, -84.53180090073595920 ) ) ;
#2338 = CARTESIAN_POINT ( 'NONE',  ( -20.20997486282891131, -0.3303599360441825672, -29.60348406988234871 ) ) ;
#2339 = CARTESIAN_POINT ( 'NONE',  ( -1.031422197589716205, -36.13727897780108123, 28.14735071801782951 ) ) ;
#2340 = CARTESIAN_POINT ( 'NONE',  ( 2.433796855181233454, -109.1007109081219539, -96.28145139437795308 ) ) ;
#2341 = ORIENTED_EDGE ( 'NONE', *, *, #15603, .T. ) ;
#2342 = VERTEX_POINT ( 'NONE', #10819 ) ;
#2343 = DIRECTION ( 'NONE',  ( 0.000000000000000000, 5.223019709708233256E-21, -1.000000000000000000 ) ) ;
#2344 = DIRECTION ( 'NONE',  ( -0.5914120900931443270, 0.8063295922669343474, -0.008020494142999051376 ) ) ;
#2345 = ORIENTED_EDGE ( 'NONE', *, *, #11680, .F. ) ;
#2346 = ORIENTED_EDGE ( 'NONE', *, *, #11026, .T. ) ;
#2347 = CARTESIAN_POINT ( 'NONE',  ( -1.056502255334265339, 14.64009593116102614, -43.40574022158779144 ) ) ;
#2348 = ORIENTED_EDGE ( 'NONE', *, *, #15709, .T. ) ;
#2349 = CARTESIAN_POINT ( 'NONE',  ( 109.1586900883932856, -0.004851151255037395443, -0.005236795036860529204 ) ) ;
#2350 = ORIENTED_EDGE ( 'NONE', *, *, #11494, .T. ) ;
#2351 = EDGE_CURVE ( 'NONE', #3038, #24477, #17696, .T. ) ;
#2352 = CIRCLE ( 'NONE', #12041, 12.50000000000000178 ) ;
#2353 = CARTESIAN_POINT ( 'NONE',  ( -1.583189561560256253, 43.29471907393742924, -16.68617981233717273 ) ) ;
#2354 = AXIS2_PLACEMENT_3D ( 'NONE', #16199, #15916, #18345 ) ;
#2355 = ORIENTED_EDGE ( 'NONE', *, *, #27918, .F. ) ;
#2356 = EDGE_CURVE ( 'NONE', #26821, #26828, #20000, .T. ) ;
#2357 = CARTESIAN_POINT ( 'NONE',  ( -1.583189561560256253, 16.68617981233763459, 43.29471907393723029 ) ) ;
#2358 = CARTESIAN_POINT ( 'NONE',  ( -1.239374126674604337, 25.08410696974242882, -38.61989855450947573 ) ) ;
#2359 = CARTESIAN_POINT ( 'NONE',  ( 109.1721716018069657, -0.01673651515803011372, -0.003350975118864128570 ) ) ;
#2360 = CARTESIAN_POINT ( 'NONE',  ( -2.911734481061396540, 12.03743348210780439, -46.11606034418766598 ) ) ;
#2361 = B_SPLINE_CURVE_WITH_KNOTS ( 'NONE', 3,
 ( #13666, #9646, #13956, #27340, #11513, #11369, #20580, #5321 ),
 .UNSPECIFIED., .F., .F.,
 ( 4, 2, 2, 4 ),
 ( 0.000000000000000000, 0.0002429588503611220809, 0.0004859177007222441618, 0.0009718354014444829025 ),
 .UNSPECIFIED. ) ;
#2362 = CARTESIAN_POINT ( 'NONE',  ( -55.24390624410018802, 0.001451500391951047672, 0.01032895241566990016 ) ) ;
#2363 = B_SPLINE_CURVE_WITH_KNOTS ( 'NONE', 3,
 ( #20654, #11886, #9883, #22554, #22410, #9737, #16342, #20377 ),
 .UNSPECIFIED., .F., .F.,
 ( 4, 2, 2, 4 ),
 ( 1.993045536433795054E-17, 0.0002429588503611349558, 0.0004859177007222500165, 0.0009718354014444676153 ),
 .UNSPECIFIED. ) ;
#2364 = CARTESIAN_POINT ( 'NONE',  ( 109.1592201516379674, 0.005027640251764384401, -0.006044422199831492315 ) ) ;
#2366 = CARTESIAN_POINT ( 'NONE',  ( 26.11404676487259024, -33.91085499298451822, 108.0249973236466445 ) ) ;
#2365 = FACE_OUTER_BOUND ( 'NONE', #9824, .T. ) ;
#2367 = CARTESIAN_POINT ( 'NONE',  ( 119.2224693531408803, -90.00000000000005684, 19.99999999999990052 ) ) ;
#2368 = ORIENTED_EDGE ( 'NONE', *, *, #28417, .T. ) ;
#2369 = CARTESIAN_POINT ( 'NONE',  ( 109.1586900883932856, -0.006819617742892453323, 0.002109621908824122621 ) ) ;
#2370 = CARTESIAN_POINT ( 'NONE',  ( 32.73300124599735739, 62.10906484417237294, 99.90245962373859356 ) ) ;
#2371 = FACE_OUTER_BOUND ( 'NONE', #12750, .T. ) ;
#2372 = FACE_OUTER_BOUND ( 'NONE', #12315, .T. ) ;
#2373 = CARTESIAN_POINT ( 'NONE',  ( 2.108985857320910817, -125.1820688103226757, 73.75356715683039965 ) ) ;
#2374 = CARTESIAN_POINT ( 'NONE',  ( -1.259920593601984162, 16.33409644610551581, -43.01175804832013938 ) ) ;
#2375 = VECTOR ( 'NONE', #3215, 1000.000000000000114 ) ;
#2376 = CARTESIAN_POINT ( 'NONE',  ( 109.1592201516379674, -0.005027640251767255368, -0.006044422199822518590 ) ) ;
#2377 = CARTESIAN_POINT ( 'NONE',  ( 26.11404676487259024, 55.62948129436384193, -98.61392875273304526 ) ) ;
#2378 = B_SPLINE_CURVE_WITH_KNOTS ( 'NONE', 3,
 ( #2494, #18035, #18176, #336, #22672, #7266, #2643, #15888 ),
 .UNSPECIFIED., .F., .F.,
 ( 4, 2, 2, 4 ),
 ( 0.000000000000000000, 0.002761524886576648043, 0.005523049773153296087, 0.01104609954630659217 ),
 .UNSPECIFIED. ) ;
#2379 = CARTESIAN_POINT ( 'NONE',  ( 2.430230287190581429, -118.5711603495686859, 84.35270093935218938 ) ) ;
#2380 = ORIENTED_EDGE ( 'NONE', *, *, #14936, .T. ) ;
#2381 = CARTESIAN_POINT ( 'NONE',  ( 13.36082413113061307, -142.1654513177092269, 56.35051087434914763 ) ) ;
#2382 = FACE_OUTER_BOUND ( 'NONE', #17560, .T. ) ;
#2383 = CARTESIAN_POINT ( 'NONE',  ( -1.464342487929861214, -35.90631960086394514, 29.09292098541700611 ) ) ;
#2384 = ADVANCED_FACE ( 'NONE', ( #15389 ), #4912, .F. ) ;
#2385 = VERTEX_POINT ( 'NONE', #17829 ) ;
#2386 = CARTESIAN_POINT ( 'NONE',  ( 109.1721716018069657, -0.01254847260354819902, 0.01157047143379294832 ) ) ;
#2387 = EDGE_CURVE ( 'NONE', #15661, #7846, #15779, .T. ) ;
#2388 = CARTESIAN_POINT ( 'NONE',  ( 94.22246935314088034, -90.00000000000005684, -6.938893903907228378E-15 ) ) ;
#2389 = FACE_OUTER_BOUND ( 'NONE', #809, .T. ) ;
#2390 = ORIENTED_EDGE ( 'NONE', *, *, #13514, .T. ) ;
#2391 = EDGE_CURVE ( 'NONE', #422, #12008, #11260, .T. ) ;
#2392 = DIRECTION ( 'NONE',  ( 0.000000000000000000, 0.000000000000000000, 1.000000000000000000 ) ) ;
#2393 = CONICAL_SURFACE ( 'NONE', #4710, 117.6351876552689504, 0.9945805576725580410 ) ;
#2394 = CARTESIAN_POINT ( 'NONE',  ( -55.25719721206881729, -0.007063345920776780730, 0.008651607285660046359 ) ) ;
#2395 = CONICAL_SURFACE ( 'NONE', #1047, 117.6351876552689504, 0.9945805576725580410 ) ;
#2396 = CARTESIAN_POINT ( 'NONE',  ( 1.833206310202350808, 132.2594754479313792, -59.70089235435300878 ) ) ;
#2397 = LINE ( 'NONE', #24032, #23245 ) ;
#2398 = CARTESIAN_POINT ( 'NONE',  ( -7.711401346138398338, -6.030154970217270538, -52.11446537925909439 ) ) ;
#2399 = CARTESIAN_POINT ( 'NONE',  ( 1.833838848569426361, -132.4919773286273426, 59.18404309081314807 ) ) ;
#2400 = EDGE_LOOP ( 'NONE', ( #14615, #9558, #4860, #2982 ) ) ;
#2401 = CARTESIAN_POINT ( 'NONE',  ( -22.34422965417126150, -17.95715691811022552, 33.39267070835840912 ) ) ;
#2402 = CARTESIAN_POINT ( 'NONE',  ( 109.1624594426973260, -0.002863932759303939191, -0.01570508117119672614 ) ) ;
#2403 = CARTESIAN_POINT ( 'NONE',  ( -20.20997486282892552, 3.551351076220724598E-15, -29.60348406988233450 ) ) ;
#2404 = CARTESIAN_POINT ( 'NONE',  ( 1.833485406944057594, 108.1939177044926055, 96.69979900902202985 ) ) ;
#2405 = EDGE_LOOP ( 'NONE', ( #20624, #1599, #14286, #5807 ) ) ;
#2406 = ORIENTED_EDGE ( 'NONE', *, *, #26096, .T. ) ;
#2407 = ORIENTED_EDGE ( 'NONE', *, *, #12847, .T. ) ;
#2408 = CARTESIAN_POINT ( 'NONE',  ( 25.64708010899965629, 103.1718249732474249, 45.87517365398517910 ) ) ;
#2409 = CARTESIAN_POINT ( 'NONE',  ( 109.1586900883932856, 0.005833932871487514972, -0.004113747441000934618 ) ) ;
#2410 = CARTESIAN_POINT ( 'NONE',  ( 25.64681081121879203, 75.86069728268988399, 83.63051021305928145 ) ) ;
#2411 = CARTESIAN_POINT ( 'NONE',  ( -20.57838717382308147, 27.96569011373101077, 10.78122205916971055 ) ) ;
#2412 = CARTESIAN_POINT ( 'NONE',  ( -8.786685647604890903, -53.04920435127188938, -7.199674155858766689 ) ) ;
#2413 = EDGE_CURVE ( 'NONE', #3326, #5301, #16411, .T. ) ;
#2414 = CARTESIAN_POINT ( 'NONE',  ( 25.64681081121879203, 46.30456157731328659, 102.9795863647030103 ) ) ;
#2415 = CIRCLE ( 'NONE', #18517, 80.00000000000000000 ) ;
#2416 = VERTEX_POINT ( 'NONE', #2143 ) ;
#2417 = CARTESIAN_POINT ( 'NONE',  ( 25.65782528836479059, -34.34372400279175963, -107.5689571161382929 ) ) ;
#2418 = CARTESIAN_POINT ( 'NONE',  ( -1.619063947482197729, -11.94059994246129008, 44.80407745103795492 ) ) ;
#2419 = FACE_OUTER_BOUND ( 'NONE', #7849, .T. ) ;
#2420 = CARTESIAN_POINT ( 'NONE',  ( -8.786685647604890903, 23.24040270374391426, -48.22796981442777309 ) ) ;
#2421 = CARTESIAN_POINT ( 'NONE',  ( 25.70243777736188306, 102.8829101922930960, 46.60897284577198718 ) ) ;
#2422 = CARTESIAN_POINT ( 'NONE',  ( 109.1586900883932856, -0.002301750759607945531, -0.006757191295056121962 ) ) ;
#2424 =( BOUNDED_SURFACE ( )  B_SPLINE_SURFACE ( 3, 1, ( 
 ( #17347, #2221 ),
 ( #15598, #6715 ),
 ( #21681, #17634 ),
 ( #24416, #8721 ) ),
 .UNSPECIFIED., .F., .F., .F. ) 
 B_SPLINE_SURFACE_WITH_KNOTS ( ( 4, 4 ),
 ( 2, 2 ),
 ( 0.000000000000000000, 1.000000000000000000 ),
 ( 0.000000000000000000, 1.000000000000000000 ),
 .UNSPECIFIED. ) 
 GEOMETRIC_REPRESENTATION_ITEM ( )  RATIONAL_B_SPLINE_SURFACE ( (
 ( 1.000000000000000000, 1.000000000000000000),
 ( 0.9934239774497837239, 0.8357310067453919133),
 ( 0.9934239774497837239, 0.8357310067453919133),
 ( 1.000000000000000000, 1.000000000000000000) ) ) 
 REPRESENTATION_ITEM ( '' )  SURFACE ( )  );
#2423 = CIRCLE ( 'NONE', #9360, 143.8872038478949946 ) ;
#2425 = ADVANCED_FACE ( 'NONE', ( #6497 ), #7879, .F. ) ;
#2426 = VECTOR ( 'NONE', #14860, 1000.000000000000227 ) ;
#2427 = VERTEX_POINT ( 'NONE', #14381 ) ;
#2428 = CARTESIAN_POINT ( 'NONE',  ( 1.833206308920097172, 142.0914675761166563, -29.44113170198408014 ) ) ;
#2429 = CARTESIAN_POINT ( 'NONE',  ( -1.619063947482197729, -11.94059994246129008, 44.80407745103795492 ) ) ;
#2430 = ORIENTED_EDGE ( 'NONE', *, *, #3842, .F. ) ;
#2431 = EDGE_CURVE ( 'NONE', #9946, #7628, #9797, .T. ) ;
#2432 = B_SPLINE_CURVE_WITH_KNOTS ( 'NONE', 3,
 ( #21925, #44, #11553, #22508, #16009, #13418, #2773, #20330 ),
 .UNSPECIFIED., .F., .F.,
 ( 4, 2, 2, 4 ),
 ( 0.000000000000000000, 0.002761524886576654115, 0.005523049773153308230, 0.01104609954630660952 ),
 .UNSPECIFIED. ) ;
#2433 = ORIENTED_EDGE ( 'NONE', *, *, #24449, .F. ) ;
#2434 = ORIENTED_EDGE ( 'NONE', *, *, #3842, .T. ) ;
#2435 = CARTESIAN_POINT ( 'NONE',  ( 9.884929003653608603, 114.6392083957130836, -97.56484214660510190 ) ) ;
#2436 = CARTESIAN_POINT ( 'NONE',  ( 26.04756280548354042, 84.84709444968909509, 74.90181827458373220 ) ) ;
#2437 = CARTESIAN_POINT ( 'NONE',  ( -1.031422197589711987, 25.67058493451442658, -37.93675465142480618 ) ) ;
#2438 = ORIENTED_EDGE ( 'NONE', *, *, #7235, .F. ) ;
#2439 = FACE_OUTER_BOUND ( 'NONE', #3040, .T. ) ;
#2440 = AXIS2_PLACEMENT_3D ( 'NONE', #25533, #3626, #19456 ) ;
#2441 = VECTOR ( 'NONE', #18680, 1000.000000000000000 ) ;
#2442 = CARTESIAN_POINT ( 'NONE',  ( 26.11404676487259024, 67.46175819463365997, 90.92995828888226129 ) ) ;
#2443 = VERTEX_POINT ( 'NONE', #100 ) ;
#2444 = CARTESIAN_POINT ( 'NONE',  ( 25.87036335909427720, 92.04585932622775601, 65.65170964736162773 ) ) ;
#2445 = VERTEX_POINT ( 'NONE', #6734 ) ;
#2446 = CARTESIAN_POINT ( 'NONE',  ( -1.583189561560253589, 38.94740041318330981, 25.21827308671188561 ) ) ;
#2447 = CARTESIAN_POINT ( 'NONE',  ( 24.01988960052062083, -61.78678588189937670, -115.5642432877697416 ) ) ;
#2448 = CARTESIAN_POINT ( 'NONE',  ( 2.108393763691190248, -145.2872457912033042, -1.280847988473292398 ) ) ;
#2449 = DIRECTION ( 'NONE',  ( 0.000000000000000000, 5.223019709708233256E-21, -1.000000000000000000 ) ) ;
#2450 = CARTESIAN_POINT ( 'NONE',  ( -1.619063947482197729, -11.94059994246129008, 44.80407745103795492 ) ) ;
#2451 = LINE ( 'NONE', #20300, #27627 ) ;
#2452 = B_SPLINE_CURVE_WITH_KNOTS ( 'NONE', 3,
 ( #24765, #27022, #7336, #16098 ),
 .UNSPECIFIED., .F., .F.,
 ( 4, 4 ),
 ( 0.000000000000000000, 0.01077107196513877631 ),
 .UNSPECIFIED. ) ;
#2453 = CARTESIAN_POINT ( 'NONE',  ( -1.619063947482197729, 43.26576862488456499, 16.67502769180516964 ) ) ;
#2454 = CARTESIAN_POINT ( 'NONE',  ( -1.113427685307003534, -35.91272432484637278, 28.52429901637207266 ) ) ;
#2455 = CARTESIAN_POINT ( 'NONE',  ( -55.24728320129491266, 0.008013189884952347936, 0.01214321324517130159 ) ) ;
#2456 = DIRECTION ( 'NONE',  ( 0.000000000000000000, 0.000000000000000000, -1.000000000000000000 ) ) ;
#2457 = CARTESIAN_POINT ( 'NONE',  ( 2.108985857320919699, -43.67763756616749049, 138.5727354014056516 ) ) ;
#2458 = CARTESIAN_POINT ( 'NONE',  ( 13.36082413113061307, -148.1362653801000135, -37.97423473099446767 ) ) ;
#2459 = ADVANCED_FACE ( 'NONE', ( #2382 ), #2721, .F. ) ;
#2460 = ORIENTED_EDGE ( 'NONE', *, *, #16287, .F. ) ;
#2461 =( BOUNDED_SURFACE ( )  B_SPLINE_SURFACE ( 3, 1, ( 
 ( #16845, #3880 ),
 ( #3312, #1156 ),
 ( #21293, #25344 ),
 ( #21000, #3586 ) ),
 .UNSPECIFIED., .F., .F., .F. ) 
 B_SPLINE_SURFACE_WITH_KNOTS ( ( 4, 4 ),
 ( 2, 2 ),
 ( 0.000000000000000000, 1.000000000000000000 ),
 ( 0.000000000000000000, 1.000000000000000000 ),
 .UNSPECIFIED. ) 
 GEOMETRIC_REPRESENTATION_ITEM ( )  RATIONAL_B_SPLINE_SURFACE ( (
 ( 1.000000000000000000, 1.000000000000000000),
 ( 0.6386103224230316178, 0.9954351624131538845),
 ( 0.6386103224230316178, 0.9954351624131538845),
 ( 1.000000000000000000, 1.000000000000000000) ) ) 
 REPRESENTATION_ITEM ( '' )  SURFACE ( )  );
#2462 = EDGE_CURVE ( 'NONE', #7846, #5380, #13233, .T. ) ;
#2463 = ORIENTED_EDGE ( 'NONE', *, *, #28164, .F. ) ;
#2464 = CARTESIAN_POINT ( 'NONE',  ( 2.433796855181205476, -96.28145139437610567, -109.1007109081235882 ) ) ;
#2465 = CARTESIAN_POINT ( 'NONE',  ( 25.98552792386799126, 107.2612904323495542, -35.98568266743403399 ) ) ;
#2466 = B_SPLINE_CURVE_WITH_KNOTS ( 'NONE', 3,
 ( #23195, #3585, #8201, #27779, #23468, #6052, #12364, #14807, #3878, #1005, #5463, #9799, #27336 ),
 .UNSPECIFIED., .F., .F.,
 ( 4, 3, 3, 3, 4 ),
 ( 6.938893903907227607E-18, 0.0007657099931970539480, 0.001531419946797919806, 0.002296279302920154267, 0.003061450627205759834 ),
 .UNSPECIFIED. ) ;
#2467 = ORIENTED_EDGE ( 'NONE', *, *, #15714, .F. ) ;
#2468 = EDGE_CURVE ( 'NONE', #28211, #20564, #27509, .T. ) ;
#2469 = ORIENTED_EDGE ( 'NONE', *, *, #23569, .F. ) ;
#2470 = ORIENTED_EDGE ( 'NONE', *, *, #5642, .T. ) ;
#2471 = CARTESIAN_POINT ( 'NONE',  ( -55.24198130335446422, -0.004276389980775889554, -0.008252882783650218948 ) ) ;
#2472 = ORIENTED_EDGE ( 'NONE', *, *, #11972, .F. ) ;
#2473 = CARTESIAN_POINT ( 'NONE',  ( -55.24390624410018802, 0.004572280736703349113, -0.009374879212967143077 ) ) ;
#2474 = CARTESIAN_POINT ( 'NONE',  ( 25.73574536432414561, -107.1893601970592300, -35.67555431182938719 ) ) ;
#2475 = CARTESIAN_POINT ( 'NONE',  ( -1.048994561756796839, 43.31369460697995777, 14.87838255483211469 ) ) ;
#2476 = ORIENTED_EDGE ( 'NONE', *, *, #9411, .T. ) ;
#2477 = CARTESIAN_POINT ( 'NONE',  ( 1.833485406944057594, -144.3694338680884073, -14.63699153649508311 ) ) ;
#2478 = CARTESIAN_POINT ( 'NONE',  ( -20.21097721650787449, 24.14932365326977148, 17.13687097598110398 ) ) ;
#2479 = CARTESIAN_POINT ( 'NONE',  ( -8.786685647604890903, 25.35688121747502066, -47.14957014837363403 ) ) ;
#2480 = CARTESIAN_POINT ( 'NONE',  ( 2.433796855181205476, -142.6247129145649808, 28.83182736670489987 ) ) ;
#2481 = CARTESIAN_POINT ( 'NONE',  ( 1.834118845439484335, -29.99597360113166289, 141.9759513273463938 ) ) ;
#2482 = CARTESIAN_POINT ( 'NONE',  ( 32.73300124599738581, 84.80615050150476009, -81.52272205837115848 ) ) ;
#2483 = EDGE_CURVE ( 'NONE', #11098, #16995, #6093, .T. ) ;
#2484 = ORIENTED_EDGE ( 'NONE', *, *, #17025, .T. ) ;
#2486 = CARTESIAN_POINT ( 'NONE',  ( -8.786685647604890903, -52.67761315067293282, -9.545808661480407409 ) ) ;
#2485 = CARTESIAN_POINT ( 'NONE',  ( 25.64692872815575342, 91.15762468787745831, 66.62748454953189992 ) ) ;
#2487 = CARTESIAN_POINT ( 'NONE',  ( 14.74894986621300319, -1.023413983156987147E-16, 2.558534957892467869E-17 ) ) ;
#2488 = CARTESIAN_POINT ( 'NONE',  ( -1.056502255334264895, -36.75727364034712963, 27.33667001641208572 ) ) ;
#2489 = CARTESIAN_POINT ( 'NONE',  ( 32.73300124599732186, 0.000000000000000000, 0.000000000000000000 ) ) ;
#2490 = EDGE_LOOP ( 'NONE', ( #12175, #4207, #10346, #10001 ) ) ;
#2491 = CARTESIAN_POINT ( 'NONE',  ( 2.430230287190592531, 145.5073573687466819, -1.451610819318251089 ) ) ;
#2492 = ADVANCED_FACE ( 'NONE', ( #21844 ), #24417, .F. ) ;
#2493 = VERTEX_POINT ( 'NONE', #2239 ) ;
#2494 = CARTESIAN_POINT ( 'NONE',  ( -8.786685647604890903, -23.24040270374424466, -48.22796981442760256 ) ) ;
#2495 = CARTESIAN_POINT ( 'NONE',  ( 2.263178113027049410, 141.9207360579561055, 31.59906256848331907 ) ) ;
#2496 = ORIENTED_EDGE ( 'NONE', *, *, #14089, .T. ) ;
#2497 = ORIENTED_EDGE ( 'NONE', *, *, #11941, .F. ) ;
#2498 = B_SPLINE_CURVE_WITH_KNOTS ( 'NONE', 3,
 ( #3002, #9346, #6896, #2853 ),
 .UNSPECIFIED., .F., .F.,
 ( 4, 4 ),
 ( 5.845992376248150641E-16, 0.008383748772660029602 ),
 .UNSPECIFIED. ) ;
#2499 = CARTESIAN_POINT ( 'NONE',  ( -20.57838717382308147, -27.96569011373093971, -10.78122205916989529 ) ) ;
#2500 = EDGE_CURVE ( 'NONE', #1301, #9661, #22172, .T. ) ;
#2501 = ORIENTED_EDGE ( 'NONE', *, *, #23556, .F. ) ;
#2502 = CARTESIAN_POINT ( 'NONE',  ( 1.833750490713699444, -96.89879583303773813, -108.0159692407140568 ) ) ;
#2503 = ORIENTED_EDGE ( 'NONE', *, *, #23561, .F. ) ;
#2504 =( BOUNDED_SURFACE ( )  B_SPLINE_SURFACE ( 3, 1, ( 
 ( #10194, #1798 ),
 ( #25454, #19368 ),
 ( #28141, #17208 ),
 ( #6287, #221 ) ),
 .UNSPECIFIED., .F., .F., .F. ) 
 B_SPLINE_SURFACE_WITH_KNOTS ( ( 4, 4 ),
 ( 2, 2 ),
 ( 0.000000000000000000, 1.000000000000000000 ),
 ( 0.000000000000000000, 1.000000000000000000 ),
 .UNSPECIFIED. ) 
 GEOMETRIC_REPRESENTATION_ITEM ( )  RATIONAL_B_SPLINE_SURFACE ( (
 ( 1.000000000000000000, 1.000000000000000000),
 ( 0.9934239774497837239, 0.8357310067453919133),
 ( 0.9934239774497837239, 0.8357310067453919133),
 ( 1.000000000000000000, 1.000000000000000000) ) ) 
 REPRESENTATION_ITEM ( '' )  SURFACE ( )  );
#2505 = CARTESIAN_POINT ( 'NONE',  ( 28.37603512858455446, 68.88140609180194929, 91.75440368549958237 ) ) ;
#2506 = CARTESIAN_POINT ( 'NONE',  ( 5.340103556456506695, -84.79482753886469482, -120.6284720803335091 ) ) ;
#2507 = CARTESIAN_POINT ( 'NONE',  ( -55.24340739397742084, -0.009842732675351817742, 0.002421372372454084262 ) ) ;
#2508 = CARTESIAN_POINT ( 'NONE',  ( -7.711401346138389457, 10.36923727626120773, -51.42722225669425740 ) ) ;
#2509 = CARTESIAN_POINT ( 'NONE',  ( 8.186469829614228644, -63.89871393833106339, 134.9918587494111648 ) ) ;
#2510 = CARTESIAN_POINT ( 'NONE',  ( -55.24271866751342941, 0.001425019990782615698, -0.009388511352197861579 ) ) ;
#2511 = CARTESIAN_POINT ( 'NONE',  ( 13.36082413113061307, -147.2768864064170486, 41.18148072373564617 ) ) ;
#2512 = CARTESIAN_POINT ( 'NONE',  ( 30.59138290137891047, -79.74792615266090934, -84.53179630244071063 ) ) ;
#2513 = CARTESIAN_POINT ( 'NONE',  ( -55.24271866751342941, 0.006757859501006707216, 0.006671293903669109175 ) ) ;
#2514 = EDGE_CURVE ( 'NONE', #24670, #4384, #18393, .T. ) ;
#2515 = ORIENTED_EDGE ( 'NONE', *, *, #26003, .T. ) ;
#2516 = CARTESIAN_POINT ( 'NONE',  ( -1.583189561560255143, -2.490696082059541627, 46.33203782964464068 ) ) ;
#2517 = CARTESIAN_POINT ( 'NONE',  ( 30.59138290137879679, -33.33271994911419256, 111.3296280985501596 ) ) ;
#2518 = EDGE_CURVE ( 'NONE', #24427, #1176, #4328, .T. ) ;
#2520 = CARTESIAN_POINT ( 'NONE',  ( -8.786685647604720373, -47.14957014837338534, -25.35688121747513435 ) ) ;
#2519 = CARTESIAN_POINT ( 'NONE',  ( -55.24340739397742794, 0.002421372372456844640, -0.009842732675349010960 ) ) ;
#2521 = B_SPLINE_CURVE_WITH_KNOTS ( 'NONE', 3,
 ( #12749, #21533, #1805, #10605, #25304, #14493, #23298, #18964 ),
 .UNSPECIFIED., .F., .F.,
 ( 4, 2, 2, 4 ),
 ( 0.000000000000000000, 0.0002429588503611183675, 0.0004859177007222367350, 0.0009718354014444859383 ),
 .UNSPECIFIED. ) ;
#2522 = CARTESIAN_POINT ( 'NONE',  ( -24.53237795827027412, -22.94498492516361310, -24.99972053297897290 ) ) ;
#2523 = CARTESIAN_POINT ( 'NONE',  ( 1.832998868059890096, -44.33343224355329681, 138.1720401012265427 ) ) ;
#2524 = CARTESIAN_POINT ( 'NONE',  ( -1.463510566862822770, 11.94877850058565727, 44.64091840826476698 ) ) ;
#2525 = ORIENTED_EDGE ( 'NONE', *, *, #9725, .F. ) ;
#2526 = FACE_OUTER_BOUND ( 'NONE', #25146, .T. ) ;
#2527 = ADVANCED_FACE ( 'NONE', ( #811 ), #10629, .F. ) ;
#2528 = CARTESIAN_POINT ( 'NONE',  ( 2.430230287190589422, -125.2872625092167596, 74.01081053031055035 ) ) ;
#2529 = CARTESIAN_POINT ( 'NONE',  ( 14.74894986621300319, -5.136656239696338858E-17, 37.50000000000001421 ) ) ;
#2530 = CARTESIAN_POINT ( 'NONE',  ( 26.28373643307407548, 71.57300207276523452, -105.5888781856744174 ) ) ;
#2531 = EDGE_LOOP ( 'NONE', ( #19992, #26224, #27993, #15738 ) ) ;
#2532 = CARTESIAN_POINT ( 'NONE',  ( 1.832998868059890096, -138.1720401012269974, 44.33343224355190415 ) ) ;
#2533 = EDGE_CURVE ( 'NONE', #6495, #27090, #24587, .T. ) ;
#2534 = CARTESIAN_POINT ( 'NONE',  ( 6.224689322667647851, -71.79702446228394308, 129.4863684118285221 ) ) ;
#2535 = LINE ( 'NONE', #4552, #19780 ) ;
#2536 = VERTEX_POINT ( 'NONE', #15428 ) ;
#2537 = ORIENTED_EDGE ( 'NONE', *, *, #12546, .T. ) ;
#2538 = CARTESIAN_POINT ( 'NONE',  ( 2.433796855181205476, 86.69855925934130880, -116.8607839509047892 ) ) ;
#2539 = CARTESIAN_POINT ( 'NONE',  ( 13.36082413113061307, -119.8836995922720092, -94.94363694444177781 ) ) ;
#2540 = ORIENTED_EDGE ( 'NONE', *, *, #25433, .T. ) ;
#2541 = CARTESIAN_POINT ( 'NONE',  ( -9.156249394959706578, 53.90509764945129945, 8.027840202794124025 ) ) ;
#2542 = CARTESIAN_POINT ( 'NONE',  ( -24.53239521893650377, -22.94500969220219488, 24.99972072650167476 ) ) ;
#2543 = CARTESIAN_POINT ( 'NONE',  ( 5.340103579038286696, 28.39990973304668032, -144.6887562507421876 ) ) ;
#2544 = CARTESIAN_POINT ( 'NONE',  ( 25.64681081121879203, 23.88203588908081443, 110.3564950173082480 ) ) ;
#2545 = CARTESIAN_POINT ( 'NONE',  ( 1.833603222531960952, -125.8904991419471884, 72.16916166673696864 ) ) ;
#2546 = EDGE_LOOP ( 'NONE', ( #11351, #14635, #21006, #5852 ) ) ;
#2547 = CIRCLE ( 'NONE', #17718, 44.74884827092600403 ) ;
#2548 = CARTESIAN_POINT ( 'NONE',  ( 2.433796855181205476, -132.3327394885227477, -60.50726454508036056 ) ) ;
#2549 = CARTESIAN_POINT ( 'NONE',  ( 5.340103579038244952, -62.06990748397762303, -133.7487108093470169 ) ) ;
#2550 = CARTESIAN_POINT ( 'NONE',  ( 25.64681081121879203, -97.99105938547884875, -56.09509703373446854 ) ) ;
#2551 = ORIENTED_EDGE ( 'NONE', *, *, #25140, .F. ) ;
#2552 = ORIENTED_EDGE ( 'NONE', *, *, #10951, .F. ) ;
#2553 = ORIENTED_EDGE ( 'NONE', *, *, #13372, .T. ) ;
#2554 = CARTESIAN_POINT ( 'NONE',  ( -1.045287976400379737, -25.66401692420040703, -37.92705037016734337 ) ) ;
#2555 =( REPRESENTATION_RELATIONSHIP ('NONE','NONE', #15430, #7571 ) REPRESENTATION_RELATIONSHIP_WITH_TRANSFORMATION ( #3540 )SHAPE_REPRESENTATION_RELATIONSHIP( ) );
#2556 = CARTESIAN_POINT ( 'NONE',  ( -1.031422197589711764, 45.78027046666443312, 1.530725436377622817 ) ) ;
#2557 = ADVANCED_FACE ( 'NONE', ( #6972, #22368 ), #28387, .T. ) ;
#2558 = CARTESIAN_POINT ( 'NONE',  ( -1.058197053496161555, -38.06270006878834522, 25.48582931365511328 ) ) ;
#2559 = CARTESIAN_POINT ( 'NONE',  ( 1.832998868059858122, -84.86110816369684073, 117.7096351258385027 ) ) ;
#2560 = CARTESIAN_POINT ( 'NONE',  ( 1.833838850093478579, 144.3148369740567318, 15.16809710532109712 ) ) ;
#2561 = CARTESIAN_POINT ( 'NONE',  ( -20.21097721712959583, -8.835581498567664838, -28.26295595852182529 ) ) ;
#2562 = CARTESIAN_POINT ( 'NONE',  ( 1.833485406944057594, 117.7091014914950193, 84.86072343962607079 ) ) ;
#2563 = VERTEX_POINT ( 'NONE', #24242 ) ;
#2564 = CARTESIAN_POINT ( 'NONE',  ( 26.11404676487257603, -84.89295829319442532, -74.91683232331061504 ) ) ;
#2565 = CARTESIAN_POINT ( 'NONE',  ( 109.1589550718174877, -0.007571935245604908930, -0.0002241941239241235554 ) ) ;
#2566 = CARTESIAN_POINT ( 'NONE',  ( 26.11404676487259024, -112.4785329405482912, 12.95861723607416671 ) ) ;
#2567 = CARTESIAN_POINT ( 'NONE',  ( 109.1587776205901861, 0.001442274044995796702, -0.007186028091168164718 ) ) ;
#2568 = EDGE_CURVE ( 'NONE', #27540, #24434, #24947, .T. ) ;
#2569 = CARTESIAN_POINT ( 'NONE',  ( 55.79472521941426777, -66.75682020267549888, 28.92526238350451351 ) ) ;
#2570 = ADVANCED_FACE ( 'NONE', ( #15723 ), #5461, .T. ) ;
#2571 = ORIENTED_EDGE ( 'NONE', *, *, #24124, .T. ) ;
#2572 = CARTESIAN_POINT ( 'NONE',  ( 2.430230287190592531, 142.6294793592097960, 28.83279105684475851 ) ) ;
#2573 = VERTEX_POINT ( 'NONE', #22062 ) ;
#2574 = CARTESIAN_POINT ( 'NONE',  ( -8.786685647604887350, 53.04920435127183254, 7.199674155859139724 ) ) ;
#2575 = B_SPLINE_CURVE_WITH_KNOTS ( 'NONE', 3,
 ( #20845, #10352, #25312, #16524, #19114, #10058 ),
 .UNSPECIFIED., .F., .F.,
 ( 4, 2, 4 ),
 ( 1.389302603484999005E-17, 0.0006311571484586086080, 0.001262314296917203555 ),
 .UNSPECIFIED. ) ;
#2576 = CARTESIAN_POINT ( 'NONE',  ( 1.833485406944057594, -142.0485807715644171, -29.64752363041688454 ) ) ;
#2577 = VERTEX_POINT ( 'NONE', #4367 ) ;
#2578 = B_SPLINE_CURVE_WITH_KNOTS ( 'NONE', 3,
 ( #789, #5102, #13880, #2958, #16184, #6851 ),
 .UNSPECIFIED., .F., .F.,
 ( 4, 2, 4 ),
 ( 3.689388176052398149E-16, 0.003576372551511164399, 0.007152745103021965374 ),
 .UNSPECIFIED. ) ;
#2579 = ORIENTED_EDGE ( 'NONE', *, *, #10709, .T. ) ;
#2580 = VERTEX_POINT ( 'NONE', #325 ) ;
#2581 = CARTESIAN_POINT ( 'NONE',  ( -20.20700224038492721, -18.19058640100206503, 23.35150625415678860 ) ) ;
#2582 = FACE_OUTER_BOUND ( 'NONE', #23599, .T. ) ;
#2583 = CARTESIAN_POINT ( 'NONE',  ( -20.47566338032525124, 16.24827550219824701, -25.06314818626695740 ) ) ;
#2584 =( BOUNDED_SURFACE ( )  B_SPLINE_SURFACE ( 3, 1, ( 
 ( #14917, #21403 ),
 ( #10477, #3981 ),
 ( #18971, #19378 ),
 ( #21111, #10350 ) ),
 .UNSPECIFIED., .F., .F., .F. ) 
 B_SPLINE_SURFACE_WITH_KNOTS ( ( 4, 4 ),
 ( 2, 2 ),
 ( 0.000000000000000000, 1.000000000000000000 ),
 ( 0.000000000000000000, 1.000000000000000000 ),
 .UNSPECIFIED. ) 
 GEOMETRIC_REPRESENTATION_ITEM ( )  RATIONAL_B_SPLINE_SURFACE ( (
 ( 1.000000000000000000, 1.000000000000000000),
 ( 0.6386103224230302855, 0.9954351624131538845),
 ( 0.6386103224230302855, 0.9954351624131538845),
 ( 1.000000000000000000, 1.000000000000000000) ) ) 
 REPRESENTATION_ITEM ( '' )  SURFACE ( )  );
#2585 = B_SPLINE_CURVE_WITH_KNOTS ( 'NONE', 3,
 ( #22186, #17425, #11, #28362, #12972, #4338, #2454, #6508, #2028, #4471 ),
 .UNSPECIFIED., .F., .F.,
 ( 4, 2, 2, 2, 4 ),
 ( 0.000000000000000000, 0.0003346267210630928380, 0.0006692534421261856761, 0.001003880163189278460, 0.001338506884252371352 ),
 .UNSPECIFIED. ) ;
#2586 = CARTESIAN_POINT ( 'NONE',  ( 10.93730112726007775, 51.37919228020501805, -142.1801301103781725 ) ) ;
#2587 = ORIENTED_EDGE ( 'NONE', *, *, #7537, .F. ) ;
#2588 = CARTESIAN_POINT ( 'NONE',  ( 10.93730112725990367, -92.80059208661606363, -119.3442956573281748 ) ) ;
#2589 = ORIENTED_EDGE ( 'NONE', *, *, #11086, .F. ) ;
#2590 = CARTESIAN_POINT ( 'NONE',  ( 25.69398547355838502, 91.80679989327151702, 65.78402800526194483 ) ) ;
#2591 = EDGE_LOOP ( 'NONE', ( #22277, #4233, #1204, #9913 ) ) ;
#2592 = CARTESIAN_POINT ( 'NONE',  ( -55.25719721206881729, 0.01041086141212550775, -0.004044147484878501606 ) ) ;
#2593 = CARTESIAN_POINT ( 'NONE',  ( -1.049817751779871688, -37.35030165458155693, 26.50542916749608580 ) ) ;
#2594 = EDGE_CURVE ( 'NONE', #19089, #5993, #11871, .T. ) ;
#2595 = CARTESIAN_POINT ( 'NONE',  ( -8.259864102781634188, -6.590267880897305197, -52.60025989855206063 ) ) ;
#2596 = CARTESIAN_POINT ( 'NONE',  ( 16.75465622695657331, 25.01894884133855612, 140.0080030360327896 ) ) ;
#2597 = CARTESIAN_POINT ( 'NONE',  ( 109.1592201516379674, -0.001934867487012880598, 0.007620268632968135725 ) ) ;
#2598 =( BOUNDED_SURFACE ( )  B_SPLINE_SURFACE ( 3, 1, ( 
 ( #26107, #12720 ),
 ( #10860, #19345 ),
 ( #25839, #25975 ),
 ( #26244, #21933 ) ),
 .UNSPECIFIED., .F., .F., .F. ) 
 B_SPLINE_SURFACE_WITH_KNOTS ( ( 4, 4 ),
 ( 2, 2 ),
 ( 0.000000000000000000, 1.000000000000000000 ),
 ( 0.000000000000000000, 1.000000000000000000 ),
 .UNSPECIFIED. ) 
 GEOMETRIC_REPRESENTATION_ITEM ( )  RATIONAL_B_SPLINE_SURFACE ( (
 ( 1.000000000000000000, 1.000000000000000000),
 ( 0.9593753223639863714, 0.9995975284513187731),
 ( 0.9593753223639863714, 0.9995975284513187731),
 ( 1.000000000000000000, 1.000000000000000000) ) ) 
 REPRESENTATION_ITEM ( '' )  SURFACE ( )  );
#2599 = CARTESIAN_POINT ( 'NONE',  ( -4.473127245936434626, 3.196405119334491562, 49.22197550883364414 ) ) ;
#2600 = CARTESIAN_POINT ( 'NONE',  ( -8.786685647604887350, -25.35688121747534751, -47.14957014837345639 ) ) ;
#2601 = ADVANCED_FACE ( 'NONE', ( #17448 ), #19450, .F. ) ;
#2602 = EDGE_CURVE ( 'NONE', #23301, #11627, #22915, .T. ) ;
#2603 = CARTESIAN_POINT ( 'NONE',  ( 10.93730112726002979, 92.80059208661855052, -119.3442956573263558 ) ) ;
#2604 = CARTESIAN_POINT ( 'NONE',  ( 25.64681081121879203, -66.03065707438874199, -91.59071981940638807 ) ) ;
#2605 = CARTESIAN_POINT ( 'NONE',  ( -55.24271866751342941, 0.008488649505343330570, 0.004256484107795472684 ) ) ;
#2606 = CARTESIAN_POINT ( 'NONE',  ( -1.058473599757810746, 38.06357893967467731, 25.48501014712358881 ) ) ;
#2607 = ORIENTED_EDGE ( 'NONE', *, *, #10395, .F. ) ;
#2608 = ORIENTED_EDGE ( 'NONE', *, *, #27061, .F. ) ;
#2609 = CARTESIAN_POINT ( 'NONE',  ( 26.11404676487259024, 24.64483677384848903, 110.5078194225162207 ) ) ;
#2610 = CARTESIAN_POINT ( 'NONE',  ( 1.832998868059890096, -117.7096351258381901, -84.86110816369725285 ) ) ;
#2611 = VERTEX_POINT ( 'NONE', #26382 ) ;
#2612 = B_SPLINE_CURVE_WITH_KNOTS ( 'NONE', 3,
 ( #6426, #15042, #17490, #19371 ),
 .UNSPECIFIED., .F., .F.,
 ( 4, 4 ),
 ( 0.000000000000000000, 0.01077107196513815181 ),
 .UNSPECIFIED. ) ;
#2613 = ORIENTED_EDGE ( 'NONE', *, *, #7561, .T. ) ;
#2614 = EDGE_LOOP ( 'NONE', ( #22494, #19497, #25440, #28061 ) ) ;
#2615 = CARTESIAN_POINT ( 'NONE',  ( -1.044556982611269502, 25.56989963842203650, -37.98985389331818396 ) ) ;
#2616 = B_SPLINE_CURVE_WITH_KNOTS ( 'NONE', 3,
 ( #12303, #18500, #18935, #27711 ),
 .UNSPECIFIED., .F., .F.,
 ( 4, 4 ),
 ( 4.887365971079175436E-16, 0.008383748772659961948 ),
 .UNSPECIFIED. ) ;
#2617 = CARTESIAN_POINT ( 'NONE',  ( 9.884929003653626367, 124.2095058357577670, 85.04731144912555862 ) ) ;
#2618 = DIRECTION ( 'NONE',  ( 0.7071067811865485719, 4.906538933386790339E-16, 0.7071067811865465735 ) ) ;
#2619 = EDGE_CURVE ( 'NONE', #23901, #10557, #24104, .T. ) ;
#2620 = CARTESIAN_POINT ( 'NONE',  ( -55.24340739397742794, -0.009842732675348539115, -0.002421372372456522849 ) ) ;
#2621 = ORIENTED_EDGE ( 'NONE', *, *, #14464, .T. ) ;
#2622 = CARTESIAN_POINT ( 'NONE',  ( 32.73300124599732186, 0.000000000000000000, 0.000000000000000000 ) ) ;
#2623 = B_SPLINE_CURVE_WITH_KNOTS ( 'NONE', 3,
 ( #2989, #11905, #9603, #18364, #15317, #6418, #23856, #13451, #19782, #6564 ),
 .UNSPECIFIED., .F., .F.,
 ( 4, 2, 2, 2, 4 ),
 ( 8.420559318810145779E-18, 0.0003346267210630978796, 0.0006692534421261874108, 0.001003880163189276942, 0.001338506884252366365 ),
 .UNSPECIFIED. ) ;
#2624 = B_SPLINE_CURVE_WITH_KNOTS ( 'NONE', 3,
 ( #621, #16007, #7544, #24818, #25096, #16156 ),
 .UNSPECIFIED., .F., .F.,
 ( 4, 2, 4 ),
 ( 2.684971462552800574E-17, 0.0006311636237756952823, 0.001262327247551372567 ),
 .UNSPECIFIED. ) ;
#2625 = CARTESIAN_POINT ( 'NONE',  ( -21.41427618760447871, 29.81030852927067443, -7.777551129310157130 ) ) ;
#2626 = CARTESIAN_POINT ( 'NONE',  ( 9.884929003653608603, 11.54837932063031047, 150.0922431698405717 ) ) ;
#2627 = EDGE_CURVE ( 'NONE', #11607, #19219, #27684, .T. ) ;
#2628 = EDGE_CURVE ( 'NONE', #4784, #17963, #21543, .T. ) ;
#2629 = CARTESIAN_POINT ( 'NONE',  ( 16.05277956358197144, 134.7758735858410830, -48.70400867628961095 ) ) ;
#2630 = CARTESIAN_POINT ( 'NONE',  ( 109.1586900883932856, 0.002810909342002405019, -0.006561743627145274170 ) ) ;
#2631 = CARTESIAN_POINT ( 'NONE',  ( -4.162674018437150458, -3.424137510344606117, 48.79210541969628423 ) ) ;
#2632 =( BOUNDED_SURFACE ( )  B_SPLINE_SURFACE ( 3, 1, ( 
 ( #18330, #14023 ),
 ( #22835, #24414 ),
 ( #4686, #9722 ),
 ( #21222, #27265 ) ),
 .UNSPECIFIED., .F., .F., .F. ) 
 B_SPLINE_SURFACE_WITH_KNOTS ( ( 4, 4 ),
 ( 2, 2 ),
 ( 0.000000000000000000, 1.000000000000000000 ),
 ( 0.000000000000000000, 1.000000000000000000 ),
 .UNSPECIFIED. ) 
 GEOMETRIC_REPRESENTATION_ITEM ( )  RATIONAL_B_SPLINE_SURFACE ( (
 ( 1.000000000000000000, 1.000000000000000000),
 ( 0.7789835883360578528, 0.9689951854195403280),
 ( 0.7789835883360578528, 0.9689951854195403280),
 ( 1.000000000000000000, 1.000000000000000000) ) ) 
 REPRESENTATION_ITEM ( '' )  SURFACE ( )  );
#2633 = EDGE_LOOP ( 'NONE', ( #13746, #22279, #11686, #21522 ) ) ;
#2635 = CARTESIAN_POINT ( 'NONE',  ( -9.156249394959706578, 48.32878616081010392, -25.18996226954632078 ) ) ;
#2634 = CARTESIAN_POINT ( 'NONE',  ( -9.156249394959713683, 53.74753343182715781, 9.022661520477214481 ) ) ;
#2636 = CARTESIAN_POINT ( 'NONE',  ( 1.833485406944043827, -144.2578170162061895, -15.69895494453532869 ) ) ;
#2637 = CARTESIAN_POINT ( 'NONE',  ( 25.64708228042119487, 45.88917180166276921, 103.1656011680034055 ) ) ;
#2638 = CARTESIAN_POINT ( 'NONE',  ( 2.430230287190589422, 84.35270093935415048, -118.5711603495673074 ) ) ;
#2639 = CARTESIAN_POINT ( 'NONE',  ( -1.619063947482197729, -29.22875152547781852, -35.99532424477369830 ) ) ;
#2640 = ORIENTED_EDGE ( 'NONE', *, *, #25373, .F. ) ;
#2641 = CARTESIAN_POINT ( 'NONE',  ( -20.20700224038492010, -0.9908225410476447781, 29.58392382092673500 ) ) ;
#2642 = ORIENTED_EDGE ( 'NONE', *, *, #13129, .F. ) ;
#2643 = CARTESIAN_POINT ( 'NONE',  ( -2.911734481061404534, -17.36785190846011417, -44.38410240830297226 ) ) ;
#2644 = B_SPLINE_CURVE_WITH_KNOTS ( 'NONE', 3,
 ( #4743, #24060, #278, #24193, #22313, #20277, #141, #4886, #15382, #8936 ),
 .UNSPECIFIED., .F., .F.,
 ( 4, 3, 3, 4 ),
 ( 0.000000000000000000, 0.0002669560319015610878, 0.0005492286108966271422, 0.0008315040496093543303 ),
 .UNSPECIFIED. ) ;
#2645 = CARTESIAN_POINT ( 'NONE',  ( 2.433796855181233454, 137.9325382748291418, -46.34326152018600453 ) ) ;
#2646 = VERTEX_POINT ( 'NONE', #624 ) ;
#2647 = CARTESIAN_POINT ( 'NONE',  ( 19.66333377628682655, 121.4767361208146639, -64.94841092372071500 ) ) ;
#2648 = EDGE_LOOP ( 'NONE', ( #21089, #21586, #19739, #6640 ) ) ;
#2649 = CARTESIAN_POINT ( 'NONE',  ( 2.430230287190581429, -96.28466919684025527, -109.1043569252024099 ) ) ;
#2650 = EDGE_LOOP ( 'NONE', ( #16941, #6061, #26086, #4322 ) ) ;
#2651 = B_SPLINE_CURVE_WITH_KNOTS ( 'NONE', 3,
 ( #2001, #8365, #10390, #6338, #12941, #15230, #25778 ),
 .UNSPECIFIED., .F., .F.,
 ( 4, 3, 4 ),
 ( 0.000000000000000000, 0.02398743853561338332, 0.04000277880656213231 ),
 .UNSPECIFIED. ) ;
#2652 = ADVANCED_FACE ( 'NONE', ( #18612 ), #18798, .T. ) ;
#2653 = CARTESIAN_POINT ( 'NONE',  ( -1.048172774974294175, 37.64158596421250991, 26.08722459372745206 ) ) ;
#2654 = EDGE_CURVE ( 'NONE', #25436, #18316, #7104, .T. ) ;
#2655 = CARTESIAN_POINT ( 'NONE',  ( -1.048996300304498419, -14.87787369922200043, -43.31387123529974303 ) ) ;
#2656 = CARTESIAN_POINT ( 'NONE',  ( 1.833838850855462166, 30.08297881069679391, 141.9572669680996739 ) ) ;
#2657 = AXIS2_PLACEMENT_3D ( 'NONE', #5788, #1591, #19428 ) ;
#2658 = EDGE_CURVE ( 'NONE', #18577, #2563, #22539, .T. ) ;
#2659 = CARTESIAN_POINT ( 'NONE',  ( 1.834118845439484335, 138.0627591860436212, -44.67218053242251585 ) ) ;
#2660 = CARTESIAN_POINT ( 'NONE',  ( -20.57838717382308502, 27.96569011373086866, -10.78122205917010135 ) ) ;
#2661 = B_SPLINE_CURVE_WITH_KNOTS ( 'NONE', 3,
 ( #6330, #2700, #258, #26584 ),
 .UNSPECIFIED., .F., .F.,
 ( 4, 4 ),
 ( 1.904175111373004964E-16, 0.001982023823822943748 ),
 .UNSPECIFIED. ) ;
#2662 = CARTESIAN_POINT ( 'NONE',  ( 94.22246935314088034, -90.00000000000005684, -6.938893903907228378E-15 ) ) ;
#2663 = CARTESIAN_POINT ( 'NONE',  ( 109.1778270068192853, 0.005967275455169884606, 0.007152128381194073486 ) ) ;
#2664 = DIRECTION ( 'NONE',  ( 0.000000000000000000, 0.000000000000000000, 1.000000000000000000 ) ) ;
#2665 = DIRECTION ( 'NONE',  ( -1.000000000000000000, -0.000000000000000000, -0.000000000000000000 ) ) ;
#2666 = CARTESIAN_POINT ( 'NONE',  ( -1.048994561756789734, -27.53485040342867407, 36.59609844253159139 ) ) ;
#2667 = CARTESIAN_POINT ( 'NONE',  ( 30.59138290137885718, -109.6600423140543228, 38.47117663195916037 ) ) ;
#2668 = CARTESIAN_POINT ( 'NONE',  ( -1.619063947482201282, 43.26576862488434472, -16.67502769180576649 ) ) ;
#2669 = ORIENTED_EDGE ( 'NONE', *, *, #11224, .F. ) ;
#2670 = CARTESIAN_POINT ( 'NONE',  ( 25.64681081121879203, 23.06870491922322230, 110.5293738517609228 ) ) ;
#2671 = CARTESIAN_POINT ( 'NONE',  ( 1.834118845439484335, 145.1099497418795750, 0.1779704863075100008 ) ) ;
#2672 = CARTESIAN_POINT ( 'NONE',  ( -4.473127245936431073, 45.82513704981569447, 18.25038884639822712 ) ) ;
#2673 = ORIENTED_EDGE ( 'NONE', *, *, #375, .F. ) ;
#2674 = CARTESIAN_POINT ( 'NONE',  ( 25.64703792032472052, 75.44170528134999643, -84.00887408968974057 ) ) ;
#2675 = ORIENTED_EDGE ( 'NONE', *, *, #7491, .F. ) ;
#2676 = CARTESIAN_POINT ( 'NONE',  ( -1.539760825549692402, -16.63252404870386059, -43.19716078875433851 ) ) ;
#2677 = VECTOR ( 'NONE', #16786, 1000.000000000000114 ) ;
#2678 =( BOUNDED_SURFACE ( )  B_SPLINE_SURFACE ( 3, 1, ( 
 ( #17697, #17143 ),
 ( #26477, #6224 ),
 ( #15105, #14976 ),
 ( #21601, #8516 ) ),
 .UNSPECIFIED., .F., .F., .F. ) 
 B_SPLINE_SURFACE_WITH_KNOTS ( ( 4, 4 ),
 ( 2, 2 ),
 ( 0.000000000000000000, 1.000000000000000000 ),
 ( 0.000000000000000000, 1.000000000000000000 ),
 .UNSPECIFIED. ) 
 GEOMETRIC_REPRESENTATION_ITEM ( )  RATIONAL_B_SPLINE_SURFACE ( (
 ( 1.000000000000000000, 1.000000000000000000),
 ( 0.9960225298536222738, 0.9999952330161893110),
 ( 0.9960225298536222738, 0.9999952330161893110),
 ( 1.000000000000000000, 1.000000000000000000) ) ) 
 REPRESENTATION_ITEM ( '' )  SURFACE ( )  );
#2679 = CARTESIAN_POINT ( 'NONE',  ( 32.73300124599735028, 8.473903470906103408, 117.3295799645430151 ) ) ;
#2680 = CARTESIAN_POINT ( 'NONE',  ( -1.463510566862831430, 46.14841196428341163, 2.430838777910348192 ) ) ;
#2681 = B_SPLINE_CURVE_WITH_KNOTS ( 'NONE', 3,
 ( #10190, #8037, #22092, #13029 ),
 .UNSPECIFIED., .F., .F.,
 ( 4, 4 ),
 ( 8.993834424997155211E-17, 0.008383748772659552553 ),
 .UNSPECIFIED. ) ;
#2682 = EDGE_LOOP ( 'NONE', ( #11533, #19060, #3372, #482 ) ) ;
#2683 = CARTESIAN_POINT ( 'NONE',  ( 9.884929003653608603, 85.04731144912511809, 124.2095058357580513 ) ) ;
#2684 = EDGE_CURVE ( 'NONE', #27364, #10661, #25389, .T. ) ;
#2685 = VERTEX_POINT ( 'NONE', #27528 ) ;
#2686 = CARTESIAN_POINT ( 'NONE',  ( 109.1586059443104944, -0.006570129623063787269, -0.002622205828279724604 ) ) ;
#2687 = EDGE_CURVE ( 'NONE', #11364, #12467, #10510, .T. ) ;
#2688 = ORIENTED_EDGE ( 'NONE', *, *, #24702, .F. ) ;
#2689 = FACE_OUTER_BOUND ( 'NONE', #28127, .T. ) ;
#2690 = CARTESIAN_POINT ( 'NONE',  ( 26.28373643307398666, -97.52903534490815218, -82.21796085350759142 ) ) ;
#2691 = EDGE_CURVE ( 'NONE', #24160, #8435, #7391, .T. ) ;
#2692 = CARTESIAN_POINT ( 'NONE',  ( -20.21097721650785672, -17.67178726257375487, -23.76068422213751674 ) ) ;
#2693 = CARTESIAN_POINT ( 'NONE',  ( 32.73300124599737160, -113.0038235389604466, 32.68291970228198551 ) ) ;
#2694 = B_SPLINE_CURVE_WITH_KNOTS ( 'NONE', 3,
 ( #2139, #7206, #4742, #9065, #4450, #17690 ),
 .UNSPECIFIED., .F., .F.,
 ( 4, 2, 4 ),
 ( 0.000000000000000000, 0.0004335184443140234316, 0.0008670368886280468632 ),
 .UNSPECIFIED. ) ;
#2695 = CARTESIAN_POINT ( 'NONE',  ( -1.044557008772713180, 15.70482370518816495, -43.01636061108991527 ) ) ;
#2696 = CARTESIAN_POINT ( 'NONE',  ( -55.24728320129491266, 0.01214321324517175435, -0.008013189884952098135 ) ) ;
#2697 = ORIENTED_EDGE ( 'NONE', *, *, #18312, .F. ) ;
#2698 = EDGE_CURVE ( 'NONE', #20693, #4272, #16495, .T. ) ;
#2699 = CARTESIAN_POINT ( 'NONE',  ( -4.473127245936434626, -41.70021447285072469, -26.34600523034523434 ) ) ;
#2700 = CARTESIAN_POINT ( 'NONE',  ( -20.21097721712958872, 29.61001327235739566, 0.3305963429843793433 ) ) ;
#2701 = CARTESIAN_POINT ( 'NONE',  ( 26.11404676487259024, -1.130420376096339385, -113.2169081140374232 ) ) ;
#2702 = EDGE_LOOP ( 'NONE', ( #15664, #5473, #1063, #23629 ) ) ;
#2703 = ORIENTED_EDGE ( 'NONE', *, *, #18737, .F. ) ;
#2704 = ORIENTED_EDGE ( 'NONE', *, *, #5469, .F. ) ;
#2705 = DIRECTION ( 'NONE',  ( 0.5946245182733608248, -0.7332888028688925308, -0.3297108033645242964 ) ) ;
#2706 = CARTESIAN_POINT ( 'NONE',  ( -1.619063947482201282, 44.80407745103784123, -11.94059994246174838 ) ) ;
#2707 = CARTESIAN_POINT ( 'NONE',  ( -55.25297051322618813, -0.01466904165775489814, 0.002853887643043841529 ) ) ;
#2708 = B_SPLINE_CURVE_WITH_KNOTS ( 'NONE', 3,
 ( #25315, #18384, #7626, #5593, #5155, #3290, #12073, #20848, #24756, #18239 ),
 .UNSPECIFIED., .F., .F.,
 ( 4, 3, 3, 4 ),
 ( 3.925231146709437917E-17, 0.0002669559177086447345, 0.0005339118354151110900, 0.001067817517169167285 ),
 .UNSPECIFIED. ) ;
#2709 = CARTESIAN_POINT ( 'NONE',  ( -1.619063947482197729, 46.30105812165548684, 2.489035965910320503 ) ) ;
#2710 = CARTESIAN_POINT ( 'NONE',  ( 25.70243777736190438, -103.4793210720851278, 45.26941207740255635 ) ) ;
#2711 = DIRECTION ( 'NONE',  ( -0.5914120900931443270, 0.6570486713847245586, 0.4674599267565369143 ) ) ;
#2712 = VERTEX_POINT ( 'NONE', #9990 ) ;
#2713 = CARTESIAN_POINT ( 'NONE',  ( 13.36082413113063083, 137.0038452127809876, -67.94366799842680393 ) ) ;
#2714 = CARTESIAN_POINT ( 'NONE',  ( -1.113427685307007531, -16.03057832159182539, -42.96952363574826705 ) ) ;
#2715 = CARTESIAN_POINT ( 'NONE',  ( 2.263178113027053406, -57.85473702513782257, -133.3897502891100260 ) ) ;
#2716 = CARTESIAN_POINT ( 'NONE',  ( 2.063896406836605024, -73.79559738457841434, 125.1295119249436851 ) ) ;
#2717 = DIRECTION ( 'NONE',  ( -1.000000000000000000, -0.000000000000000000, -0.000000000000000000 ) ) ;
#2718 = ORIENTED_EDGE ( 'NONE', *, *, #10921, .F. ) ;
#2719 = CARTESIAN_POINT ( 'NONE',  ( 2.430230287190592531, -31.67257033707400993, -142.0258656395025412 ) ) ;
#2720 = EDGE_CURVE ( 'NONE', #28456, #14178, #2957, .T. ) ;
#2721 =( BOUNDED_SURFACE ( )  B_SPLINE_SURFACE ( 3, 1, ( 
 ( #19960, #240 ),
 ( #19538, #24020 ),
 ( #26568, #2534 ),
 ( #13475, #22272 ) ),
 .UNSPECIFIED., .F., .F., .F. ) 
 B_SPLINE_SURFACE_WITH_KNOTS ( ( 4, 4 ),
 ( 2, 2 ),
 ( 0.000000000000000000, 1.000000000000000000 ),
 ( 0.000000000000000000, 1.000000000000000000 ),
 .UNSPECIFIED. ) 
 GEOMETRIC_REPRESENTATION_ITEM ( )  RATIONAL_B_SPLINE_SURFACE ( (
 ( 1.000000000000000000, 1.000000000000000000),
 ( 0.6386103224230316178, 0.9954351624131538845),
 ( 0.6386103224230316178, 0.9954351624131538845),
 ( 1.000000000000000000, 1.000000000000000000) ) ) 
 REPRESENTATION_ITEM ( '' )  SURFACE ( )  );
#2722 = ORIENTED_EDGE ( 'NONE', *, *, #1908, .T. ) ;
#2723 = CARTESIAN_POINT ( 'NONE',  ( 1.833485406944043827, 142.0485807715649571, -29.64752363041402816 ) ) ;
#2724 = CARTESIAN_POINT ( 'NONE',  ( -25.21435515916025594, 34.29329011225976842, -4.655591116594504086 ) ) ;
#2725 = VERTEX_POINT ( 'NONE', #11708 ) ;
#2726 = VERTEX_POINT ( 'NONE', #18166 ) ;
#2727 = ORIENTED_EDGE ( 'NONE', *, *, #25925, .T. ) ;
#2728 = EDGE_CURVE ( 'NONE', #3474, #2611, #22806, .T. ) ;
#2729 = CARTESIAN_POINT ( 'NONE',  ( -55.24728320129491266, -0.009072670231977940022, 0.01137345571547076703 ) ) ;
#2730 = CARTESIAN_POINT ( 'NONE',  ( -22.23226125620929494, -30.68305173820431619, -7.677408153693907167 ) ) ;
#2731 = EDGE_CURVE ( 'NONE', #15244, #7653, #16011, .T. ) ;
#2732 = CARTESIAN_POINT ( 'NONE',  ( 2.108985857320909485, 57.92316197981838144, -133.2480631238187243 ) ) ;
#2733 = CARTESIAN_POINT ( 'NONE',  ( -20.24399999263414429, 23.20123049637393464, 18.44171895251370330 ) ) ;
#2734 = VERTEX_POINT ( 'NONE', #20480 ) ;
#2735 = CARTESIAN_POINT ( 'NONE',  ( 1.833206310202337042, 14.42724831649545081, -144.3905118062892257 ) ) ;
#2736 = CARTESIAN_POINT ( 'NONE',  ( -1.045287976400362417, 43.05558670614268379, 15.59869763335023229 ) ) ;
#2737 = CARTESIAN_POINT ( 'NONE',  ( -1.050229599974474404, -0.2556477501656316820, 45.79907399707867199 ) ) ;
#2738 = ORIENTED_EDGE ( 'NONE', *, *, #16014, .F. ) ;
#2739 = EDGE_LOOP ( 'NONE', ( #25148, #23733, #13608, #12334 ) ) ;
#2740 = CARTESIAN_POINT ( 'NONE',  ( -55.25297051322618813, -0.01466904165775103838, -0.002853887643042541354 ) ) ;
#2741 = CARTESIAN_POINT ( 'NONE',  ( -1.045287976400365970, -36.12803364096568259, 28.14015102489869591 ) ) ;
#2742 = CARTESIAN_POINT ( 'NONE',  ( 25.64681081121879203, 112.3352186517030731, 11.38886654529711961 ) ) ;
#2743 = ADVANCED_BREP_SHAPE_REPRESENTATION ( '', ( #17192, #27263 ), #2919 ) ;
#2744 = CARTESIAN_POINT ( 'NONE',  ( 10.93730112725932635, 0.000000000000000000, 0.000000000000000000 ) ) ;
#2745 = CARTESIAN_POINT ( 'NONE',  ( -4.473127245936431073, -49.22197550883370809, -3.196405119333634470 ) ) ;
#2746 = B_SPLINE_CURVE_WITH_KNOTS ( 'NONE', 3,
 ( #946, #22991, #18206, #25009 ),
 .UNSPECIFIED., .F., .F.,
 ( 4, 4 ),
 ( 0.000000000000000000, 0.01077107196513849528 ),
 .UNSPECIFIED. ) ;
#2747 = CARTESIAN_POINT ( 'NONE',  ( -1.239374126674604337, 42.99367564261279995, -16.50008610789313934 ) ) ;
#2748 = DIRECTION ( 'NONE',  ( 0.000000000000000000, 0.000000000000000000, 1.000000000000000000 ) ) ;
#2749 = CARTESIAN_POINT ( 'NONE',  ( -20.20700224038492010, -10.08426345511570332, 27.82980252387829623 ) ) ;
#2750 = CARTESIAN_POINT ( 'NONE',  ( -1.113548883309562587, 44.18588492042589166, -12.28732181966532622 ) ) ;
#2751 = DIRECTION ( 'NONE',  ( 0.5914120900931443270, 0.5335794202785180129, 0.6045864222316765790 ) ) ;
#2752 = ORIENTED_EDGE ( 'NONE', *, *, #15285, .T. ) ;
#2753 = CARTESIAN_POINT ( 'NONE',  ( -1.044556982611280604, 44.03203163107544071, 12.57890920527730394 ) ) ;
#2754 = CARTESIAN_POINT ( 'NONE',  ( -55.24340739397742794, -0.0007387096945702591004, -0.01010924026184094153 ) ) ;
#2755 = ORIENTED_EDGE ( 'NONE', *, *, #9123, .T. ) ;
#2756 = ORIENTED_EDGE ( 'NONE', *, *, #19898, .F. ) ;
#2757 = ORIENTED_EDGE ( 'NONE', *, *, #20662, .F. ) ;
#2758 = CARTESIAN_POINT ( 'NONE',  ( -1.056502255334265339, 13.66916755949911177, 43.72121397317208391 ) ) ;
#2759 = ADVANCED_FACE ( 'NONE', ( #21041 ), #13556, .F. ) ;
#2760 = AXIS2_PLACEMENT_3D ( 'NONE', #1104, #16066, #20387 ) ;
#2761 = B_SPLINE_CURVE_WITH_KNOTS ( 'NONE', 3,
 ( #18895, #25531, #21187, #1612, #25235, #27815, #14568, #23373, #10413, #16447 ),
 .UNSPECIFIED., .F., .F.,
 ( 4, 2, 2, 2, 4 ),
 ( 1.371419323662773916E-18, 0.0003346267210630953859, 0.0006692534421261894708, 0.001003880163189283447, 0.001338506884252376773 ),
 .UNSPECIFIED. ) ;
#2762 = CARTESIAN_POINT ( 'NONE',  ( 1.832998868059858122, 125.4013017422241063, -73.01698022778225550 ) ) ;
#2763 = CARTESIAN_POINT ( 'NONE',  ( -55.24198130335446422, 0.008252882783649323831, 0.004276389980779915848 ) ) ;
#2764 = EDGE_CURVE ( 'NONE', #18334, #12354, #5352, .T. ) ;
#2765 = DIRECTION ( 'NONE',  ( -0.7071067811865485719, 0.000000000000000000, 0.7071067811865465735 ) ) ;
#2766 = EDGE_CURVE ( 'NONE', #18662, #21864, #15615, .T. ) ;
#2767 = CARTESIAN_POINT ( 'NONE',  ( 32.73300124599732186, 0.000000000000000000, 0.000000000000000000 ) ) ;
#2768 =( BOUNDED_SURFACE ( )  B_SPLINE_SURFACE ( 3, 1, ( 
 ( #2178, #19748 ),
 ( #6677, #185 ),
 ( #24678, #8973 ),
 ( #18013, #26801 ) ),
 .UNSPECIFIED., .F., .F., .F. ) 
 B_SPLINE_SURFACE_WITH_KNOTS ( ( 4, 4 ),
 ( 2, 2 ),
 ( 0.000000000000000000, 1.000000000000000000 ),
 ( 0.000000000000000000, 1.000000000000000000 ),
 .UNSPECIFIED. ) 
 GEOMETRIC_REPRESENTATION_ITEM ( )  RATIONAL_B_SPLINE_SURFACE ( (
 ( 1.000000000000000000, 1.000000000000000000),
 ( 0.9956975270656955868, 0.8568959468854907557),
 ( 0.9956975270656955868, 0.8568959468854907557),
 ( 1.000000000000000000, 1.000000000000000000) ) ) 
 REPRESENTATION_ITEM ( '' )  SURFACE ( )  );
#2769 = CARTESIAN_POINT ( 'NONE',  ( 32.73300124599732186, 0.000000000000000000, 0.000000000000000000 ) ) ;
#2770 = CARTESIAN_POINT ( 'NONE',  ( 10.93730112725995873, 4.928439153522441885, -151.0983828010091656 ) ) ;
#2771 = CARTESIAN_POINT ( 'NONE',  ( 109.1721716018069657, -0.01665253177026227577, 0.003746085893652734838 ) ) ;
#2772 = DIRECTION ( 'NONE',  ( -0.7637818620346800147, 0.3617919495470713898, -0.5345501402766312804 ) ) ;
#2773 = CARTESIAN_POINT ( 'NONE',  ( -2.911734481061399205, -44.38410240830292963, 17.36785190846027049 ) ) ;
#2774 = CARTESIAN_POINT ( 'NONE',  ( 1.832998868059858122, -97.49378069860870255, 107.4798986104856766 ) ) ;
#2775 = CARTESIAN_POINT ( 'NONE',  ( -20.37983603106073716, -23.16947629293375854, -18.69865230096518616 ) ) ;
#2776 = ORIENTED_EDGE ( 'NONE', *, *, #818, .T. ) ;
#2777 = CONICAL_SURFACE ( 'NONE', #24386, 34.60786435723138510, 0.8559913436420825139 ) ;
#2779 = CARTESIAN_POINT ( 'NONE',  ( 32.73300124599737160, -75.82012867748541396, 89.94078864464039214 ) ) ;
#2778 = CARTESIAN_POINT ( 'NONE',  ( 32.73300124599738581, -72.21147546950486174, -92.86301839380092815 ) ) ;
#2780 = CIRCLE ( 'NONE', #23503, 117.6351876552689504 ) ;
#2781 = CARTESIAN_POINT ( 'NONE',  ( 9.884929003653626367, -132.4189379373565316, -71.59798461011472170 ) ) ;
#2782 = CARTESIAN_POINT ( 'NONE',  ( -20.20700224038492721, 23.35150625415659320, -18.19058640100232438 ) ) ;
#2783 = CARTESIAN_POINT ( 'NONE',  ( -1.155031165708876317, 16.13806347973058664, 42.97366960678581194 ) ) ;
#2784 = ADVANCED_FACE ( 'NONE', ( #16888 ), #12640, .F. ) ;
#2785 = ORIENTED_EDGE ( 'NONE', *, *, #3535, .T. ) ;
#2786 = CARTESIAN_POINT ( 'NONE',  ( 32.73300124599732186, 0.000000000000000000, 0.000000000000000000 ) ) ;
#2787 = VECTOR ( 'NONE', #26228, 1000.000000000000114 ) ;
#2788 = VERTEX_POINT ( 'NONE', #17010 ) ;
#2789 = CARTESIAN_POINT ( 'NONE',  ( -8.786685647604885574, 6.096987947571466530E-17, -1.524246986892866633E-17 ) ) ;
#2790 = CARTESIAN_POINT ( 'NONE',  ( -55.24340739397742794, -0.01010924026184046101, 0.0007387096945705813253 ) ) ;
#2791 = ORIENTED_EDGE ( 'NONE', *, *, #13176, .F. ) ;
#2792 = CARTESIAN_POINT ( 'NONE',  ( 10.93730112726024117, 133.3192575531818136, -71.28103789254788580 ) ) ;
#2793 = ORIENTED_EDGE ( 'NONE', *, *, #1155, .T. ) ;
#2794 = CARTESIAN_POINT ( 'NONE',  ( -22.34422965417124729, -37.30738373203622871, -6.759368364654178230 ) ) ;
#2795 = VERTEX_POINT ( 'NONE', #14706 ) ;
#2796 = ADVANCED_FACE ( 'NONE', ( #6238 ), #22399, .F. ) ;
#2797 = B_SPLINE_CURVE_WITH_KNOTS ( 'NONE', 3,
 ( #4649, #2629, #11132, #13706, #11410, #15567, #10992 ),
 .UNSPECIFIED., .F., .F.,
 ( 4, 3, 4 ),
 ( 6.745041218394538905E-16, 0.02816610861753245793, 0.04000277880656290252 ),
 .UNSPECIFIED. ) ;
#2798 = B_SPLINE_CURVE_WITH_KNOTS ( 'NONE', 3,
 ( #20190, #13148, #10863, #479, #9271, #26111 ),
 .UNSPECIFIED., .F., .F.,
 ( 4, 2, 4 ),
 ( 3.681866292528241208E-16, 0.003576372551511175675, 0.007152745103021982721 ),
 .UNSPECIFIED. ) ;
#2799 = ORIENTED_EDGE ( 'NONE', *, *, #13654, .F. ) ;
#2800 = DIRECTION ( 'NONE',  ( 0.000000000000000000, 0.000000000000000000, 1.000000000000000000 ) ) ;
#2801 = AXIS2_PLACEMENT_3D ( 'NONE', #25808, #23379, #3630 ) ;
#2802 = VECTOR ( 'NONE', #11675, 1000.000000000000114 ) ;
#2803 = CARTESIAN_POINT ( 'NONE',  ( 1.832998868059858122, -84.86110816369524912, -117.7096351258396396 ) ) ;
#2804 = CARTESIAN_POINT ( 'NONE',  ( 1.833485406944057594, 15.69895494453384721, 144.2578170162063884 ) ) ;
#2805 = CARTESIAN_POINT ( 'NONE',  ( -9.156249394959713683, 38.89149400288408032, -38.17928057392006025 ) ) ;
#2806 =( BOUNDED_SURFACE ( )  B_SPLINE_SURFACE ( 3, 1, ( 
 ( #9652, #5186 ),
 ( #11670, #4904 ),
 ( #22774, #3041 ),
 ( #1016, #22477 ) ),
 .UNSPECIFIED., .F., .F., .F. ) 
 B_SPLINE_SURFACE_WITH_KNOTS ( ( 4, 4 ),
 ( 2, 2 ),
 ( 0.000000000000000000, 1.000000000000000000 ),
 ( 0.000000000000000000, 1.000000000000000000 ),
 .UNSPECIFIED. ) 
 GEOMETRIC_REPRESENTATION_ITEM ( )  RATIONAL_B_SPLINE_SURFACE ( (
 ( 1.000000000000000000, 1.000000000000000000),
 ( 0.7789835883360576307, 0.9689951854195403280),
 ( 0.7789835883360576307, 0.9689951854195403280),
 ( 1.000000000000000000, 1.000000000000000000) ) ) 
 REPRESENTATION_ITEM ( '' )  SURFACE ( )  );
#2807 = CARTESIAN_POINT ( 'NONE',  ( 1.833838850855489255, -72.47782099564557257, -125.7132320915355876 ) ) ;
#2808 = CARTESIAN_POINT ( 'NONE',  ( 13.36082413113063083, 106.9547846563635431, 109.3026516754236184 ) ) ;
#2809 = CARTESIAN_POINT ( 'NONE',  ( 180.4657679828686980, -20.00000000000000000, 3.130582043300658722E-16 ) ) ;
#2810 = PRODUCT_DEFINITION_SHAPE ( 'NONE', 'NONE',  #28483 ) ;
#2811 = FACE_OUTER_BOUND ( 'NONE', #10078, .T. ) ;
#2812 = CARTESIAN_POINT ( 'NONE',  ( 16.75465622695647738, -98.56308464785139734, 102.5353941815400418 ) ) ;
#2813 = B_SPLINE_CURVE_WITH_KNOTS ( 'NONE', 3,
 ( #8241, #17003, #22026, #11096, #15530, #26481, #19720, #11234, #6786, #2291 ),
 .UNSPECIFIED., .F., .F.,
 ( 4, 2, 2, 2, 4 ),
 ( 2.863532086325413454E-16, 0.0003346187017559052986, 0.0006692374035115242594, 0.001003856105267143329, 0.001338474807022762289 ),
 .UNSPECIFIED. ) ;
#2814 = ORIENTED_EDGE ( 'NONE', *, *, #26216, .T. ) ;
#2815 = LINE ( 'NONE', #25001, #17972 ) ;
#2817 = CARTESIAN_POINT ( 'NONE',  ( 25.70243777736191859, 45.26941207740291873, 103.4793210720849004 ) ) ;
#2816 = CARTESIAN_POINT ( 'NONE',  ( 94.22246935314088034, 90.00000000000005684, -6.938893903907228378E-15 ) ) ;
#2818 = CARTESIAN_POINT ( 'NONE',  ( 25.65782528836477638, -84.30028114518222537, 75.12678957786475564 ) ) ;
#2819 = CARTESIAN_POINT ( 'NONE',  ( -4.178947244162622532, 45.38689110596718734, -18.28784278438465805 ) ) ;
#2820 = EDGE_LOOP ( 'NONE', ( #962, #18818, #23589, #27214 ) ) ;
#2821 = EDGE_LOOP ( 'NONE', ( #19997, #20775, #3010, #19375 ) ) ;
#2822 = DIRECTION ( 'NONE',  ( 0.000000000000000000, 0.000000000000000000, 1.000000000000000000 ) ) ;
#2823 = VECTOR ( 'NONE', #4638, 1000.000000000000227 ) ;
#2824 = CARTESIAN_POINT ( 'NONE',  ( 1.832998868059890096, 145.1092030902949830, 0.5339089137752738301 ) ) ;
#2825 = CARTESIAN_POINT ( 'NONE',  ( -55.25297051322618813, -0.002853887643042011396, 0.01466904165775133329 ) ) ;
#2826 = ORIENTED_EDGE ( 'NONE', *, *, #21057, .T. ) ;
#2827 = CARTESIAN_POINT ( 'NONE',  ( 1.832998868059890096, 97.49378069860942730, -107.4798986104850087 ) ) ;
#2828 = CIRCLE ( 'NONE', #9742, 151.1787379149930359 ) ;
#2829 = EDGE_LOOP ( 'NONE', ( #10399, #3790, #8937, #775 ) ) ;
#2830 = CARTESIAN_POINT ( 'NONE',  ( 24.22246935314087324, 90.00000000000005684, 39.99999999999999289 ) ) ;
#2831 = EDGE_CURVE ( 'NONE', #7680, #22569, #14980, .T. ) ;
#2832 = CIRCLE ( 'NONE', #13394, 117.6351876552689504 ) ;
#2833 = ADVANCED_FACE ( 'NONE', ( #17157 ), #10809, .F. ) ;
#2834 = CARTESIAN_POINT ( 'NONE',  ( -25.21435515916043357, -34.29329011225959079, -4.655591116594231416 ) ) ;
#2835 = CARTESIAN_POINT ( 'NONE',  ( 109.1586059443104944, 0.002622205828288684017, 0.006570129623060880740 ) ) ;
#2836 = ORIENTED_EDGE ( 'NONE', *, *, #2720, .F. ) ;
#2837 = CARTESIAN_POINT ( 'NONE',  ( 32.73300124599735739, -44.31599526638029118, 108.9684813982487412 ) ) ;
#2838 = B_SPLINE_CURVE_WITH_KNOTS ( 'NONE', 3,
 ( #7960, #16724, #23488, #1862, #12801, #14963, #21451, #132, #3898, #4313, #6625, #25924, #4442 ),
 .UNSPECIFIED., .F., .F.,
 ( 4, 3, 3, 3, 4 ),
 ( 1.250926888277100303E-17, 0.0007657099931970583933, 0.001531419946797919589, 0.002296279302920155134, 0.003061450627205745088 ),
 .UNSPECIFIED. ) ;
#2839 = ORIENTED_EDGE ( 'NONE', *, *, #8333, .T. ) ;
#2840 = DIRECTION ( 'NONE',  ( -0.5946245182733607137, 0.08110646981860127058, -0.7999021332774015614 ) ) ;
#2841 = DIRECTION ( 'NONE',  ( 0.000000000000000000, 0.000000000000000000, 1.000000000000000000 ) ) ;
#2842 = CARTESIAN_POINT ( 'NONE',  ( -21.41430102051744200, -1.815007301162189446, -30.75470819672111134 ) ) ;
#2843 = EDGE_LOOP ( 'NONE', ( #4922, #18678, #26819, #7289, #15528, #27664, #11564, #7666, #21942, #22075, #9126, #24896, #21469, #13925, #1072, #22571, #19319, #18253, #23211, #27188, #17300, #120, #25770, #2407, #24343, #12123, #17271, #3644, #14897, #27958, #20488, #1000, #26399, #27934, #1162, #26185, #15819, #13439, #18311, #17751, #10530, #5949, #913, #20168, #16926, #18795, #22005, #16529, #6294, #24219, #22346, #27571, #25549, #14558, #2497, #27032, #306, #1973, #9674, #12306, #2552, #11223, #4104, #9613 ) ) ;
#2844 = EDGE_CURVE ( 'NONE', #1503, #13365, #15260, .T. ) ;
#2845 = CARTESIAN_POINT ( 'NONE',  ( 25.64681081121879203, 0.4157506337727869816, 112.9102952884414464 ) ) ;
#2846 = CARTESIAN_POINT ( 'NONE',  ( -1.031422197589716205, 28.14735071801744581, -36.13727897780137965 ) ) ;
#2847 = CARTESIAN_POINT ( 'NONE',  ( 25.64681081121880624, 23.06870491922473931, -110.5293738517606243 ) ) ;
#2848 = VERTEX_POINT ( 'NONE', #23936 ) ;
#2849 = VECTOR ( 'NONE', #25234, 1000.000000000000341 ) ;
#2850 = ORIENTED_EDGE ( 'NONE', *, *, #26796, .F. ) ;
#2851 = ORIENTED_EDGE ( 'NONE', *, *, #17222, .T. ) ;
#2852 = CARTESIAN_POINT ( 'NONE',  ( -55.24728320129491266, -0.0006547948648744401781, 0.01453410071985650025 ) ) ;
#2853 = CARTESIAN_POINT ( 'NONE',  ( 26.11404676487259024, 45.01677474591551942, -103.8885755249565079 ) ) ;
#2855 = CARTESIAN_POINT ( 'NONE',  ( 25.64708228042121618, 75.52311986518023446, 83.93578330383108721 ) ) ;
#2854 = CARTESIAN_POINT ( 'NONE',  ( 1.832998868059858122, 15.69902610990375713, 144.2584710144581095 ) ) ;
#2856 = CARTESIAN_POINT ( 'NONE',  ( -1.050229599974473293, 0.2556477501659514262, -45.79907399707867199 ) ) ;
#2857 = CARTESIAN_POINT ( 'NONE',  ( -25.21435515916025594, 34.29329011225976842, -4.655591116594504086 ) ) ;
#2858 = CARTESIAN_POINT ( 'NONE',  ( 25.64692872815575342, -84.12425003484094077, 75.31297890941242201 ) ) ;
#2859 =( BOUNDED_SURFACE ( )  B_SPLINE_SURFACE ( 3, 1, ( 
 ( #16146, #9537 ),
 ( #463, #24949 ),
 ( #2763, #20750 ),
 ( #20319, #26935 ) ),
 .UNSPECIFIED., .F., .F., .F. ) 
 B_SPLINE_SURFACE_WITH_KNOTS ( ( 4, 4 ),
 ( 2, 2 ),
 ( 0.000000000000000000, 1.000000000000000000 ),
 ( 0.000000000000000000, 1.000000000000000000 ),
 .UNSPECIFIED. ) 
 GEOMETRIC_REPRESENTATION_ITEM ( )  RATIONAL_B_SPLINE_SURFACE ( (
 ( 1.000000000000000000, 1.000000000000000000),
 ( 0.9593753223639863714, 0.9995975284513187731),
 ( 0.9593753223639863714, 0.9995975284513187731),
 ( 1.000000000000000000, 1.000000000000000000) ) ) 
 REPRESENTATION_ITEM ( '' )  SURFACE ( )  );
#2860 = CARTESIAN_POINT ( 'NONE',  ( -2.904412668506669348, -46.12477647685265936, 11.97478724945559136 ) ) ;
#2861 = VERTEX_POINT ( 'NONE', #15540 ) ;
#2862 = CARTESIAN_POINT ( 'NONE',  ( 2.430230287190592531, 132.3371620660959138, -60.50928654924622663 ) ) ;
#2863 = CARTESIAN_POINT ( 'NONE',  ( 26.11404676487257603, 110.9778746459746941, 22.43340081644806006 ) ) ;
#2864 = CARTESIAN_POINT ( 'NONE',  ( 25.64681081121880624, 11.38886654529674303, 112.3352186517031157 ) ) ;
#2865 = EDGE_CURVE ( 'NONE', #9063, #4666, #20788, .T. ) ;
#2866 = CARTESIAN_POINT ( 'NONE',  ( -1.031422197589716205, -37.93675465142491277, -25.67058493451430934 ) ) ;
#2867 = CARTESIAN_POINT ( 'NONE',  ( -20.20612092514784308, -27.77903665678158873, 10.22177639105890279 ) ) ;
#2868 = EDGE_CURVE ( 'NONE', #10229, #9016, #15998, .T. ) ;
#2869 = CARTESIAN_POINT ( 'NONE',  ( 25.65782528836481191, -75.12678957786447143, -84.30028114518245275 ) ) ;
#2870 = EDGE_LOOP ( 'NONE', ( #10453, #1098, #9974, #27720 ) ) ;
#2871 = CARTESIAN_POINT ( 'NONE',  ( 2.430230287190589422, -137.9371479820465254, 46.34481016236777862 ) ) ;
#2872 = ORIENTED_EDGE ( 'NONE', *, *, #18785, .T. ) ;
#2874 = EDGE_CURVE ( 'NONE', #11368, #3864, #2585, .T. ) ;
#2873 = CARTESIAN_POINT ( 'NONE',  ( 30.59141879584294443, -44.78722686469137670, -107.2355637993506292 ) ) ;
#2875 = CARTESIAN_POINT ( 'NONE',  ( 13.36082413113063083, -56.35051087435060424, 142.1654513177086301 ) ) ;
#2876 = ORIENTED_EDGE ( 'NONE', *, *, #6707, .T. ) ;
#2877 = CIRCLE ( 'NONE', #1931, 20.00000000000000000 ) ;
#2878 = ADVANCED_FACE ( 'NONE', ( #21765 ), #13725, .F. ) ;
#2879 = EDGE_LOOP ( 'NONE', ( #22242, #6218, #11057, #6869 ) ) ;
#2880 = VERTEX_POINT ( 'NONE', #8660 ) ;
#2881 = CARTESIAN_POINT ( 'NONE',  ( -1.583189561560253589, -29.24830400313191348, -36.01941156322777005 ) ) ;
#2882 = CARTESIAN_POINT ( 'NONE',  ( 25.64660436782539676, 56.95711784271983902, 97.49251393956794232 ) ) ;
#2883 = CARTESIAN_POINT ( 'NONE',  ( -20.20700224038492010, 24.51628800869071867, 16.58740185276683832 ) ) ;
#2884 = CARTESIAN_POINT ( 'NONE',  ( 1.833485406944043827, 125.9346397303445286, -72.09189602597577107 ) ) ;
#2885 = VERTEX_POINT ( 'NONE', #9087 ) ;
#2886 = CARTESIAN_POINT ( 'NONE',  ( -20.24399999263415140, -24.70869149526192032, 16.36687688782885530 ) ) ;
#2887 = CARTESIAN_POINT ( 'NONE',  ( 25.98552792386798060, 45.02923844025622202, -103.7897946223260703 ) ) ;
#2888 = CARTESIAN_POINT ( 'NONE',  ( -20.24399999263415495, -27.76448601145549233, -10.36954246768234889 ) ) ;
#2889 = ORIENTED_EDGE ( 'NONE', *, *, #13729, .F. ) ;
#2890 = ORIENTED_EDGE ( 'NONE', *, *, #9074, .F. ) ;
#2891 = B_SPLINE_CURVE_WITH_KNOTS ( 'NONE', 3,
 ( #4791, #13410, #22210, #9107 ),
 .UNSPECIFIED., .F., .F.,
 ( 4, 4 ),
 ( 1.904175111373004964E-16, 0.001982023823822943748 ),
 .UNSPECIFIED. ) ;
#2892 = FACE_OUTER_BOUND ( 'NONE', #4368, .T. ) ;
#2893 = CARTESIAN_POINT ( 'NONE',  ( 5.340103579038181003, 2.303180387975235277, 147.4316330314912591 ) ) ;
#2894 = CARTESIAN_POINT ( 'NONE',  ( 109.1589550718174877, 0.007359857714023718654, 0.001793588804091254558 ) ) ;
#2895 = B_SPLINE_CURVE_WITH_KNOTS ( 'NONE', 3,
 ( #5873, #14632, #23431, #3695, #21257, #14773, #23584, #3844, #12609, #21395 ),
 .UNSPECIFIED., .F., .F.,
 ( 4, 3, 3, 4 ),
 ( 1.387778780781445676E-17, 0.0002669560319015968665, 0.0005492286108966422126, 0.0008315040496093392599 ),
 .UNSPECIFIED. ) ;
#2896 = CARTESIAN_POINT ( 'NONE',  ( -7.078251931573406708, -34.59014398252944034, -38.93060825814217196 ) ) ;
#2897 = CARTESIAN_POINT ( 'NONE',  ( 2.433796855181205476, 109.1007109081238724, -96.28145139437575040 ) ) ;
#2898 = AXIS2_PLACEMENT_3D ( 'NONE', #10997, #15291, #13006 ) ;
#2899 = DIRECTION ( 'NONE',  ( 0.000000000000000000, -5.223019709708116647E-21, 1.000000000000000000 ) ) ;
#2900 = VERTEX_POINT ( 'NONE', #26491 ) ;
#2901 = CARTESIAN_POINT ( 'NONE',  ( 25.65782528836479770, 84.30028114518268012, -75.12678957786421563 ) ) ;
#2902 = CARTESIAN_POINT ( 'NONE',  ( -1.048996300304498419, -0.7649764263854993418, -45.79145529752469201 ) ) ;
#2904 =( BOUNDED_SURFACE ( )  B_SPLINE_SURFACE ( 3, 1, ( 
 ( #9655, #17843 ),
 ( #7358, #16124 ),
 ( #5039, #7225 ),
 ( #586, #24350 ) ),
 .UNSPECIFIED., .F., .F., .F. ) 
 B_SPLINE_SURFACE_WITH_KNOTS ( ( 4, 4 ),
 ( 2, 2 ),
 ( 0.000000000000000000, 1.000000000000000000 ),
 ( 0.000000000000000000, 1.000000000000000000 ),
 .UNSPECIFIED. ) 
 GEOMETRIC_REPRESENTATION_ITEM ( )  RATIONAL_B_SPLINE_SURFACE ( (
 ( 1.000000000000000000, 1.000000000000000000),
 ( 0.9593753223639863714, 0.9995975284513187731),
 ( 0.9593753223639863714, 0.9995975284513187731),
 ( 1.000000000000000000, 1.000000000000000000) ) ) 
 REPRESENTATION_ITEM ( '' )  SURFACE ( )  );
#2903 = AXIS2_PLACEMENT_3D ( 'NONE', #3556, #18970, #12337 ) ;
#2905 = EDGE_CURVE ( 'NONE', #24611, #6748, #19418, .T. ) ;
#2906 = EDGE_CURVE ( 'NONE', #18869, #16496, #16356, .T. ) ;
#2907 = CARTESIAN_POINT ( 'NONE',  ( -55.24300891470648622, -0.002702093572889207890, -0.009439835024157681651 ) ) ;
#2908 = CARTESIAN_POINT ( 'NONE',  ( -1.619063947482197729, -38.92136151114888776, 25.20140673341416360 ) ) ;
#2909 = CARTESIAN_POINT ( 'NONE',  ( -1.044556982611269280, 37.98985389331847529, 25.56989963842161728 ) ) ;
#2910 = ORIENTED_EDGE ( 'NONE', *, *, #166, .T. ) ;
#2911 = ORIENTED_EDGE ( 'NONE', *, *, #4965, .T. ) ;
#2913 = ADVANCED_FACE ( 'NONE', ( #4620 ), #19608, .F. ) ;
#2912 = PLANE ( 'NONE',  #14273 ) ;
#2914 = B_SPLINE_CURVE_WITH_KNOTS ( 'NONE', 3,
 ( #24111, #25319, #5596, #18979 ),
 .UNSPECIFIED., .F., .F.,
 ( 4, 4 ),
 ( 2.938411120583618971E-16, 0.01077107486149829312 ),
 .UNSPECIFIED. ) ;
#2915 = ORIENTED_EDGE ( 'NONE', *, *, #2698, .F. ) ;
#2916 = ORIENTED_EDGE ( 'NONE', *, *, #14570, .F. ) ;
#2917 = VERTEX_POINT ( 'NONE', #6939 ) ;
#2918 = CARTESIAN_POINT ( 'NONE',  ( 109.1624594426973118, -0.01405141589344819329, -0.007576898892907043756 ) ) ;
#2919 =( GEOMETRIC_REPRESENTATION_CONTEXT ( 3 ) GLOBAL_UNCERTAINTY_ASSIGNED_CONTEXT ( ( #3341 ) ) GLOBAL_UNIT_ASSIGNED_CONTEXT ( ( #24443, #17931, #13762 ) ) REPRESENTATION_CONTEXT ( 'NONE', 'WORKASPACE' ) );
#2920 = CARTESIAN_POINT ( 'NONE',  ( -1.019300379054419725, -35.83762006677378764, 28.53917295602937187 ) ) ;
#2921 = CARTESIAN_POINT ( 'NONE',  ( 28.43349137099833968, 46.80919715693054428, -115.0977416143052068 ) ) ;
#2922 = CARTESIAN_POINT ( 'NONE',  ( 109.1586900883932856, 0.006819617742892441180, -0.002109621908824171194 ) ) ;
#2923 = CARTESIAN_POINT ( 'NONE',  ( 26.11404676487257603, 22.43340081644767636, 110.9778746459747794 ) ) ;
#2924 = DIRECTION ( 'NONE',  ( 1.000000000000000000, -6.938893903907226837E-18, 1.734723475976806709E-18 ) ) ;
#2925 = DIRECTION ( 'NONE',  ( -1.000000000000000000, -0.000000000000000000, -0.000000000000000000 ) ) ;
#2926 = CARTESIAN_POINT ( 'NONE',  ( -55.24390624410018802, -0.007245494385991098352, -0.007503127514281985981 ) ) ;
#2927 = B_SPLINE_CURVE_WITH_KNOTS ( 'NONE', 3,
 ( #7432, #9581, #18341, #27124, #1058, #23099, #1334 ),
 .UNSPECIFIED., .F., .F.,
 ( 4, 3, 4 ),
 ( 0.000000000000000000, 0.02398743853561339720, 0.04000277880656218088 ),
 .UNSPECIFIED. ) ;
#2928 = CARTESIAN_POINT ( 'NONE',  ( 1.833838850093465700, -85.29338149487134046, -117.3962623502782918 ) ) ;
#2930 = VECTOR ( 'NONE', #18557, 999.9999999999998863 ) ;
#2929 = CARTESIAN_POINT ( 'NONE',  ( 8.186469829614351212, -118.7566730983342325, -90.56875932797710504 ) ) ;
#2931 = CARTESIAN_POINT ( 'NONE',  ( -23.79223135445719350, -3.207301057648115350, 33.03345552685149755 ) ) ;
#2932 = CARTESIAN_POINT ( 'NONE',  ( 25.87036335909426654, -83.35447252092919257, 76.38467849957120848 ) ) ;
#2933 = EDGE_CURVE ( 'NONE', #3608, #8194, #4681, .T. ) ;
#2934 = CARTESIAN_POINT ( 'NONE',  ( 1.833206310202338374, 15.90849712171739405, 144.2348262833782542 ) ) ;
#2935 = CARTESIAN_POINT ( 'NONE',  ( -1.050229599974473516, -37.20249516760156183, 26.71319688967675177 ) ) ;
#2936 = DIRECTION ( 'NONE',  ( -0.5946245182733607137, -0.7356888587241614541, -0.3243201896541662577 ) ) ;
#2937 = DIRECTION ( 'NONE',  ( -1.000000000000000000, -0.000000000000000000, -0.000000000000000000 ) ) ;
#2938 = ORIENTED_EDGE ( 'NONE', *, *, #23419, .T. ) ;
#2939 = CARTESIAN_POINT ( 'NONE',  ( 28.37599760073041821, -13.77583212279408720, 113.9023239246302523 ) ) ;
#2940 = ORIENTED_EDGE ( 'NONE', *, *, #10678, .T. ) ;
#2942 = EDGE_CURVE ( 'NONE', #16635, #1896, #1216, .T. ) ;
#2941 = CARTESIAN_POINT ( 'NONE',  ( 109.1586900883932856, -0.005236795036868191477, -0.004851151255031838257 ) ) ;
#2943 = CARTESIAN_POINT ( 'NONE',  ( 25.87036335909427720, 12.80197335559962468, 112.3329723497411408 ) ) ;
#2944 = EDGE_LOOP ( 'NONE', ( #22047, #2129, #9802, #26217 ) ) ;
#2945 = EDGE_CURVE ( 'NONE', #17470, #12390, #3318, .T. ) ;
#2946 = VERTEX_POINT ( 'NONE', #734 ) ;
#2947 = ORIENTED_EDGE ( 'NONE', *, *, #5235, .F. ) ;
#2948 = B_SPLINE_CURVE_WITH_KNOTS ( 'NONE', 3,
 ( #26181, #2264, #24179, #8362, #23775, #21728 ),
 .UNSPECIFIED., .F., .F.,
 ( 4, 2, 4 ),
 ( 1.908688579121390716E-17, 0.0006311636237756899697, 0.001262327247551360641 ),
 .UNSPECIFIED. ) ;
#2949 = B_SPLINE_CURVE_WITH_KNOTS ( 'NONE', 3,
 ( #21219, #18489, #27260, #27840, #7572, #16327 ),
 .UNSPECIFIED., .F., .F.,
 ( 4, 2, 4 ),
 ( 3.930079588515292562E-17, 0.0006311571484586184742, 0.001262314296917197484 ),
 .UNSPECIFIED. ) ;
#2950 =( BOUNDED_SURFACE ( )  B_SPLINE_SURFACE ( 3, 1, ( 
 ( #20484, #18470 ),
 ( #18307, #20767 ),
 ( #9694, #24691 ),
 ( #24826, #907 ) ),
 .UNSPECIFIED., .F., .F., .F. ) 
 B_SPLINE_SURFACE_WITH_KNOTS ( ( 4, 4 ),
 ( 2, 2 ),
 ( 0.000000000000000000, 1.000000000000000000 ),
 ( 0.000000000000000000, 1.000000000000000000 ),
 .UNSPECIFIED. ) 
 GEOMETRIC_REPRESENTATION_ITEM ( )  RATIONAL_B_SPLINE_SURFACE ( (
 ( 1.000000000000000000, 1.000000000000000000),
 ( 0.6386103224230316178, 0.9954351624131538845),
 ( 0.6386103224230316178, 0.9954351624131538845),
 ( 1.000000000000000000, 1.000000000000000000) ) ) 
 REPRESENTATION_ITEM ( '' )  SURFACE ( )  );
#2951 = CARTESIAN_POINT ( 'NONE',  ( 8.186469777910955870, 12.15801985874169056, -148.8557359139592506 ) ) ;
#2952 = B_SPLINE_CURVE_WITH_KNOTS ( 'NONE', 3,
 ( #9476, #11476, #27447, #5288, #7616, #16226 ),
 .UNSPECIFIED., .F., .F.,
 ( 4, 2, 4 ),
 ( 3.178475462313071774E-16, 0.003576372551511121031, 0.007152745103021923741 ),
 .UNSPECIFIED. ) ;
#2953 = CARTESIAN_POINT ( 'NONE',  ( -9.156249394959706578, 25.18996226954685369, 48.32878616080981260 ) ) ;
#2954 = CARTESIAN_POINT ( 'NONE',  ( 1.834118845439484335, -132.6369225636078113, 58.85894970554871009 ) ) ;
#2955 = CARTESIAN_POINT ( 'NONE',  ( 1.833691583653537238, 29.82175144858098648, 142.0122737882508943 ) ) ;
#2956 = CARTESIAN_POINT ( 'NONE',  ( -1.619063947482197729, -2.489035965910479486, -46.30105812165547974 ) ) ;
#2957 = B_SPLINE_CURVE_WITH_KNOTS ( 'NONE', 3,
 ( #7837, #26944, #5665, #23239 ),
 .UNSPECIFIED., .F., .F.,
 ( 4, 4 ),
 ( 0.000000000000000000, 0.01077107196513799915 ),
 .UNSPECIFIED. ) ;
#2958 = CARTESIAN_POINT ( 'NONE',  ( -22.23342874802667879, -30.68433055777675733, 7.677086057585283285 ) ) ;
#2959 = CARTESIAN_POINT ( 'NONE',  ( 109.1587776205901861, -0.002185517590237729887, 0.006995903587863968806 ) ) ;
#2960 = CARTESIAN_POINT ( 'NONE',  ( -1.045287976400365970, 15.59869763335068171, -43.05558670614252037 ) ) ;
#2961 = CARTESIAN_POINT ( 'NONE',  ( -55.24300891470648622, 0.009225237711098475957, 0.003362556190414738716 ) ) ;
#2962 = CARTESIAN_POINT ( 'NONE',  ( 25.64681081121879203, -110.3564950173080206, -23.88203588908195130 ) ) ;
#2963 = CARTESIAN_POINT ( 'NONE',  ( 28.37603512858450117, -78.09501335733530425, -84.05169593519805460 ) ) ;
#2964 = CARTESIAN_POINT ( 'NONE',  ( -1.323439229708141651, -2.317790194800056547, -46.01398008004440499 ) ) ;
#2965 = ORIENTED_EDGE ( 'NONE', *, *, #23655, .T. ) ;
#2966 = CARTESIAN_POINT ( 'NONE',  ( 1.834118845439484335, -145.1099497418795750, -0.1779704863085233013 ) ) ;
#2968 = CARTESIAN_POINT ( 'NONE',  ( -21.41430102051744910, 7.777552968935758315, -29.81033373822130628 ) ) ;
#2967 = LINE ( 'NONE', #24850, #27207 ) ;
#2969 = ADVANCED_FACE ( 'NONE', ( #27354 ), #22574, .F. ) ;
#2970 = CARTESIAN_POINT ( 'NONE',  ( -1.619063947482197729, -46.30105812165550105, -2.489035965909997206 ) ) ;
#2971 = CARTESIAN_POINT ( 'NONE',  ( 109.1586900883932856, 0.0008465529156545837123, -0.007088091345232582462 ) ) ;
#2972 = B_SPLINE_CURVE_WITH_KNOTS ( 'NONE', 3,
 ( #18754, #2934, #7696, #20910, #12277, #7395 ),
 .UNSPECIFIED., .F., .F.,
 ( 4, 2, 4 ),
 ( 1.042864983293993125E-17, 0.0006311571484586064396, 0.001262314296917202688 ),
 .UNSPECIFIED. ) ;
#2973 = CARTESIAN_POINT ( 'NONE',  ( 28.37603512858360588, -113.9023475466375572, 13.77584568114256314 ) ) ;
#2974 = VERTEX_POINT ( 'NONE', #15848 ) ;
#2975 = ORIENTED_EDGE ( 'NONE', *, *, #23914, .T. ) ;
#2976 = FACE_OUTER_BOUND ( 'NONE', #28445, .T. ) ;
#2977 = CARTESIAN_POINT ( 'NONE',  ( 109.1778270068192853, 0.002542344697958587828, 0.008960903982060992520 ) ) ;
#2978 = VERTEX_POINT ( 'NONE', #18273 ) ;
#2979 = CARTESIAN_POINT ( 'NONE',  ( 25.64692872815577829, -97.94438212068862981, 56.17679456083764222 ) ) ;
#2980 = ORIENTED_EDGE ( 'NONE', *, *, #13125, .F. ) ;
#2981 = CARTESIAN_POINT ( 'NONE',  ( 109.1587776205901861, 0.007186028091168156912, 0.001442274044995822289 ) ) ;
#2982 = ORIENTED_EDGE ( 'NONE', *, *, #9468, .T. ) ;
#2983 = CARTESIAN_POINT ( 'NONE',  ( 10.93730112726006354, 145.2260730187408626, -42.00474393596100953 ) ) ;
#2984 =( BOUNDED_SURFACE ( )  B_SPLINE_SURFACE ( 3, 1, ( 
 ( #11143, #19919 ),
 ( #203, #6834 ),
 ( #8991, #15577 ),
 ( #4662, #17191 ) ),
 .UNSPECIFIED., .F., .F., .F. ) 
 B_SPLINE_SURFACE_WITH_KNOTS ( ( 4, 4 ),
 ( 2, 2 ),
 ( 0.000000000000000000, 1.000000000000000000 ),
 ( 0.000000000000000000, 1.000000000000000000 ),
 .UNSPECIFIED. ) 
 GEOMETRIC_REPRESENTATION_ITEM ( )  RATIONAL_B_SPLINE_SURFACE ( (
 ( 1.000000000000000000, 1.000000000000000000),
 ( 0.9934239774497838349, 0.8357310067453913582),
 ( 0.9934239774497838349, 0.8357310067453913582),
 ( 1.000000000000000000, 1.000000000000000000) ) ) 
 REPRESENTATION_ITEM ( '' )  SURFACE ( )  );
#2985 = ORIENTED_EDGE ( 'NONE', *, *, #12549, .T. ) ;
#2986 = CARTESIAN_POINT ( 'NONE',  ( 32.73300124599737160, -117.3295799645428872, -8.473903470907334423 ) ) ;
#2987 = ORIENTED_EDGE ( 'NONE', *, *, #14695, .T. ) ;
#2988 = CARTESIAN_POINT ( 'NONE',  ( -20.20700224038492721, -10.08426345511609235, -27.82980252387815767 ) ) ;
#2989 = CARTESIAN_POINT ( 'NONE',  ( -1.619063947482197729, -38.92136151114925724, -25.20140673341360227 ) ) ;
#2990 = DIRECTION ( 'NONE',  ( -1.000000000000000000, 6.938893903907226837E-18, -1.734723475976806709E-18 ) ) ;
#2991 = CARTESIAN_POINT ( 'NONE',  ( 1.833809397773861205, -125.7576368866148755, 72.40070666294548118 ) ) ;
#2992 = ORIENTED_EDGE ( 'NONE', *, *, #20471, .T. ) ;
#2993 = EDGE_CURVE ( 'NONE', #194, #11495, #27523, .T. ) ;
#2994 = CARTESIAN_POINT ( 'NONE',  ( 10.93730112725990722, -136.0306644680979389, -65.95960219663263047 ) ) ;
#2995 = CARTESIAN_POINT ( 'NONE',  ( -1.619063947482197729, -29.22875152547781852, -35.99532424477369830 ) ) ;
#2996 = CARTESIAN_POINT ( 'NONE',  ( 25.87036335909427720, 98.40409479825439121, 55.67065048714044195 ) ) ;
#2997 = VERTEX_POINT ( 'NONE', #24792 ) ;
#2998 = ADVANCED_FACE ( 'NONE', ( #3181 ), #28422, .F. ) ;
#2999 = ORIENTED_EDGE ( 'NONE', *, *, #23329, .F. ) ;
#3000 = VERTEX_POINT ( 'NONE', #20592 ) ;
#3001 = CARTESIAN_POINT ( 'NONE',  ( -1.048171036023513025, 36.44209502233747600, 27.73816396939524509 ) ) ;
#3002 = CARTESIAN_POINT ( 'NONE',  ( 32.73300124599738581, 44.31599526638102304, -108.9684813982483860 ) ) ;
#3004 = DIRECTION ( 'NONE',  ( 1.000000000000000000, -6.938893903907226837E-18, 1.734723475976806709E-18 ) ) ;
#3003 = CARTESIAN_POINT ( 'NONE',  ( -20.90916690077964191, -39.20864005633521998, 5.322316104228396405 ) ) ;
#3005 = EDGE_CURVE ( 'NONE', #25954, #1001, #20128, .T. ) ;
#3006 = CARTESIAN_POINT ( 'NONE',  ( 16.75465622695663725, 48.33695624543491931, -133.7599617830020122 ) ) ;
#3007 = CARTESIAN_POINT ( 'NONE',  ( 1.833485406944043827, 144.3694338680884925, 14.63699153649408480 ) ) ;
#3008 = CARTESIAN_POINT ( 'NONE',  ( -16.86833981943427574, 39.83928801320588775, -19.19877306373863490 ) ) ;
#3009 = CARTESIAN_POINT ( 'NONE',  ( 25.64700659047693065, 46.13293552475933978, -103.0567718204598435 ) ) ;
#3010 = ORIENTED_EDGE ( 'NONE', *, *, #27252, .T. ) ;
#3011 = DIRECTION ( 'NONE',  ( 0.000000000000000000, 5.223019709708233256E-21, -1.000000000000000000 ) ) ;
#3012 = CARTESIAN_POINT ( 'NONE',  ( 28.37599760073042532, 98.45181492308118720, 58.91309773266183925 ) ) ;
#3013 = CARTESIAN_POINT ( 'NONE',  ( 25.64708228042121618, 11.76327187353814807, 112.2968511928420128 ) ) ;
#3014 = CARTESIAN_POINT ( 'NONE',  ( 1.832998868059890096, 84.86110816369760812, -117.7096351258379343 ) ) ;
#3015 = CARTESIAN_POINT ( 'NONE',  ( 26.11404676487257603, -47.08215554553588333, 102.9690087468800073 ) ) ;
#3016 = CARTESIAN_POINT ( 'NONE',  ( 25.98552792386797705, -84.79516057869827250, -74.89816102339797510 ) ) ;
#3017 = ORIENTED_EDGE ( 'NONE', *, *, #232, .T. ) ;
#3018 = CARTESIAN_POINT ( 'NONE',  ( -55.24300891470650754, 0.0003472257464218577502, 0.009812809446892801005 ) ) ;
#3019 = CARTESIAN_POINT ( 'NONE',  ( 24.01988960052061017, -100.1926921796488728, 84.46375358746880124 ) ) ;
#3020 = B_SPLINE_CURVE_WITH_KNOTS ( 'NONE', 3,
 ( #999, #7207, #3304, #18561, #14084, #12088, #5019 ),
 .UNSPECIFIED., .F., .F.,
 ( 4, 3, 4 ),
 ( 3.555125210177727942E-17, 0.02816610861753246139, 0.04000277880656218782 ),
 .UNSPECIFIED. ) ;
#3021 = CARTESIAN_POINT ( 'NONE',  ( 2.433796855181205476, -60.50726454507993424, 132.3327394885229182 ) ) ;
#3022 = ORIENTED_EDGE ( 'NONE', *, *, #14591, .F. ) ;
#3023 = ORIENTED_EDGE ( 'NONE', *, *, #15796, .F. ) ;
#3024 = ORIENTED_EDGE ( 'NONE', *, *, #6512, .F. ) ;
#3025 = B_SPLINE_CURVE_WITH_KNOTS ( 'NONE', 3,
 ( #13464, #1961, #10764, #5548 ),
 .UNSPECIFIED., .F., .F.,
 ( 4, 4 ),
 ( 1.892757412642747523E-16, 0.001982023823822945917 ),
 .UNSPECIFIED. ) ;
#3026 = CARTESIAN_POINT ( 'NONE',  ( -1.050231094221194983, -45.79908322896422135, 0.2545420581353859402 ) ) ;
#3027 = CARTESIAN_POINT ( 'NONE',  ( 25.64681081121880624, -23.88203588908001507, -110.3564950173084185 ) ) ;
#3028 = CARTESIAN_POINT ( 'NONE',  ( -1.239374126674604337, -44.48112152129355934, -11.92219841463812280 ) ) ;
#3029 = EDGE_CURVE ( 'NONE', #27652, #9673, #16279, .T. ) ;
#3030 = CARTESIAN_POINT ( 'NONE',  ( 26.11404676487257603, 112.4785329405482059, 12.95861723607491456 ) ) ;
#3031 = CARTESIAN_POINT ( 'NONE',  ( -1.619063947482201282, 44.80407745103784123, -11.94059994246174838 ) ) ;
#3032 = ORIENTED_EDGE ( 'NONE', *, *, #18785, .F. ) ;
#3033 = CARTESIAN_POINT ( 'NONE',  ( -21.81686047589425215, 16.72402253294313823, -34.70276904128894557 ) ) ;
#3034 = CARTESIAN_POINT ( 'NONE',  ( 1.833838850093477912, 44.84137955663405251, -138.0075868208081715 ) ) ;
#3035 =( BOUNDED_SURFACE ( )  B_SPLINE_SURFACE ( 3, 1, ( 
 ( #3580, #28030 ),
 ( #1698, #21561 ),
 ( #18992, #19540 ),
 ( #12361, #1422 ) ),
 .UNSPECIFIED., .F., .F., .F. ) 
 B_SPLINE_SURFACE_WITH_KNOTS ( ( 4, 4 ),
 ( 2, 2 ),
 ( 0.000000000000000000, 1.000000000000000000 ),
 ( 0.000000000000000000, 1.000000000000000000 ),
 .UNSPECIFIED. ) 
 GEOMETRIC_REPRESENTATION_ITEM ( )  RATIONAL_B_SPLINE_SURFACE ( (
 ( 1.000000000000000000, 1.000000000000000000),
 ( 0.7789835883360578528, 0.9689951854195403280),
 ( 0.7789835883360578528, 0.9689951854195403280),
 ( 1.000000000000000000, 1.000000000000000000) ) ) 
 REPRESENTATION_ITEM ( '' )  SURFACE ( )  );
#3036 = EDGE_CURVE ( 'NONE', #1086, #7747, #1026, .T. ) ;
#3037 = CARTESIAN_POINT ( 'NONE',  ( 32.73300124599737870, 20.69176323058787759, -115.8010721414081132 ) ) ;
#3038 = VERTEX_POINT ( 'NONE', #25648 ) ;
#3039 = EDGE_CURVE ( 'NONE', #1356, #5719, #15940, .T. ) ;
#3040 = EDGE_LOOP ( 'NONE', ( #11677, #10672, #23494, #20948 ) ) ;
#3041 = CARTESIAN_POINT ( 'NONE',  ( -7.078251931573406708, -38.93060825814203696, 34.59014398252958244 ) ) ;
#3042 = CARTESIAN_POINT ( 'NONE',  ( 1.833485406944043827, 14.63699153649359452, 144.3694338680885778 ) ) ;
#3043 = CARTESIAN_POINT ( 'NONE',  ( -1.619063947482197729, -2.489035965910479486, -46.30105812165547974 ) ) ;
#3044 = CARTESIAN_POINT ( 'NONE',  ( 26.11404676487257603, -113.2169081140374232, 1.130420376096734847 ) ) ;
#3045 = CARTESIAN_POINT ( 'NONE',  ( 109.1589550718175161, -0.007507020724820348372, 0.001014448720249620404 ) ) ;
#3046 = CARTESIAN_POINT ( 'NONE',  ( -1.323830074806771284, 2.318057800980712457, -46.01435746200690602 ) ) ;
#3047 = EDGE_LOOP ( 'NONE', ( #6635, #6862, #25887, #24554 ) ) ;
#3048 = CARTESIAN_POINT ( 'NONE',  ( 1.833838850093465700, 59.02146106675083104, 132.5643635152036097 ) ) ;
#3049 = CARTESIAN_POINT ( 'NONE',  ( 109.1587776205901861, 0.007328861771499511728, -8.330235398538848315E-05 ) ) ;
#3050 = CARTESIAN_POINT ( 'NONE',  ( -1.619063947482201282, 44.80407745103784123, -11.94059994246174838 ) ) ;
#3051 = CARTESIAN_POINT ( 'NONE',  ( 2.430230287190572103, 144.5585181921885862, 16.65331920325788317 ) ) ;
#3052 = CARTESIAN_POINT ( 'NONE',  ( 25.64660436782551400, -107.5626123667556442, -34.33930645842109897 ) ) ;
#3053 = ORIENTED_EDGE ( 'NONE', *, *, #21230, .T. ) ;
#3054 = CARTESIAN_POINT ( 'NONE',  ( 25.87036335909427009, -57.38512068812939759, -97.41424496619579543 ) ) ;
#3055 = ORIENTED_EDGE ( 'NONE', *, *, #15974, .T. ) ;
#3056 = ORIENTED_EDGE ( 'NONE', *, *, #27807, .T. ) ;
#3057 = ORIENTED_EDGE ( 'NONE', *, *, #24283, .F. ) ;
#3058 = CARTESIAN_POINT ( 'NONE',  ( -1.050230346682668126, 43.55729751025884156, 14.15335421912537583 ) ) ;
#3059 = B_SPLINE_CURVE_WITH_KNOTS ( 'NONE', 3,
 ( #3942, #28109, #12711, #21637, #21497, #1911, #10713 ),
 .UNSPECIFIED., .F., .F.,
 ( 4, 3, 4 ),
 ( 0.000000000000000000, 0.006568092053401818758, 0.02506242213020845946 ),
 .UNSPECIFIED. ) ;
#3060 = CARTESIAN_POINT ( 'NONE',  ( 19.66333377628720314, 123.9466021833770526, 60.10102584214407528 ) ) ;
#3061 = ADVANCED_FACE ( 'NONE', ( #21309 ), #5683, .F. ) ;
#3062 = ADVANCED_FACE ( 'NONE', ( #5927 ), #14139, .T. ) ;
#3063 = CARTESIAN_POINT ( 'NONE',  ( -8.786685647604894456, -23.24040270374358030, 48.22796981442792230 ) ) ;
#3064 = CARTESIAN_POINT ( 'NONE',  ( 1.894214914920914650, -14.22353624692096474, 144.4515288797483379 ) ) ;
#3065 = CARTESIAN_POINT ( 'NONE',  ( -1.155031165708882757, 2.068616213631583545, 45.85732438018710866 ) ) ;
#3066 = ADVANCED_FACE ( 'NONE', ( #17126 ), #27959, .T. ) ;
#3067 = CARTESIAN_POINT ( 'NONE',  ( 10.93730112725972070, -4.928439153521261495, 151.0983828010090804 ) ) ;
#3068 = CARTESIAN_POINT ( 'NONE',  ( -55.24271866751342941, -0.008433070970613520956, -0.004365563123939561994 ) ) ;
#3069 = B_SPLINE_CURVE_WITH_KNOTS ( 'NONE', 3,
 ( #26332, #19995, #26607, #566, #24475, #11496 ),
 .UNSPECIFIED., .F., .F.,
 ( 4, 2, 4 ),
 ( 0.000000000000000000, 0.0004335184443140181732, 0.0008670368886280363464 ),
 .UNSPECIFIED. ) ;
#3070 = CARTESIAN_POINT ( 'NONE',  ( 109.1589550718174877, -0.007507020724817397607, -0.001014448720240716502 ) ) ;
#3071 = EDGE_CURVE ( 'NONE', #2974, #18117, #17366, .T. ) ;
#3072 = CARTESIAN_POINT ( 'NONE',  ( -25.21435515916043713, 25.00736669481056751, 23.92354251275909505 ) ) ;
#3073 = CARTESIAN_POINT ( 'NONE',  ( 25.64699802086727587, -75.72889180797064057, -83.75009658924072653 ) ) ;
#3074 = CARTESIAN_POINT ( 'NONE',  ( 55.79472521941426777, 66.75682020267569783, -28.92526238350408008 ) ) ;
#3076 = CARTESIAN_POINT ( 'NONE',  ( 109.1721716018069657, 0.005466227998629004728, 0.01616973485710952382 ) ) ;
#3075 = CARTESIAN_POINT ( 'NONE',  ( -1.583189561560253589, 44.83405390829688741, 11.94859433442854701 ) ) ;
#3077 = CARTESIAN_POINT ( 'NONE',  ( 25.64692872815575342, 45.63107645358331155, 103.2799065540885834 ) ) ;
#3078 = CARTESIAN_POINT ( 'NONE',  ( 28.37599760073041821, 100.2461467136618012, -55.80522390574013514 ) ) ;
#3079 = CARTESIAN_POINT ( 'NONE',  ( 32.73300124599732186, 0.000000000000000000, 0.000000000000000000 ) ) ;
#3080 = ORIENTED_EDGE ( 'NONE', *, *, #15550, .F. ) ;
#3081 = FACE_OUTER_BOUND ( 'NONE', #27655, .T. ) ;
#3082 = ORIENTED_EDGE ( 'NONE', *, *, #14692, .F. ) ;
#3083 = CARTESIAN_POINT ( 'NONE',  ( 2.433796855181233454, -16.65276281464466024, -144.5536872373193660 ) ) ;
#3084 = CARTESIAN_POINT ( 'NONE',  ( 25.73574536432414916, -12.61003673871966235, 112.2643803187784926 ) ) ;
#3085 = VERTEX_POINT ( 'NONE', #19288 ) ;
#3086 = ORIENTED_EDGE ( 'NONE', *, *, #17960, .T. ) ;
#3087 = VERTEX_POINT ( 'NONE', #14546 ) ;
#3088 = CARTESIAN_POINT ( 'NONE',  ( 26.11404676487257603, -97.48350837663569735, -57.58742681967552102 ) ) ;
#3089 = CARTESIAN_POINT ( 'NONE',  ( 109.1586900883932856, 0.006757191295056129768, -0.002301750759607921679 ) ) ;
#3090 = EDGE_CURVE ( 'NONE', #704, #2885, #27925, .T. ) ;
#3091 = CARTESIAN_POINT ( 'NONE',  ( 10.93730112725932635, 0.000000000000000000, 0.000000000000000000 ) ) ;
#3092 = DIRECTION ( 'NONE',  ( 0.000000000000000000, 0.000000000000000000, 1.000000000000000000 ) ) ;
#3093 = CARTESIAN_POINT ( 'NONE',  ( -6.574463467970635300, 47.03022655117400319, -20.55340846381147202 ) ) ;
#3094 = EDGE_CURVE ( 'NONE', #13345, #18731, #9114, .T. ) ;
#3095 = CARTESIAN_POINT ( 'NONE',  ( -25.21435515916043713, -34.29329011225952684, 4.655591116594705703 ) ) ;
#3096 = CARTESIAN_POINT ( 'NONE',  ( -20.20700224038492365, 8.199606986804329978, -28.44216453106539078 ) ) ;
#3097 = CARTESIAN_POINT ( 'NONE',  ( 9.884929003653626367, 103.8128997986857627, 109.0134320167736774 ) ) ;
#3098 = CARTESIAN_POINT ( 'NONE',  ( 109.1586059443104944, -0.003294606663363280809, -0.006260042619939223604 ) ) ;
#3099 = DIRECTION ( 'NONE',  ( 0.5946245182733607137, -0.2512550613902274632, 0.7637359336799379728 ) ) ;
#3100 = CARTESIAN_POINT ( 'NONE',  ( -1.259972190295307604, -2.243354636026084759, -45.95417440459613800 ) ) ;
#3101 = ORIENTED_EDGE ( 'NONE', *, *, #2619, .F. ) ;
#3102 = ORIENTED_EDGE ( 'NONE', *, *, #15067, .T. ) ;
#3103 = CARTESIAN_POINT ( 'NONE',  ( 26.11404676487259024, 12.95861723607453619, 112.4785329405482628 ) ) ;
#3105 = CARTESIAN_POINT ( 'NONE',  ( 10.93730112725943293, 128.3908183996590537, 79.81734490845931873 ) ) ;
#3104 = CARTESIAN_POINT ( 'NONE',  ( 5.340103556456544887, 62.06990747183869672, -133.7487107983438364 ) ) ;
#3106 = CARTESIAN_POINT ( 'NONE',  ( -8.786685647604889127, 9.545808661480615243, -52.67761315067287597 ) ) ;
#3107 = B_SPLINE_CURVE_WITH_KNOTS ( 'NONE', 3,
 ( #1701, #26164, #1570, #6456, #16967, #15206, #8341, #13067, #21852, #10913 ),
 .UNSPECIFIED., .F., .F.,
 ( 4, 2, 2, 2, 4 ),
 ( 7.757919228897728493E-18, 0.0003346267210630983675, 0.0006692534421261890371, 0.001003880163189279761, 0.001338506884252370268 ),
 .UNSPECIFIED. ) ;
#3108 = CARTESIAN_POINT ( 'NONE',  ( 30.59138290137886784, -111.3296280985501312, -33.33271994911455494 ) ) ;
#3109 = EDGE_LOOP ( 'NONE', ( #13631, #9794, #13363, #1337 ) ) ;
#3110 = CARTESIAN_POINT ( 'NONE',  ( 1.832998868059858122, 125.9352106559994127, -72.09222286250950162 ) ) ;
#3111 = CARTESIAN_POINT ( 'NONE',  ( -55.24340739397742084, 0.006539691034612836289, -0.007744344507854826129 ) ) ;
#3112 = CARTESIAN_POINT ( 'NONE',  ( -1.463510566862823437, -38.76366072687759612, 25.15876608740857989 ) ) ;
#3113 = ORIENTED_EDGE ( 'NONE', *, *, #19740, .T. ) ;
#3114 = CARTESIAN_POINT ( 'NONE',  ( 109.1778270068192853, -0.007152128381195992091, -0.005967275455179304154 ) ) ;
#3115 = CARTESIAN_POINT ( 'NONE',  ( 25.73574536432415982, -112.4329083163019476, 11.00659994954114218 ) ) ;
#3116 = B_SPLINE_CURVE_WITH_KNOTS ( 'NONE', 3,
 ( #18438, #16434, #25520, #23074, #11969, #1310, #7371, #20743 ),
 .UNSPECIFIED., .F., .F.,
 ( 4, 2, 2, 4 ),
 ( 3.469446951953614189E-18, 0.0002429588503611279356, 0.0004859177007222524017, 0.0009718354014444825772 ),
 .UNSPECIFIED. ) ;
#3117 = CARTESIAN_POINT ( 'NONE',  ( 1.833206310202320388, -132.2594754479309245, 59.70089235435385433 ) ) ;
#3118 = EDGE_LOOP ( 'NONE', ( #9560, #21723, #11395, #9807 ) ) ;
#3119 = CARTESIAN_POINT ( 'NONE',  ( 1.832998868059890096, -45.34898734665952702, -137.8420662456174739 ) ) ;
#3120 = ORIENTED_EDGE ( 'NONE', *, *, #25561, .F. ) ;
#3121 = CARTESIAN_POINT ( 'NONE',  ( 25.65782528836481191, -45.39960327191544565, -103.3897864210300810 ) ) ;
#3122 = CARTESIAN_POINT ( 'NONE',  ( 32.73300124599738581, 3.836798148480494497, -117.5726003567928757 ) ) ;
#3123 = EDGE_CURVE ( 'NONE', #21594, #15548, #18760, .T. ) ;
#3124 = ORIENTED_EDGE ( 'NONE', *, *, #26063, .F. ) ;
#3125 = B_SPLINE_CURVE_WITH_KNOTS ( 'NONE', 3,
 ( #6709, #7416, #16182, #18324, #9566, #24989, #22828, #27104, #5245, #11869 ),
 .UNSPECIFIED., .F., .F.,
 ( 4, 3, 3, 4 ),
 ( 3.122502256758252770E-17, 0.0002669559177086159489, 0.0005339118354151012238, 0.001067817517169167719 ),
 .UNSPECIFIED. ) ;
#3126 = FACE_OUTER_BOUND ( 'NONE', #15413, .T. ) ;
#3127 = EDGE_CURVE ( 'NONE', #4329, #10668, #6679, .T. ) ;
#3128 = CARTESIAN_POINT ( 'NONE',  ( -20.20700224038492010, -18.19058640100240254, -23.35150625415651859 ) ) ;
#3129 = DIRECTION ( 'NONE',  ( 0.5946245182733607137, 0.5994612328333218665, -0.5357871896547430346 ) ) ;
#3130 = CARTESIAN_POINT ( 'NONE',  ( -7.078251931573406708, 20.86696228105292761, 47.71415099571781582 ) ) ;
#3131 = EDGE_CURVE ( 'NONE', #14400, #14753, #1873, .T. ) ;
#3132 = ORIENTED_EDGE ( 'NONE', *, *, #21352, .F. ) ;
#3133 = CARTESIAN_POINT ( 'NONE',  ( -1.048994561756802169, -14.87838255483227101, 43.31369460697990803 ) ) ;
#3135 = CARTESIAN_POINT ( 'NONE',  ( -55.25297051322618813, -0.01019003092403448357, -0.01093108995494832154 ) ) ;
#3134 = CARTESIAN_POINT ( 'NONE',  ( -1.155031165708884311, -25.28071330859858534, 38.31525684316168423 ) ) ;
#3136 = CARTESIAN_POINT ( 'NONE',  ( 2.433796855181205476, 107.1581411821785821, 98.43889364293895028 ) ) ;
#3137 = ORIENTED_EDGE ( 'NONE', *, *, #4526, .F. ) ;
#3138 = ORIENTED_EDGE ( 'NONE', *, *, #19330, .F. ) ;
#3139 = VERTEX_POINT ( 'NONE', #3467 ) ;
#3140 = CARTESIAN_POINT ( 'NONE',  ( 32.73300124599732186, 0.000000000000000000, 0.000000000000000000 ) ) ;
#3142 = CARTESIAN_POINT ( 'NONE',  ( 5.340103556456599954, 47.74933482044561828, -139.5040934094286911 ) ) ;
#3141 = CARTESIAN_POINT ( 'NONE',  ( 1.833809397773830563, 107.9565774559024760, -96.96506043213346970 ) ) ;
#3143 = CARTESIAN_POINT ( 'NONE',  ( -55.24300891470650754, 0.006048736206179803135, 0.007734635432136488173 ) ) ;
#3144 = EDGE_CURVE ( 'NONE', #15935, #16104, #24222, .T. ) ;
#3145 = CARTESIAN_POINT ( 'NONE',  ( -55.24271866751342941, 0.001425019990779444407, 0.009388511352200054269 ) ) ;
#3146 = CARTESIAN_POINT ( 'NONE',  ( -20.90916690077965256, -34.84883504600963988, -18.74041620980156253 ) ) ;
#3147 = EDGE_LOOP ( 'NONE', ( #27890, #19517, #27434, #12577 ) ) ;
#3148 = CARTESIAN_POINT ( 'NONE',  ( -1.239374126674604337, -38.61989855450958231, -25.08410696974230092 ) ) ;
#3149 = CARTESIAN_POINT ( 'NONE',  ( 25.65782528836480125, -66.83837989650129430, 91.01210296572919844 ) ) ;
#3150 = CARTESIAN_POINT ( 'NONE',  ( 109.1624594426973260, -0.01438905500501222109, -0.006914244825461785676 ) ) ;
#3151 = CARTESIAN_POINT ( 'NONE',  ( -20.20700224038492721, -27.82980252387812570, 10.08426345511618649 ) ) ;
#3153 = CARTESIAN_POINT ( 'NONE',  ( 109.1721716018069515, -0.008708654716135843035, 0.01467989464938419288 ) ) ;
#3152 = B_SPLINE_CURVE_WITH_KNOTS ( 'NONE', 3,
 ( #4072, #8268, #17031, #21788, #6121, #3940, #21633 ),
 .UNSPECIFIED., .F., .F.,
 ( 4, 3, 4 ),
 ( 0.000000000000000000, 0.006568092053401763247, 0.02506242213020846987 ),
 .UNSPECIFIED. ) ;
#3154 = VERTEX_POINT ( 'NONE', #25780 ) ;
#3155 = CARTESIAN_POINT ( 'NONE',  ( 25.69398547355842055, -12.54367966927970102, -112.2438548322124205 ) ) ;
#3156 = EDGE_CURVE ( 'NONE', #5981, #3564, #21091, .T. ) ;
#3157 = CARTESIAN_POINT ( 'NONE',  ( 19.66333377628710011, -105.3186440504701125, 88.78556591841261536 ) ) ;
#3158 = FACE_OUTER_BOUND ( 'NONE', #13040, .T. ) ;
#3159 = VERTEX_POINT ( 'NONE', #2564 ) ;
#3160 = ADVANCED_FACE ( 'NONE', ( #2003 ), #11722, .F. ) ;
#3161 = VERTEX_POINT ( 'NONE', #10803 ) ;
#3162 = EDGE_CURVE ( 'NONE', #20059, #23545, #13179, .T. ) ;
#3164 = B_SPLINE_CURVE_WITH_KNOTS ( 'NONE', 3,
 ( #18329, #5836, #16330, #14159, #20791, #18927 ),
 .UNSPECIFIED., .F., .F.,
 ( 4, 2, 4 ),
 ( 8.239936510889833698E-18, 0.0006311636237756815130, 0.001262327247551354786 ),
 .UNSPECIFIED. ) ;
#3163 = CARTESIAN_POINT ( 'NONE',  ( -1.045287976400365970, 45.76855895860946077, 1.530335034933974381 ) ) ;
#3165 = CARTESIAN_POINT ( 'NONE',  ( -12.94347594948497537, -42.93165645342824632, 23.08810053288727104 ) ) ;
#3166 = DIRECTION ( 'NONE',  ( -0.7563875759206388771, -0.4122509917856824191, -0.5078650950445610102 ) ) ;
#3167 = CLOSED_SHELL ( 'NONE', ( #18753, #4684, #22561, #27696, #11598, #26506, #7461, #16008, #9327, #16885, #16834, #22775, #20763, #6642, #18729, #23628, #8672, #27941, #12827, #25330, #21185, #19854, #25200, #8187, #8642, #8176, #3581, #6075, #3062, #25882, #1101, #13906, #7323, #16148, #15580, #4708, #2218, #24718, #12704, #2323, #18659, #7494, #8072, #14285, #5997, #26009, #5365, #18855, #11840, #8137, #4357, #19650, #20066, #18574, #15122, #751, #11151, #20659, #15636, #21842, #12574, #3066, #18459, #15255, #6582, #18763, #18811, #9280, #28479, #27051, #6381, #19809, #16253, #5568, #13477, #11668, #27335, #3678, #1211, #11744, #28209, #4000, #27883, #9234, #16179, #5093, #17129, #16936, #11575, #8033, #9503, #6285, #1150, #5910, #27254, #17820, #13023, #28274, #1569, #12932, #24520, #12897, #6813, #12764, #26962, #12811, #317, #15089, #17186, #8886, #13970, #14006, #27287, #9658, #17136, #3646, #14787, #14294, #26765, #12027, #11276, #22312, #25258, #3575, #24225, #4012, #26862, #19128, #10439, #19361, #27861, #2796, #11761, #20142, #19183, #12540, #19886, #4169, #13760, #4219, #6171, #14792, #23967, #26435, #20177, #3909, #20707, #21423, #5305, #5524, #4515, #1902, #17595, #5034, #15392, #23756, #21836, #14155, #4680, #21706, #25849, #12771, #9778, #10812, #19530, #22400, #4958, #21192, #3776, #11645, #13673, #2459, #3965, #171, #2043, #11464, #22912, #25171, #10442, #4899, #1187, #5859, #3487, #5344, #25911, #25335, #13060, #23294, #16734, #14878, #7973, #17910, #20923, #16261, #812, #15061, #1657, #9757, #11733, #22675, #16615, #9037, #4281, #16901, #23568, #17765, #21677, #27661, #4058, #14665, #4285, #13551, #903, #1029, #6606, #12192, #23937, #5833, #25749, #13057, #12877, #24812, #5029, #16316, #21957, #18629, #1796, #24686, #22048, #584, #953, #14495, #5096, #3323, #1439, #24096, #10423, #27929, #16699, #18919, #23624, #595, #21944, #7022, #13766, #12415, #11084, #25878, #22193, #4364, #24618, #9664, #9472, #23963, #8679, #21386, #22471, #17828, #24794, #8001, #15921, #20071, #2492, #9305, #9937, #7708, #13178, #2913, #23809, #15415, #26795, #26409, #25238, #15160, #11534, #27928, #15236, #16452, #8978, #13098, #15479, #9194, #5464, #7934, #14057, #14435, #4034, #26509, #27776, #4473, #26160, #14529, #27438, #19921, #25760, #20952, #6811, #21991, #8784, #18692, #16878, #4122, #21664, #25264, #1238, #12138, #6484, #5754, #9564, #5040, #15348, #11251, #27332, #4885, #22972, #12991, #20993, #7264, #17467, #14723, #4025, #3509, #486, #7002, #2007, #25974, #2759, #545, #5863, #20227, #2095, #2181, #2012, #15002, #15018, #783, #5240, #2384, #3061, #26241, #11436, #4973, #5133, #2165, #27030, #25048, #15029, #2784, #14858, #19469, #20202, #3356, #3457, #19081, #24091, #1117, #5672, #26866, #23995, #21166, #25376, #19052, #1880, #12043, #6706, #7389, #10107, #2016, #26511, #18526, #24840, #12678, #13093, #20349, #2557, #22430, #22475, #21455, #10401, #24040, #14031, #10646, #24982, #2103, #3877, #10303, #8616, #7612, #4296, #12349, #14218, #4541 ) ) ;
#3168 = CARTESIAN_POINT ( 'NONE',  ( 24.01988960052065991, -73.52806416354015084, -108.4726924928705927 ) ) ;
#3169 = CARTESIAN_POINT ( 'NONE',  ( 26.11404676487257603, -1.130420376097928115, 113.2169081140373947 ) ) ;
#3170 = CARTESIAN_POINT ( 'NONE',  ( 10.93730112725982195, -145.2260730187404079, 42.00474393596209666 ) ) ;
#3171 = CARTESIAN_POINT ( 'NONE',  ( 25.64699802086726876, 35.11755197949837992, 107.3112355540541643 ) ) ;
#3172 = FACE_OUTER_BOUND ( 'NONE', #10825, .T. ) ;
#3173 = ORIENTED_EDGE ( 'NONE', *, *, #16759, .F. ) ;
#3174 = ORIENTED_EDGE ( 'NONE', *, *, #3377, .T. ) ;
#3175 = CARTESIAN_POINT ( 'NONE',  ( -1.583189561560255143, -46.33203782964464068, -2.490696082059702832 ) ) ;
#3176 = FACE_OUTER_BOUND ( 'NONE', #8032, .T. ) ;
#3177 = CARTESIAN_POINT ( 'NONE',  ( 28.43349137099832191, -76.27296957774061070, -98.08682467580860020 ) ) ;
#3178 = DIRECTION ( 'NONE',  ( 0.000000000000000000, 0.000000000000000000, 1.000000000000000000 ) ) ;
#3179 = CARTESIAN_POINT ( 'NONE',  ( 109.1586059443104944, 0.005555961672773770607, -0.004378796245590031722 ) ) ;
#3180 = ORIENTED_EDGE ( 'NONE', *, *, #17166, .T. ) ;
#3181 = FACE_OUTER_BOUND ( 'NONE', #1759, .T. ) ;
#3182 = CARTESIAN_POINT ( 'NONE',  ( -1.050230347699842692, 5.964912479342754695E-15, -45.79907861674080749 ) ) ;
#3183 = CARTESIAN_POINT ( 'NONE',  ( 109.1586900883932856, 0.005715190711481724431, -0.004277182003227242291 ) ) ;
#3184 = B_SPLINE_CURVE_WITH_KNOTS ( 'NONE', 3,
 ( #19451, #28082, #14982, #14847 ),
 .UNSPECIFIED., .F., .F.,
 ( 4, 4 ),
 ( 3.254074918541991720E-16, 0.01077107486149803464 ),
 .UNSPECIFIED. ) ;
#3185 = CARTESIAN_POINT ( 'NONE',  ( -55.24271866751342941, 0.004365563123939758886, -0.008433070970614048312 ) ) ;
#3186 = DIRECTION ( 'NONE',  ( 0.000000000000000000, 0.000000000000000000, 1.000000000000000000 ) ) ;
#3187 = CARTESIAN_POINT ( 'NONE',  ( 25.64681081121879203, -110.3564950173083474, 23.88203588908045916 ) ) ;
#3188 = EDGE_CURVE ( 'NONE', #13254, #25142, #13354, .T. ) ;
#3189 = ORIENTED_EDGE ( 'NONE', *, *, #4158, .T. ) ;
#3190 = CARTESIAN_POINT ( 'NONE',  ( 1.833485406944057594, 145.1085452359073429, -0.5339064996889759662 ) ) ;
#3191 = ORIENTED_EDGE ( 'NONE', *, *, #14098, .T. ) ;
#3192 = ORIENTED_EDGE ( 'NONE', *, *, #24696, .T. ) ;
#3193 = EDGE_CURVE ( 'NONE', #8101, #17023, #26946, .T. ) ;
#3194 = ORIENTED_EDGE ( 'NONE', *, *, #12570, .T. ) ;
#3195 = CARTESIAN_POINT ( 'NONE',  ( 25.64681081121880624, 66.03065707438935306, 91.59071981940594753 ) ) ;
#3196 = EDGE_CURVE ( 'NONE', #22961, #12630, #7044, .T. ) ;
#3197 =( BOUNDED_SURFACE ( )  B_SPLINE_SURFACE ( 3, 1, ( 
 ( #23713, #21383 ),
 ( #12457, #27865 ),
 ( #8162, #10459 ),
 ( #25717, #6003 ) ),
 .UNSPECIFIED., .F., .F., .F. ) 
 B_SPLINE_SURFACE_WITH_KNOTS ( ( 4, 4 ),
 ( 2, 2 ),
 ( 0.000000000000000000, 1.000000000000000000 ),
 ( 0.000000000000000000, 1.000000000000000000 ),
 .UNSPECIFIED. ) 
 GEOMETRIC_REPRESENTATION_ITEM ( )  RATIONAL_B_SPLINE_SURFACE ( (
 ( 1.000000000000000000, 1.000000000000000000),
 ( 0.6386103224230316178, 0.9954351624131538845),
 ( 0.6386103224230316178, 0.9954351624131538845),
 ( 1.000000000000000000, 1.000000000000000000) ) ) 
 REPRESENTATION_ITEM ( '' )  SURFACE ( )  );
#3198 = DIRECTION ( 'NONE',  ( 0.000000000000000000, 0.000000000000000000, 1.000000000000000000 ) ) ;
#3199 = CARTESIAN_POINT ( 'NONE',  ( 32.73300124599732186, 0.000000000000000000, 0.000000000000000000 ) ) ;
#3200 = CARTESIAN_POINT ( 'NONE',  ( -25.21435515916043713, -25.00736669481004526, 23.92354251275963861 ) ) ;
#3201 = CARTESIAN_POINT ( 'NONE',  ( -24.53237795827029899, -24.99972053297889119, 22.94498492516371613 ) ) ;
#3202 = CARTESIAN_POINT ( 'NONE',  ( 109.1587776205901861, -0.006305329297950526372, 0.003736572840496112016 ) ) ;
#3203 = DIRECTION ( 'NONE',  ( 0.000000000000000000, 5.223019709707975211E-21, -1.000000000000000000 ) ) ;
#3204 = CARTESIAN_POINT ( 'NONE',  ( 6.224689322667630975, 12.92299475786958673, 147.4941644018828697 ) ) ;
#3205 = CARTESIAN_POINT ( 'NONE',  ( 8.186469829614358318, -108.6390983847743854, -102.4860667297607222 ) ) ;
#3206 = CARTESIAN_POINT ( 'NONE',  ( 1.833691583653525470, -85.00512109099176428, -117.6050685739178050 ) ) ;
#3207 = CARTESIAN_POINT ( 'NONE',  ( 30.59141879584311852, -33.33270905817506957, -111.3296561588017113 ) ) ;
#3208 = DIRECTION ( 'NONE',  ( -1.000000000000000000, -0.000000000000000000, -0.000000000000000000 ) ) ;
#3209 = FACE_OUTER_BOUND ( 'NONE', #1734, .T. ) ;
#3210 = DIRECTION ( 'NONE',  ( 0.7563875759206388771, -0.5490129373055229189, 0.3556158456312960015 ) ) ;
#3211 = CARTESIAN_POINT ( 'NONE',  ( 9.884929003653608603, -150.0922431698405717, 11.54837932062982198 ) ) ;
#3212 = CARTESIAN_POINT ( 'NONE',  ( 6.224689322667630975, -100.9623537450659114, 108.2965163446070704 ) ) ;
#3213 = CARTESIAN_POINT ( 'NONE',  ( 9.884929003653626367, 114.6392083957118047, 97.56484214660662246 ) ) ;
#3214 = ORIENTED_EDGE ( 'NONE', *, *, #16014, .T. ) ;
#3215 = DIRECTION ( 'NONE',  ( 0.7563875759206387661, 0.5490129373055256945, -0.3556158456312918936 ) ) ;
#3216 = EDGE_CURVE ( 'NONE', #6575, #15678, #5667, .T. ) ;
#3217 = CARTESIAN_POINT ( 'NONE',  ( -20.47566262905010248, 7.708089517695595028, 28.85746289809567600 ) ) ;
#3218 = CARTESIAN_POINT ( 'NONE',  ( 1.831572820252008738, 138.3111855986067269, -43.90210991190477330 ) ) ;
#3219 = ORIENTED_EDGE ( 'NONE', *, *, #26274, .T. ) ;
#3220 = EDGE_CURVE ( 'NONE', #16392, #12695, #22447, .T. ) ;
#3221 = EDGE_LOOP ( 'NONE', ( #10409, #1827, #15842, #20092 ) ) ;
#3222 = EDGE_LOOP ( 'NONE', ( #23248, #16246, #21655, #23486 ) ) ;
#3223 = EDGE_CURVE ( 'NONE', #4538, #14688, #17309, .T. ) ;
#3224 = B_SPLINE_CURVE_WITH_KNOTS ( 'NONE', 3,
 ( #7947, #3884, #18161, #21297, #20325, #23339, #5915, #20611, #16004, #13990 ),
 .UNSPECIFIED., .F., .F.,
 ( 4, 2, 2, 2, 4 ),
 ( 2.913600445039318278E-16, 0.0003346187017559116412, 0.0006692374035115318488, 0.001003856105267152219, 0.001338474807022772481 ),
 .UNSPECIFIED. ) ;
#3225 = VERTEX_POINT ( 'NONE', #8926 ) ;
#3226 = CARTESIAN_POINT ( 'NONE',  ( -55.24390624410018802, -0.009374879212970498032, 0.004572280736701721943 ) ) ;
#3227 = EDGE_CURVE ( 'NONE', #7560, #3533, #22492, .T. ) ;
#3228 = DIRECTION ( 'NONE',  ( 0.5946245182733608248, -0.7999021332774035598, 0.08110646981858252169 ) ) ;
#3229 =( BOUNDED_SURFACE ( )  B_SPLINE_SURFACE ( 3, 1, ( 
 ( #5124, #11890 ),
 ( #20946, #11754 ),
 ( #14323, #20521 ),
 ( #808, #9590 ) ),
 .UNSPECIFIED., .F., .F., .F. ) 
 B_SPLINE_SURFACE_WITH_KNOTS ( ( 4, 4 ),
 ( 2, 2 ),
 ( 0.000000000000000000, 1.000000000000000000 ),
 ( 0.000000000000000000, 1.000000000000000000 ),
 .UNSPECIFIED. ) 
 GEOMETRIC_REPRESENTATION_ITEM ( )  RATIONAL_B_SPLINE_SURFACE ( (
 ( 1.000000000000000000, 1.000000000000000000),
 ( 0.7789835883360578528, 0.9689951854195403280),
 ( 0.7789835883360578528, 0.9689951854195403280),
 ( 1.000000000000000000, 1.000000000000000000) ) ) 
 REPRESENTATION_ITEM ( '' )  SURFACE ( )  );
#3230 = CARTESIAN_POINT ( 'NONE',  ( 24.01988960052059241, -129.8107982898200135, -17.94039809062754287 ) ) ;
#3231 = CARTESIAN_POINT ( 'NONE',  ( -1.619063947482201282, 43.26576862488434472, -16.67502769180576649 ) ) ;
#3232 = CARTESIAN_POINT ( 'NONE',  ( 26.11404676487257603, -108.0249973236469572, 33.91085499298339556 ) ) ;
#3233 = FACE_OUTER_BOUND ( 'NONE', #5180, .T. ) ;
#3234 = VECTOR ( 'NONE', #6793, 1000.000000000000000 ) ;
#3235 = CARTESIAN_POINT ( 'NONE',  ( 25.70243777736188662, 35.59945151684219411, -107.1912711514951866 ) ) ;
#3236 = CARTESIAN_POINT ( 'NONE',  ( -1.259920593601976169, 28.82601305773653877, -35.85909937955931071 ) ) ;
#3237 = AXIS2_PLACEMENT_3D ( 'NONE', #24708, #27251, #22825 ) ;
#3238 = CARTESIAN_POINT ( 'NONE',  ( 1.833485406944043827, -30.69200235379031838, 141.8265699653866250 ) ) ;
#3240 = CARTESIAN_POINT ( 'NONE',  ( 55.49584447822657296, 22.67407039687332215, -68.91748907713565586 ) ) ;
#3239 = CARTESIAN_POINT ( 'NONE',  ( 2.263178113027039640, 60.41552743271138581, -132.2496129425953484 ) ) ;
#3241 = CARTESIAN_POINT ( 'NONE',  ( -1.155031165708883867, -2.068616213631259804, -45.85732438018710155 ) ) ;
#3242 = CIRCLE ( 'NONE', #20234, 117.6351876552689504 ) ;
#3243 = ORIENTED_EDGE ( 'NONE', *, *, #140, .F. ) ;
#3244 = ORIENTED_EDGE ( 'NONE', *, *, #9003, .F. ) ;
#3245 = FACE_OUTER_BOUND ( 'NONE', #2739, .T. ) ;
#3246 = LINE ( 'NONE', #18644, #27693 ) ;
#3247 = B_SPLINE_CURVE_WITH_KNOTS ( 'NONE', 3,
 ( #23296, #1119, #18673, #12329, #7757, #20963, #3418 ),
 .UNSPECIFIED., .F., .F.,
 ( 4, 3, 4 ),
 ( 4.946183070983774510E-16, 0.02816610861753248568, 0.04000277880656268742 ),
 .UNSPECIFIED. ) ;
#3248 = CARTESIAN_POINT ( 'NONE',  ( -20.21097721650788159, -23.76068422213743503, 17.67178726257384014 ) ) ;
#3249 = FACE_OUTER_BOUND ( 'NONE', #2821, .T. ) ;
#3250 = ORIENTED_EDGE ( 'NONE', *, *, #14119, .F. ) ;
#3251 = EDGE_LOOP ( 'NONE', ( #2472, #2061, #24855, #27914 ) ) ;
#3252 = CARTESIAN_POINT ( 'NONE',  ( 1.833691583653573209, 44.50270951807548414, 138.1170938425793224 ) ) ;
#3253 = CARTESIAN_POINT ( 'NONE',  ( 25.64681081121879203, -35.28660243342475411, -107.2555980796244910 ) ) ;
#3254 = CARTESIAN_POINT ( 'NONE',  ( 109.1592201516379674, 0.001934867487021726170, 0.007620268632971113378 ) ) ;
#3255 = EDGE_LOOP ( 'NONE', ( #26348, #17389, #1106, #11172 ) ) ;
#3256 = CARTESIAN_POINT ( 'NONE',  ( -22.23342874802667168, -7.677086057585177592, -30.68433055777678931 ) ) ;
#3257 = EDGE_CURVE ( 'NONE', #26408, #19554, #26588, .T. ) ;
#3258 = B_SPLINE_CURVE_WITH_KNOTS ( 'NONE', 3,
 ( #12331, #14346, #10345, #25463, #16940, #5875, #27585, #21397, #6165, #6019 ),
 .UNSPECIFIED., .F., .F.,
 ( 4, 2, 2, 2, 4 ),
 ( 2.976962515321448001E-16, 0.0003346187017559152190, 0.0006692374035115327162, 0.001003856105267150267, 0.001338474807022767710 ),
 .UNSPECIFIED. ) ;
#3259 = CARTESIAN_POINT ( 'NONE',  ( 25.98107933586750917, -112.6229961579372230, 10.73978443746694289 ) ) ;
#3260 = EDGE_CURVE ( 'NONE', #9397, #13041, #12536, .T. ) ;
#3261 = CIRCLE ( 'NONE', #25343, 34.60786435723138510 ) ;
#3262 = CARTESIAN_POINT ( 'NONE',  ( -1.619063947482197729, 2.489035965910801895, 46.30105812165545842 ) ) ;
#3263 = AXIS2_PLACEMENT_3D ( 'NONE', #16073, #26579, #24878 ) ;
#3264 = VERTEX_POINT ( 'NONE', #5158 ) ;
#3265 = CARTESIAN_POINT ( 'NONE',  ( 109.1586059443104944, 0.001740416220259405171, 0.006856640434643077389 ) ) ;
#3266 = AXIS2_PLACEMENT_3D ( 'NONE', #13498, #6894, #15223 ) ;
#3267 = VERTEX_POINT ( 'NONE', #20694 ) ;
#3268 = CARTESIAN_POINT ( 'NONE',  ( -20.57838717382308147, 25.16001208503129760, 16.28767523336092893 ) ) ;
#3269 = CARTESIAN_POINT ( 'NONE',  ( 25.64660436782558861, 112.3516544824819334, 11.22538561721926342 ) ) ;
#3270 = ORIENTED_EDGE ( 'NONE', *, *, #20098, .T. ) ;
#3271 = DIRECTION ( 'NONE',  ( 0.5866777222776488054, 0.8024104850197666394, 0.1093007946606648212 ) ) ;
#3272 = CARTESIAN_POINT ( 'NONE',  ( 30.59138290137872218, 101.9665464510086537, 55.75105126023953517 ) ) ;
#3273 = CARTESIAN_POINT ( 'NONE',  ( -1.050230346682689664, 14.15203301556493010, 43.55772679531834513 ) ) ;
#3274 = CARTESIAN_POINT ( 'NONE',  ( 24.01988960052032951, 123.2441023955621091, 44.53753990739565438 ) ) ;
#3275 = ORIENTED_EDGE ( 'NONE', *, *, #23416, .T. ) ;
#3276 = FACE_OUTER_BOUND ( 'NONE', #28306, .T. ) ;
#3278 = CARTESIAN_POINT ( 'NONE',  ( -55.24728320129491266, -0.005114031043466088153, -0.01362040845703062046 ) ) ;
#3277 = CARTESIAN_POINT ( 'NONE',  ( 1.833691583653537016, 85.58103979054644128, -117.1866391460177397 ) ) ;
#3279 = CARTESIAN_POINT ( 'NONE',  ( -16.86833981943424376, -30.57013526701942041, -31.95666732167553548 ) ) ;
#3280 = ORIENTED_EDGE ( 'NONE', *, *, #7138, .T. ) ;
#3281 = ORIENTED_EDGE ( 'NONE', *, *, #26808, .T. ) ;
#3282 = ORIENTED_EDGE ( 'NONE', *, *, #18431, .F. ) ;
#3283 = DIRECTION ( 'NONE',  ( 1.000000000000000000, -6.938893903907226837E-18, 1.734723475976806709E-18 ) ) ;
#3284 = CARTESIAN_POINT ( 'NONE',  ( 32.73300124599735028, 66.00340565729339914, 97.37344512919882789 ) ) ;
#3286 = CARTESIAN_POINT ( 'NONE',  ( 2.433796855181205476, -142.0211193075553524, -31.67151202413115385 ) ) ;
#3285 = DIRECTION ( 'NONE',  ( 0.000000000000000000, 0.000000000000000000, 1.000000000000000000 ) ) ;
#3287 = VECTOR ( 'NONE', #5979, 1000.000000000000227 ) ;
#3288 = CARTESIAN_POINT ( 'NONE',  ( 25.64681081121879203, -11.38886654529598275, -112.3352186517031726 ) ) ;
#3289 = CARTESIAN_POINT ( 'NONE',  ( -25.21435515916025594, 1.749597353048488237E-16, -4.373993382621220594E-17 ) ) ;
#3290 = CARTESIAN_POINT ( 'NONE',  ( 1.833838850855487923, 107.7780290788696789, 97.16351016225925719 ) ) ;
#3291 = CARTESIAN_POINT ( 'NONE',  ( 10.93730112725972781, -92.80059208661754155, 119.3442956573269100 ) ) ;
#3292 = ORIENTED_EDGE ( 'NONE', *, *, #15708, .F. ) ;
#3293 = DIRECTION ( 'NONE',  ( 0.000000000000000000, 5.223019709707975211E-21, -1.000000000000000000 ) ) ;
#3294 = CARTESIAN_POINT ( 'NONE',  ( -55.24271866751342941, 0.004256484107793635611, 0.008488649505346116536 ) ) ;
#3295 = CARTESIAN_POINT ( 'NONE',  ( -1.155031165708884533, 44.25214473648929925, 12.20332162035416879 ) ) ;
#3296 = CARTESIAN_POINT ( 'NONE',  ( 25.73574536432414206, 74.99093179013968324, 84.49061642666495686 ) ) ;
#3297 = CARTESIAN_POINT ( 'NONE',  ( 109.1586900883932856, 0.005371970278523967128, -0.004701023939953873770 ) ) ;
#3298 = CARTESIAN_POINT ( 'NONE',  ( 8.186469829614264171, -122.8338389144551996, 84.95702201190503899 ) ) ;
#3299 = EDGE_CURVE ( 'NONE', #7211, #22124, #6037, .T. ) ;
#3300 = ORIENTED_EDGE ( 'NONE', *, *, #15709, .F. ) ;
#3301 = CARTESIAN_POINT ( 'NONE',  ( 1.831572820252009626, -137.7011124121620469, 45.77972211429768379 ) ) ;
#3302 = CARTESIAN_POINT ( 'NONE',  ( 28.37599760073042532, -45.02094138570515014, -105.5302221302111150 ) ) ;
#3303 = EDGE_CURVE ( 'NONE', #11177, #25953, #26103, .T. ) ;
#3304 = CARTESIAN_POINT ( 'NONE',  ( 21.16825799904930605, 59.09063383105323908, 121.8625396241595240 ) ) ;
#3305 = EDGE_CURVE ( 'NONE', #27642, #17966, #16686, .T. ) ;
#3306 = ORIENTED_EDGE ( 'NONE', *, *, #11705, .F. ) ;
#3307 = ORIENTED_EDGE ( 'NONE', *, *, #4289, .T. ) ;
#3308 = VECTOR ( 'NONE', #12721, 1000.000000000000000 ) ;
#3309 = CARTESIAN_POINT ( 'NONE',  ( -8.786685647604894456, -23.24040270374358030, 48.22796981442792230 ) ) ;
#3310 = CARTESIAN_POINT ( 'NONE',  ( 109.1589550718174877, 0.0005685167901298389739, 0.007553890059312249293 ) ) ;
#3311 = CIRCLE ( 'NONE', #6996, 117.6351876552689504 ) ;
#3312 = CARTESIAN_POINT ( 'NONE',  ( 109.1721716018069515, -0.001984900887706775655, 0.01695288006056417870 ) ) ;
#3313 = CARTESIAN_POINT ( 'NONE',  ( 25.64681081121879203, 97.57530875170684226, -56.81519825470653018 ) ) ;
#3314 = CARTESIAN_POINT ( 'NONE',  ( 2.430230287190581429, 145.5073573687466819, 1.451610819318244650 ) ) ;
#3315 = CARTESIAN_POINT ( 'NONE',  ( -55.24300891470648622, -0.009439835024157194193, 0.002702093572889528381 ) ) ;
#3316 = CARTESIAN_POINT ( 'NONE',  ( 25.87036335909429496, -45.07965203034989798, 103.6841944152904489 ) ) ;
#3317 = ORIENTED_EDGE ( 'NONE', *, *, #26214, .T. ) ;
#3318 = B_SPLINE_CURVE_WITH_KNOTS ( 'NONE', 3,
 ( #20450, #22484, #9390, #14105, #18141, #11678, #20301, #4910, #15986, #22924 ),
 .UNSPECIFIED., .F., .F.,
 ( 4, 2, 2, 2, 4 ),
 ( 2.863532086325413454E-16, 0.0003346187017559064912, 0.0006692374035115266446, 0.001003856105267146798, 0.001338474807022767060 ),
 .UNSPECIFIED. ) ;
#3319 = ORIENTED_EDGE ( 'NONE', *, *, #2099, .F. ) ;
#3320 = CARTESIAN_POINT ( 'NONE',  ( -1.113427685307007087, 42.96952363574832390, -16.03057832159165486 ) ) ;
#3321 = FACE_OUTER_BOUND ( 'NONE', #24203, .T. ) ;
#3322 = CARTESIAN_POINT ( 'NONE',  ( 109.1586059443104944, 0.004935564877218401141, -0.005067816690893759031 ) ) ;
#3323 = ADVANCED_FACE ( 'NONE', ( #15951 ), #25528, .F. ) ;
#3324 = CARTESIAN_POINT ( 'NONE',  ( -1.463510566862832318, 2.430838777910187432, -46.14841196428340453 ) ) ;
#3325 = CARTESIAN_POINT ( 'NONE',  ( -1.046935749539990468, -45.77872888003169294, -1.275486069320314497 ) ) ;
#3326 = VERTEX_POINT ( 'NONE', #11791 ) ;
#3327 = CARTESIAN_POINT ( 'NONE',  ( -1.056502255334265339, 14.64009593116102614, -43.40574022158779144 ) ) ;
#3328 = DIRECTION ( 'NONE',  ( -1.000000000000000000, -0.000000000000000000, -0.000000000000000000 ) ) ;
#3329 = CARTESIAN_POINT ( 'NONE',  ( -1.539763995773681726, -25.17088606276573515, -38.84665165401054310 ) ) ;
#3330 = EDGE_CURVE ( 'NONE', #7007, #23103, #22855, .T. ) ;
#3331 = CARTESIAN_POINT ( 'NONE',  ( -25.21435515916025594, 1.749597353048488237E-16, -4.373993382621220594E-17 ) ) ;
#3332 = VECTOR ( 'NONE', #3853, 1000.000000000000000 ) ;
#3333 = VERTEX_POINT ( 'NONE', #25176 ) ;
#3334 = CARTESIAN_POINT ( 'NONE',  ( 25.69398547355839213, -57.11291030433587679, -97.43788956976209192 ) ) ;
#3335 = CARTESIAN_POINT ( 'NONE',  ( 32.73300124599739291, -105.8473486001047235, -51.32617430725011332 ) ) ;
#3336 = EDGE_LOOP ( 'NONE', ( #23435, #26824, #26553, #26062, #28440, #24937 ) ) ;
#3337 = ORIENTED_EDGE ( 'NONE', *, *, #10894, .T. ) ;
#3338 = VERTEX_POINT ( 'NONE', #9624 ) ;
#3339 = CARTESIAN_POINT ( 'NONE',  ( 25.64670758986457955, -107.5375791514045574, 34.41755235608707864 ) ) ;
#3340 = CARTESIAN_POINT ( 'NONE',  ( 32.73300124599732186, 0.000000000000000000, 0.000000000000000000 ) ) ;
#3341 = UNCERTAINTY_MEASURE_WITH_UNIT (LENGTH_MEASURE( 1.000000000000000082E-05 ), #24443, 'distance_accuracy_value', 'NONE');
#3342 = CARTESIAN_POINT ( 'NONE',  ( 2.433796855181205476, -133.5135467655521779, 57.85512797797844087 ) ) ;
#3343 = CARTESIAN_POINT ( 'NONE',  ( 1.833485406944057594, -125.9346397303430223, -72.09189602597842850 ) ) ;
#3344 = AXIS2_PLACEMENT_3D ( 'NONE', #19606, #15272, #2316 ) ;
#3345 = VECTOR ( 'NONE', #4434, 1000.000000000000000 ) ;
#3346 = CARTESIAN_POINT ( 'NONE',  ( 16.05277956358235159, 142.9335921074867315, 10.32496049470132782 ) ) ;
#3347 = CARTESIAN_POINT ( 'NONE',  ( 26.11404676487257603, 108.0249973236472130, -33.91085499298264239 ) ) ;
#3348 = CARTESIAN_POINT ( 'NONE',  ( 8.186469777910776457, 49.43817851234059191, 140.9315935720371158 ) ) ;
#3349 = EDGE_CURVE ( 'NONE', #3421, #2445, #11509, .T. ) ;
#3350 = CARTESIAN_POINT ( 'NONE',  ( 10.93730112725990367, -142.1801301103781157, -51.37919228020433593 ) ) ;
#3351 = CARTESIAN_POINT ( 'NONE',  ( -20.57838717382308147, 16.28767523336157552, 25.16001208503087838 ) ) ;
#3352 = DIRECTION ( 'NONE',  ( 1.000000000000000000, -6.938893903907226837E-18, 1.734723475976806709E-18 ) ) ;
#3353 = EDGE_CURVE ( 'NONE', #11913, #4019, #14574, .T. ) ;
#3354 = B_SPLINE_CURVE_WITH_KNOTS ( 'NONE', 3,
 ( #3681, #21521, #19220, #19360 ),
 .UNSPECIFIED., .F., .F.,
 ( 4, 4 ),
 ( 0.000000000000000000, 0.008383560773332708604 ),
 .UNSPECIFIED. ) ;
#3355 = CARTESIAN_POINT ( 'NONE',  ( 26.11404676487259024, -83.38016054979834735, 76.59696442953165274 ) ) ;
#3356 = ADVANCED_FACE ( 'NONE', ( #22595 ), #11545, .F. ) ;
#3357 = CARTESIAN_POINT ( 'NONE',  ( 26.04756280548355463, -22.44333019059074985, 110.9306483680202007 ) ) ;
#3358 = CARTESIAN_POINT ( 'NONE',  ( 109.1778270068192853, -0.004958088776549044938, -0.007885345421917355421 ) ) ;
#3359 = B_SPLINE_CURVE_WITH_KNOTS ( 'NONE', 3,
 ( #16162, #5224, #13996, #16598, #22809, #20909, #1198 ),
 .UNSPECIFIED., .F., .F.,
 ( 4, 3, 4 ),
 ( 4.718224631282382674E-16, 0.02816610861753243364, 0.04000277880656261109 ),
 .UNSPECIFIED. ) ;
#3360 = DIRECTION ( 'NONE',  ( -5.541455922705464902E-20, 5.223019709708320524E-21, -1.000000000000000000 ) ) ;
#3361 = CARTESIAN_POINT ( 'NONE',  ( -7.733045908741340568, -10.42750254442575120, -51.44704017882771296 ) ) ;
#3362 = ORIENTED_EDGE ( 'NONE', *, *, #18564, .F. ) ;
#3363 = CIRCLE ( 'NONE', #13024, 53.53553390275978785 ) ;
#3364 = CARTESIAN_POINT ( 'NONE',  ( -1.113427685306993320, 25.34053733836532274, -38.22586258295203265 ) ) ;
#3365 = ORIENTED_EDGE ( 'NONE', *, *, #19125, .F. ) ;
#3366 = CARTESIAN_POINT ( 'NONE',  ( -20.57838717382308147, 7.715628353034087894, 28.96176188950209962 ) ) ;
#3367 = CARTESIAN_POINT ( 'NONE',  ( -1.049817751779889008, 26.50542916749622080, 37.35030165458145746 ) ) ;
#3368 = ORIENTED_EDGE ( 'NONE', *, *, #18461, .T. ) ;
#3369 =( BOUNDED_SURFACE ( )  B_SPLINE_SURFACE ( 3, 1, ( 
 ( #24659, #7092 ),
 ( #20306, #15852 ),
 ( #5049, #20159 ),
 ( #13541, #4915 ) ),
 .UNSPECIFIED., .F., .F., .F. ) 
 B_SPLINE_SURFACE_WITH_KNOTS ( ( 4, 4 ),
 ( 2, 2 ),
 ( 0.000000000000000000, 1.000000000000000000 ),
 ( 0.000000000000000000, 1.000000000000000000 ),
 .UNSPECIFIED. ) 
 GEOMETRIC_REPRESENTATION_ITEM ( )  RATIONAL_B_SPLINE_SURFACE ( (
 ( 1.000000000000000000, 1.000000000000000000),
 ( 0.9956975270656955868, 0.8568959468854907557),
 ( 0.9956975270656955868, 0.8568959468854907557),
 ( 1.000000000000000000, 1.000000000000000000) ) ) 
 REPRESENTATION_ITEM ( '' )  SURFACE ( )  );
#3370 = ORIENTED_EDGE ( 'NONE', *, *, #4451, .T. ) ;
#3371 = VECTOR ( 'NONE', #4270, 1000.000000000000114 ) ;
#3372 = ORIENTED_EDGE ( 'NONE', *, *, #13795, .F. ) ;
#3373 = CARTESIAN_POINT ( 'NONE',  ( 2.430230287190581429, -16.65331920325836634, 144.5585181921885294 ) ) ;
#3374 = B_SPLINE_CURVE_WITH_KNOTS ( 'NONE', 3,
 ( #19117, #16679, #14643, #25473, #3562, #5747 ),
 .UNSPECIFIED., .F., .F.,
 ( 4, 2, 4 ),
 ( 1.344410693882025498E-17, 0.0006311636237756689362, 0.001262327247551324428 ),
 .UNSPECIFIED. ) ;
#3375 = AXIS2_PLACEMENT_3D ( 'NONE', #16537, #22602, #5309 ) ;
#3376 = LINE ( 'NONE', #12159, #17698 ) ;
#3377 = EDGE_CURVE ( 'NONE', #14092, #5592, #25221, .T. ) ;
#3378 = CARTESIAN_POINT ( 'NONE',  ( 180.4657679828686980, -1.252232817320263489E-15, 3.130582043300658722E-16 ) ) ;
#3379 = CARTESIAN_POINT ( 'NONE',  ( -1.155001620486255209, 28.62773628245669499, -35.88346938217563320 ) ) ;
#3380 = CARTESIAN_POINT ( 'NONE',  ( -28.41354790283022069, 14.62505768302800924, -18.00456980371904692 ) ) ;
#3381 = CARTESIAN_POINT ( 'NONE',  ( 1.831572820252009626, -31.13525033585391100, -141.7320553118909174 ) ) ;
#3383 = CARTESIAN_POINT ( 'NONE',  ( 2.108393763691196021, 57.92353377304286965, 133.2474712570796100 ) ) ;
#3382 = CARTESIAN_POINT ( 'NONE',  ( -20.47566338032525124, 10.72601609985066062, 27.87687989047296711 ) ) ;
#3384 = EDGE_CURVE ( 'NONE', #4901, #342, #23517, .T. ) ;
#3385 = ORIENTED_EDGE ( 'NONE', *, *, #10867, .F. ) ;
#3386 = ORIENTED_EDGE ( 'NONE', *, *, #9896, .T. ) ;
#3387 = CARTESIAN_POINT ( 'NONE',  ( 2.433796855181205476, 144.8571464219891141, -13.76554153471544417 ) ) ;
#3389 = CARTESIAN_POINT ( 'NONE',  ( -1.259920593601967287, 25.19630221849107343, 38.49623866863322519 ) ) ;
#3388 = CARTESIAN_POINT ( 'NONE',  ( 25.64708010899965984, 66.32331961783506813, -91.37928813995102928 ) ) ;
#3390 = CARTESIAN_POINT ( 'NONE',  ( 2.433796855181233454, 109.1007109081226076, 96.28145139437721411 ) ) ;
#3391 = B_SPLINE_CURVE_WITH_KNOTS ( 'NONE', 3,
 ( #9110, #16446, #16005, #5503 ),
 .UNSPECIFIED., .F., .F.,
 ( 4, 4 ),
 ( 1.895855152355442610E-16, 0.001982023823822949386 ),
 .UNSPECIFIED. ) ;
#3392 =( NAMED_UNIT ( * ) PLANE_ANGLE_UNIT ( ) SI_UNIT ( $, .RADIAN. ) );
#3393 = VERTEX_POINT ( 'NONE', #20124 ) ;
#3394 = EDGE_CURVE ( 'NONE', #16076, #19079, #6591, .T. ) ;
#3395 = ORIENTED_EDGE ( 'NONE', *, *, #10331, .F. ) ;
#3396 = CARTESIAN_POINT ( 'NONE',  ( 1.894214914920974380, 137.7482714433630520, -45.75988301372497347 ) ) ;
#3397 = CARTESIAN_POINT ( 'NONE',  ( -1.259920593601994376, 35.85909937955963755, 28.82601305773611600 ) ) ;
#3398 = CARTESIAN_POINT ( 'NONE',  ( 10.93730112725990011, -146.7718404940640653, -36.23586118136687162 ) ) ;
#3399 = ORIENTED_EDGE ( 'NONE', *, *, #672, .T. ) ;
#3400 = CARTESIAN_POINT ( 'NONE',  ( -7.078251931573406708, 11.16394717458676311, -50.86685171665416050 ) ) ;
#3401 = DIRECTION ( 'NONE',  ( 0.5914120900931444380, -0.6942916636548135401, -0.4101107478122094641 ) ) ;
#3402 = AXIS2_PLACEMENT_3D ( 'NONE', #11010, #15159, #28267 ) ;
#3403 = ORIENTED_EDGE ( 'NONE', *, *, #13698, .F. ) ;
#3404 =( BOUNDED_SURFACE ( )  B_SPLINE_SURFACE ( 3, 1, ( 
 ( #12742, #6286 ),
 ( #23857, #4247 ),
 ( #4108, #21671 ),
 ( #1943, #10749 ) ),
 .UNSPECIFIED., .F., .F., .F. ) 
 B_SPLINE_SURFACE_WITH_KNOTS ( ( 4, 4 ),
 ( 2, 2 ),
 ( 0.000000000000000000, 1.000000000000000000 ),
 ( 0.000000000000000000, 1.000000000000000000 ),
 .UNSPECIFIED. ) 
 GEOMETRIC_REPRESENTATION_ITEM ( )  RATIONAL_B_SPLINE_SURFACE ( (
 ( 1.000000000000000000, 1.000000000000000000),
 ( 0.9593753223639863714, 0.9995975284513187731),
 ( 0.9593753223639863714, 0.9995975284513187731),
 ( 1.000000000000000000, 1.000000000000000000) ) ) 
 REPRESENTATION_ITEM ( '' )  SURFACE ( )  );
#3405 = ORIENTED_EDGE ( 'NONE', *, *, #1306, .F. ) ;
#3406 = CARTESIAN_POINT ( 'NONE',  ( -1.583189561560252701, -29.24830400313139478, 36.01941156322819637 ) ) ;
#3407 = ORIENTED_EDGE ( 'NONE', *, *, #24876, .F. ) ;
#3408 = CARTESIAN_POINT ( 'NONE',  ( 109.1589550718174877, -0.004632048724973759565, 0.005994046294307789347 ) ) ;
#3409 = B_SPLINE_CURVE_WITH_KNOTS ( 'NONE', 3,
 ( #5869, #10195, #23579, #969, #16661, #5426, #18669, #9905, #14628, #12466 ),
 .UNSPECIFIED., .F., .F.,
 ( 4, 3, 3, 4 ),
 ( 3.925231146709437917E-17, 0.0002669559177086530829, 0.0005339118354151471939, 0.001067817517169176392 ),
 .UNSPECIFIED. ) ;
#3410 = B_SPLINE_CURVE_WITH_KNOTS ( 'NONE', 3,
 ( #9258, #6967, #24533, #4932, #11271, #8976, #2770 ),
 .UNSPECIFIED., .F., .F.,
 ( 4, 3, 4 ),
 ( 0.000000000000000000, 0.02398743853561340067, 0.04000277880656219476 ),
 .UNSPECIFIED. ) ;
#3411 = FACE_OUTER_BOUND ( 'NONE', #23043, .T. ) ;
#3412 = EDGE_CURVE ( 'NONE', #2885, #16498, #2914, .T. ) ;
#3413 = CARTESIAN_POINT ( 'NONE',  ( 13.36082413113061307, -94.94363694444135149, 119.8836995922723219 ) ) ;
#3414 = CARTESIAN_POINT ( 'NONE',  ( 1.831572820252009626, 31.13525033585493418, 141.7320553118907185 ) ) ;
#3415 = EDGE_CURVE ( 'NONE', #11749, #16457, #3618, .T. ) ;
#3416 = ORIENTED_EDGE ( 'NONE', *, *, #27147, .T. ) ;
#3417 = CARTESIAN_POINT ( 'NONE',  ( -1.046935749539995131, -15.35946454248365711, 43.14401153755482454 ) ) ;
#3419 = CARTESIAN_POINT ( 'NONE',  ( 109.1778270068192853, 0.007885345421917369299, -0.004958088776549021519 ) ) ;
#3418 = CARTESIAN_POINT ( 'NONE',  ( 32.73300124599737160, -117.3295799645428872, -8.473903470907334423 ) ) ;
#3420 = DIRECTION ( 'NONE',  ( 1.000000000000000000, 0.000000000000000000, 0.000000000000000000 ) ) ;
#3421 = VERTEX_POINT ( 'NONE', #23180 ) ;
#3422 = EDGE_CURVE ( 'NONE', #4347, #9246, #27623, .T. ) ;
#3423 = ORIENTED_EDGE ( 'NONE', *, *, #27690, .T. ) ;
#3424 = ORIENTED_EDGE ( 'NONE', *, *, #24280, .F. ) ;
#3425 = CARTESIAN_POINT ( 'NONE',  ( -1.019300379054419725, 44.15350047934416011, 12.21833869579419130 ) ) ;
#3426 = CARTESIAN_POINT ( 'NONE',  ( 1.832998868059890096, -137.8420662456167065, -45.34898734666185049 ) ) ;
#3428 = DIRECTION ( 'NONE',  ( 0.000000000000000000, 1.000000000000000000, 0.000000000000000000 ) ) ;
#3427 = CARTESIAN_POINT ( 'NONE',  ( 2.430230287190589422, 16.65331920325738935, 144.5585181921886715 ) ) ;
#3429 = CARTESIAN_POINT ( 'NONE',  ( -1.583189561560256253, -44.83405390829680215, -11.94859433442884900 ) ) ;
#3430 = CARTESIAN_POINT ( 'NONE',  ( -25.21435515916043713, -30.48034229288627017, 16.39063784838775462 ) ) ;
#3431 = ORIENTED_EDGE ( 'NONE', *, *, #21749, .T. ) ;
#3432 = CARTESIAN_POINT ( 'NONE',  ( -22.34422965417124018, -27.39717383755262148, 26.20925041532883881 ) ) ;
#3434 = EDGE_CURVE ( 'NONE', #4384, #17500, #18026, .T. ) ;
#3433 = CARTESIAN_POINT ( 'NONE',  ( -25.21435515916043713, -30.48034229288650820, -16.39063784838731053 ) ) ;
#3435 = ORIENTED_EDGE ( 'NONE', *, *, #22243, .T. ) ;
#3436 = CARTESIAN_POINT ( 'NONE',  ( -1.045287976400362417, -43.05558670614257721, -15.59869763335051651 ) ) ;
#3437 = CARTESIAN_POINT ( 'NONE',  ( -23.77929240705207192, 4.877832571065432887, 35.93174012244165283 ) ) ;
#3438 = CARTESIAN_POINT ( 'NONE',  ( -1.050231094221210082, 13.91061116148191878, -43.63617436699743024 ) ) ;
#3439 = CARTESIAN_POINT ( 'NONE',  ( 109.1586900883932856, 0.004701023939953854688, 0.005371970278523982741 ) ) ;
#3440 = CARTESIAN_POINT ( 'NONE',  ( 25.64681081121879203, -110.5293738517610080, 23.06870491922286348 ) ) ;
#3441 = CARTESIAN_POINT ( 'NONE',  ( -20.57838717382308147, 25.16001208503129760, 16.28767523336092893 ) ) ;
#3442 = VERTEX_POINT ( 'NONE', #1406 ) ;
#3443 = B_SPLINE_CURVE_WITH_KNOTS ( 'NONE', 3,
 ( #12890, #21535, #13171, #4261, #13042, #8587, #26140 ),
 .UNSPECIFIED., .F., .F.,
 ( 4, 3, 4 ),
 ( 3.642919299551294898E-17, 0.02816610861753245099, 0.04000277880656211149 ),
 .UNSPECIFIED. ) ;
#3444 = CARTESIAN_POINT ( 'NONE',  ( 25.98552792386798771, 110.4352299692913419, -24.57669147553878020 ) ) ;
#3445 = CARTESIAN_POINT ( 'NONE',  ( 6.224689322667647851, -57.86870174583520310, 136.2818611715188979 ) ) ;
#3446 = ORIENTED_EDGE ( 'NONE', *, *, #815, .T. ) ;
#3447 = DIRECTION ( 'NONE',  ( -0.7637818620346801257, -0.02150485345385289709, -0.6451161201712178883 ) ) ;
#3448 = CARTESIAN_POINT ( 'NONE',  ( 109.1592201516379674, -0.007856029051022764623, 0.0003082430542016628347 ) ) ;
#3449 = CARTESIAN_POINT ( 'NONE',  ( 2.263178113027040972, 73.90841366068559637, -125.2099934853443415 ) ) ;
#3450 = CARTESIAN_POINT ( 'NONE',  ( 1.832998868059858122, 108.1944082009157455, 96.70023740551157232 ) ) ;
#3451 = CARTESIAN_POINT ( 'NONE',  ( 25.64708228042120197, -23.51409906510289005, 110.4357030047557231 ) ) ;
#3452 = CARTESIAN_POINT ( 'NONE',  ( 28.43349137099834678, 58.58376153369862038, -109.5743306972600664 ) ) ;
#3453 = CARTESIAN_POINT ( 'NONE',  ( 25.98552792386798060, 74.89816102339827353, -84.79516057869801671 ) ) ;
#3454 = EDGE_CURVE ( 'NONE', #22293, #4663, #25615, .T. ) ;
#3455 = CARTESIAN_POINT ( 'NONE',  ( 8.186469777910909684, -77.65916160569824456, -127.5731248346295672 ) ) ;
#3456 = DIRECTION ( 'NONE',  ( -1.000000000000000000, -0.000000000000000000, -0.000000000000000000 ) ) ;
#3457 = ADVANCED_FACE ( 'NONE', ( #12346 ), #14482, .F. ) ;
#3458 = ORIENTED_EDGE ( 'NONE', *, *, #3806, .F. ) ;
#3459 = CARTESIAN_POINT ( 'NONE',  ( 1.833603222531986487, -30.60504697399307261, 141.8454679205786420 ) ) ;
#3460 = CARTESIAN_POINT ( 'NONE',  ( -1.058473599757830730, 42.99101666105228503, -15.81436910992533029 ) ) ;
#3461 = CARTESIAN_POINT ( 'NONE',  ( 55.79472521941426777, 23.17337251492855188, -68.96476385670641207 ) ) ;
#3462 = EDGE_CURVE ( 'NONE', #213, #174, #10294, .T. ) ;
#3463 = CARTESIAN_POINT ( 'NONE',  ( -1.044556982611273277, 12.57890920527776224, -44.03203163107531282 ) ) ;
#3464 = CARTESIAN_POINT ( 'NONE',  ( 109.1589550718175161, 0.007270618150635350940, 0.002126635388718555592 ) ) ;
#3465 = CARTESIAN_POINT ( 'NONE',  ( -8.786685647604887350, 53.04920435127183254, -7.199674155859138835 ) ) ;
#3466 = ORIENTED_EDGE ( 'NONE', *, *, #22943, .F. ) ;
#3467 = CARTESIAN_POINT ( 'NONE',  ( 25.64681081121879203, 107.2555980796245905, -35.28660243342437752 ) ) ;
#3468 = CARTESIAN_POINT ( 'NONE',  ( 1.831572820252008738, -137.7011124121613932, -45.77972211429954541 ) ) ;
#3469 = DIRECTION ( 'NONE',  ( 0.5914120900931444380, -0.2415416038592965442, -0.7693434820005542463 ) ) ;
#3470 = EDGE_LOOP ( 'NONE', ( #13657, #215, #12701, #12281 ) ) ;
#3471 = CARTESIAN_POINT ( 'NONE',  ( 25.64699802086723679, -75.37548011155783456, 84.06830990999306152 ) ) ;
#3472 = CARTESIAN_POINT ( 'NONE',  ( 109.1589550718174877, 0.004632048724973717932, -0.005994046294307822306 ) ) ;
#3473 = ORIENTED_EDGE ( 'NONE', *, *, #13404, .T. ) ;
#3474 = VERTEX_POINT ( 'NONE', #16530 ) ;
#3475 = ORIENTED_EDGE ( 'NONE', *, *, #22028, .F. ) ;
#3476 = CARTESIAN_POINT ( 'NONE',  ( 26.11404676487257603, -108.0249973236469572, 33.91085499298339556 ) ) ;
#3477 = CARTESIAN_POINT ( 'NONE',  ( 109.1587776205901577, 0.007297420966928596861, -0.0006832286435102698360 ) ) ;
#3478 = CARTESIAN_POINT ( 'NONE',  ( -4.473127245936431073, 18.25038884639870673, -45.82513704981550262 ) ) ;
#3479 = EDGE_CURVE ( 'NONE', #20262, #15935, #14841, .T. ) ;
#3480 = B_SPLINE_CURVE_WITH_KNOTS ( 'NONE', 3,
 ( #15717, #4796, #468, #22362 ),
 .UNSPECIFIED., .F., .F.,
 ( 4, 4 ),
 ( 3.360511874109859618E-16, 0.01077107486149756280 ),
 .UNSPECIFIED. ) ;
#3481 = CARTESIAN_POINT ( 'NONE',  ( -8.786685647604896232, 25.35688121747570278, 47.14957014837326454 ) ) ;
#3482 = CARTESIAN_POINT ( 'NONE',  ( -20.57838717382308147, -1.611677988432151709, 29.92853265176832878 ) ) ;
#3483 = CARTESIAN_POINT ( 'NONE',  ( -12.82751273423876803, -48.09651489336695107, -8.715310691360061313 ) ) ;
#3484 = EDGE_CURVE ( 'NONE', #19144, #10778, #13905, .T. ) ;
#3485 = CARTESIAN_POINT ( 'NONE',  ( 1.833721034905629654, 132.7087680342067983, 58.69612512971652052 ) ) ;
#3486 = CARTESIAN_POINT ( 'NONE',  ( 25.64681081121879203, -84.18689316040098447, 75.24277141833462679 ) ) ;
#3487 = ADVANCED_FACE ( 'NONE', ( #11420 ), #17418, .F. ) ;
#3488 = CARTESIAN_POINT ( 'NONE',  ( -20.90916690077963125, 18.74041620980169043, -34.84883504600955462 ) ) ;
#3489 = CARTESIAN_POINT ( 'NONE',  ( -20.20700224038492721, -27.82980252387812570, 10.08426345511618649 ) ) ;
#3490 = CARTESIAN_POINT ( 'NONE',  ( 25.64681081121879203, 97.99105938548001404, -56.09509703373240797 ) ) ;
#3491 = CARTESIAN_POINT ( 'NONE',  ( 109.1592201516379674, 0.001934867487012827689, -0.007620268632968149602 ) ) ;
#3492 = CARTESIAN_POINT ( 'NONE',  ( -55.24390624410018802, -0.004572280736702649152, 0.009374879212966917563 ) ) ;
#3493 = LINE ( 'NONE', #25245, #21636 ) ;
#3494 = CARTESIAN_POINT ( 'NONE',  ( 25.64681081121879203, -0.4157506337719985012, -112.9102952884414606 ) ) ;
#3495 = CARTESIAN_POINT ( 'NONE',  ( -4.473127245936434626, 12.17046501147516224, -47.80062405537804437 ) ) ;
#3496 = CARTESIAN_POINT ( 'NONE',  ( 32.73300124599741423, 113.0038235389606314, -32.68291970228113996 ) ) ;
#3497 = VERTEX_POINT ( 'NONE', #21045 ) ;
#3498 = CARTESIAN_POINT ( 'NONE',  ( 9.884929003653626367, 35.39789245780329452, 146.3148513795968029 ) ) ;
#3499 = ORIENTED_EDGE ( 'NONE', *, *, #14692, .T. ) ;
#3500 = CARTESIAN_POINT ( 'NONE',  ( -1.031422197589711764, -15.60268798220608488, 43.06660437151322895 ) ) ;
#3501 = CARTESIAN_POINT ( 'NONE',  ( 109.1589550718175161, -0.005477029346534963497, 0.005233222325307145852 ) ) ;
#3502 = ORIENTED_EDGE ( 'NONE', *, *, #5174, .T. ) ;
#3503 = B_SPLINE_CURVE_WITH_KNOTS ( 'NONE', 3,
 ( #21568, #10641, #5770, #19409, #14527, #4291, #17663, #21856, #6460, #13071 ),
 .UNSPECIFIED., .F., .F.,
 ( 4, 3, 3, 4 ),
 ( 3.469446951953614189E-17, 0.0002669559177086241347, 0.0005339118354150929838, 0.001067817517169170104 ),
 .UNSPECIFIED. ) ;
#3504 = ORIENTED_EDGE ( 'NONE', *, *, #24803, .F. ) ;
#3505 = ORIENTED_EDGE ( 'NONE', *, *, #11144, .F. ) ;
#3506 = EDGE_CURVE ( 'NONE', #16392, #15825, #496, .T. ) ;
#3507 = CARTESIAN_POINT ( 'NONE',  ( -1.239374126674604337, 16.50008610789360119, 42.99367564261261521 ) ) ;
#3508 = CARTESIAN_POINT ( 'NONE',  ( -55.24390624410018802, 0.009209468562452933355, 0.004896917417131438528 ) ) ;
#3509 = ADVANCED_FACE ( 'NONE', ( #12693 ), #14660, .F. ) ;
#3510 = EDGE_CURVE ( 'NONE', #10441, #28137, #804, .T. ) ;
#3511 = CARTESIAN_POINT ( 'NONE',  ( 28.37599760073041821, -109.6580863494832272, 33.74340001061066374 ) ) ;
#3512 = CARTESIAN_POINT ( 'NONE',  ( -20.57838717382308147, 29.92853265176831812, -1.611677988432464126 ) ) ;
#3513 = CARTESIAN_POINT ( 'NONE',  ( -20.20700224038492365, 10.08426345511628597, 27.82980252387807951 ) ) ;
#3514 = CARTESIAN_POINT ( 'NONE',  ( 2.063896406836605024, -145.2631347824382431, -1.344106060021882598 ) ) ;
#3515 = CARTESIAN_POINT ( 'NONE',  ( 25.81918753295377300, -112.5005889664128631, -10.88546493098971268 ) ) ;
#3516 = ORIENTED_EDGE ( 'NONE', *, *, #5650, .T. ) ;
#3517 = ORIENTED_EDGE ( 'NONE', *, *, #25233, .F. ) ;
#3518 = CARTESIAN_POINT ( 'NONE',  ( 25.64699802086727587, -107.4581924007662082, -34.66526531169749603 ) ) ;
#3520 = CARTESIAN_POINT ( 'NONE',  ( 109.1586900883932856, -0.005371970278528676035, -0.004701023939945692814 ) ) ;
#3519 = CARTESIAN_POINT ( 'NONE',  ( -7.711401346138175406, -45.70592430511711513, -25.75361633141480766 ) ) ;
#3521 = CARTESIAN_POINT ( 'NONE',  ( -20.37983603106074426, -7.753708011498764208, -28.74620395171560006 ) ) ;
#3522 = B_SPLINE_CURVE_WITH_KNOTS ( 'NONE', 3,
 ( #27917, #16273, #25355, #16419 ),
 .UNSPECIFIED., .F., .F.,
 ( 4, 4 ),
 ( 0.000000000000000000, 0.008383560773332699931 ),
 .UNSPECIFIED. ) ;
#3523 = CARTESIAN_POINT ( 'NONE',  ( 2.430230287190589422, -1.451610819316722312, -145.5073573687467103 ) ) ;
#3524 = CARTESIAN_POINT ( 'NONE',  ( -20.38016308990357928, -16.25718651464962861, 24.94368798801368925 ) ) ;
#3525 =( BOUNDED_SURFACE ( )  B_SPLINE_SURFACE ( 3, 1, ( 
 ( #13622, #11615 ),
 ( #2686, #20236 ),
 ( #674, #9323 ),
 ( #25582, #10461 ) ),
 .UNSPECIFIED., .F., .F., .F. ) 
 B_SPLINE_SURFACE_WITH_KNOTS ( ( 4, 4 ),
 ( 2, 2 ),
 ( 0.000000000000000000, 1.000000000000000000 ),
 ( 0.000000000000000000, 1.000000000000000000 ),
 .UNSPECIFIED. ) 
 GEOMETRIC_REPRESENTATION_ITEM ( )  RATIONAL_B_SPLINE_SURFACE ( (
 ( 1.000000000000000000, 1.000000000000000000),
 ( 0.9960225298536222738, 0.9999952330161893110),
 ( 0.9960225298536222738, 0.9999952330161893110),
 ( 1.000000000000000000, 1.000000000000000000) ) ) 
 REPRESENTATION_ITEM ( '' )  SURFACE ( )  );
#3526 = VERTEX_POINT ( 'NONE', #10549 ) ;
#3527 = DIRECTION ( 'NONE',  ( 0.000000000000000000, -1.000000000000000000, 0.000000000000000000 ) ) ;
#3528 = CARTESIAN_POINT ( 'NONE',  ( 6.224689322667630975, 43.30635742325379312, 141.5842213414014736 ) ) ;
#3529 = CARTESIAN_POINT ( 'NONE',  ( 1.833691583653539903, -15.52203496789013748, 144.2771263798446739 ) ) ;
#3530 = ORIENTED_EDGE ( 'NONE', *, *, #8951, .T. ) ;
#3531 = CARTESIAN_POINT ( 'NONE',  ( 25.64681081121879203, -97.57530875170644435, 56.81519825470720519 ) ) ;
#3532 = CARTESIAN_POINT ( 'NONE',  ( -1.323439229708128551, -38.58845475799787295, -25.17120723334079457 ) ) ;
#3533 = VERTEX_POINT ( 'NONE', #10291 ) ;
#3534 = ORIENTED_EDGE ( 'NONE', *, *, #25339, .F. ) ;
#3535 = EDGE_CURVE ( 'NONE', #15977, #5184, #2415, .T. ) ;
#3536 = EDGE_CURVE ( 'NONE', #16728, #27632, #25901, .T. ) ;
#3537 = EDGE_CURVE ( 'NONE', #20148, #5123, #12135, .T. ) ;
#3538 = VERTEX_POINT ( 'NONE', #12410 ) ;
#3539 = DIRECTION ( 'NONE',  ( 0.5946245182733607137, -0.7870422510449677223, 0.1642747008466114989 ) ) ;
#3540 = ITEM_DEFINED_TRANSFORMATION ( 'NONE', 'NONE', #8424,  #27263 ) ;
#3541 = CARTESIAN_POINT ( 'NONE',  ( -1.539760825549682188, -44.72358953107742252, -11.93465943778497262 ) ) ;
#3542 = CARTESIAN_POINT ( 'NONE',  ( 32.73300124599732186, 0.000000000000000000, 0.000000000000000000 ) ) ;
#3543 = CARTESIAN_POINT ( 'NONE',  ( 1.894214914920972603, 138.3376769255508520, 43.94587946447450832 ) ) ;
#3544 = FACE_OUTER_BOUND ( 'NONE', #2531, .T. ) ;
#3545 = CARTESIAN_POINT ( 'NONE',  ( 10.93730112725936898, 142.1801301103782578, 51.37919228020297879 ) ) ;
#3546 = ORIENTED_EDGE ( 'NONE', *, *, #4636, .F. ) ;
#3547 = CARTESIAN_POINT ( 'NONE',  ( 2.430230287190572103, -13.76600171652544624, -144.8619874886008176 ) ) ;
#3549 = CARTESIAN_POINT ( 'NONE',  ( -1.113427685307001314, -45.82016658690749722, 1.967672929087657785 ) ) ;
#3548 = LINE ( 'NONE', #8174, #23112 ) ;
#3550 = FACE_OUTER_BOUND ( 'NONE', #21894, .T. ) ;
#3551 = ORIENTED_EDGE ( 'NONE', *, *, #1109, .F. ) ;
#3552 = B_SPLINE_CURVE_WITH_KNOTS ( 'NONE', 3,
 ( #18730, #24935, #27060, #5486 ),
 .UNSPECIFIED., .F., .F.,
 ( 4, 4 ),
 ( 1.606470082347908540E-16, 0.008383748772659627146 ),
 .UNSPECIFIED. ) ;
#3553 = ORIENTED_EDGE ( 'NONE', *, *, #19586, .F. ) ;
#3554 = ORIENTED_EDGE ( 'NONE', *, *, #24357, .T. ) ;
#3555 = LINE ( 'NONE', #20969, #19339 ) ;
#3556 = CARTESIAN_POINT ( 'NONE',  ( 10.93730112725932635, 0.000000000000000000, 0.000000000000000000 ) ) ;
#3558 = CARTESIAN_POINT ( 'NONE',  ( 2.433796855181205476, 46.34326152018925171, -137.9325382748280333 ) ) ;
#3557 = CARTESIAN_POINT ( 'NONE',  ( -8.786685647604890903, -52.67761315067279781, 9.545808661481174795 ) ) ;
#3559 = CARTESIAN_POINT ( 'NONE',  ( -25.21435515916043357, 31.17620025257608418, 15.02493970636113474 ) ) ;
#3560 = CARTESIAN_POINT ( 'NONE',  ( -10.86508079875781618, 35.35100740321776414, -36.95527278096538737 ) ) ;
#3561 = ORIENTED_EDGE ( 'NONE', *, *, #9009, .F. ) ;
#3562 = CARTESIAN_POINT ( 'NONE',  ( 1.833206308920056538, 71.90885838897399651, 126.0392061186624773 ) ) ;
#3563 = CARTESIAN_POINT ( 'NONE',  ( 109.1586900883932856, -0.005371970278528676035, -0.004701023939945692814 ) ) ;
#3564 = VERTEX_POINT ( 'NONE', #2031 ) ;
#3565 = CARTESIAN_POINT ( 'NONE',  ( 9.884929003653608603, 139.1775604444711973, -57.36421526887020406 ) ) ;
#3566 = CARTESIAN_POINT ( 'NONE',  ( -20.38016308990357928, 1.509191766064626128, 29.73560196176844173 ) ) ;
#3567 =( BOUNDED_SURFACE ( )  B_SPLINE_SURFACE ( 3, 1, ( 
 ( #23878, #4132 ),
 ( #2825, #20519 ),
 ( #17913, #2672 ),
 ( #11603, #22851 ) ),
 .UNSPECIFIED., .F., .F., .F. ) 
 B_SPLINE_SURFACE_WITH_KNOTS ( ( 4, 4 ),
 ( 2, 2 ),
 ( 0.000000000000000000, 1.000000000000000000 ),
 ( 0.000000000000000000, 1.000000000000000000 ),
 .UNSPECIFIED. ) 
 GEOMETRIC_REPRESENTATION_ITEM ( )  RATIONAL_B_SPLINE_SURFACE ( (
 ( 1.000000000000000000, 1.000000000000000000),
 ( 0.7789835883360578528, 0.9689951854195403280),
 ( 0.7789835883360578528, 0.9689951854195403280),
 ( 1.000000000000000000, 1.000000000000000000) ) ) 
 REPRESENTATION_ITEM ( '' )  SURFACE ( )  );
#3568 = CARTESIAN_POINT ( 'NONE',  ( -1.045287976400365970, 44.00138577190666922, 12.68782741917247670 ) ) ;
#3569 = CARTESIAN_POINT ( 'NONE',  ( 109.1586900883932856, -0.002995460350180849298, 0.006479576224403778457 ) ) ;
#3570 = CARTESIAN_POINT ( 'NONE',  ( -9.156249394959706578, -53.74753343182696597, 9.022661520478342467 ) ) ;
#3571 = CARTESIAN_POINT ( 'NONE',  ( 1.833485406944043827, -108.1939177044932592, 96.69979900902130510 ) ) ;
#3572 = CARTESIAN_POINT ( 'NONE',  ( 25.69398547355841345, -84.42756928260523352, -75.02007992711791928 ) ) ;
#3573 = ORIENTED_EDGE ( 'NONE', *, *, #10163, .F. ) ;
#3574 = CARTESIAN_POINT ( 'NONE',  ( 10.93730112726002623, 65.95960219663321311, -136.0306644680977683 ) ) ;
#3575 = ADVANCED_FACE ( 'NONE', ( #21201 ), #26250, .F. ) ;
#3576 = CARTESIAN_POINT ( 'NONE',  ( 1.833485406944043827, 144.3694338680886915, -14.63699153649211127 ) ) ;
#3577 = CARTESIAN_POINT ( 'NONE',  ( 16.05277956358197144, 128.9466020665984161, -62.52511797225994172 ) ) ;
#3578 = EDGE_CURVE ( 'NONE', #5939, #2880, #26079, .T. ) ;
#3579 = ORIENTED_EDGE ( 'NONE', *, *, #18568, .T. ) ;
#3580 = CARTESIAN_POINT ( 'NONE',  ( -55.25719721206881729, 0.007063345920777610795, -0.008651607285660192076 ) ) ;
#3581 = ADVANCED_FACE ( 'NONE', ( #10419 ), #19445, .T. ) ;
#3582 = CARTESIAN_POINT ( 'NONE',  ( 26.11404676487257603, -67.46175819463425682, 90.92995828888176391 ) ) ;
#3583 = FACE_OUTER_BOUND ( 'NONE', #24155, .T. ) ;
#3584 = ADVANCED_FACE ( 'NONE', ( #27956 ), #1102, .F. ) ;
#3585 = CARTESIAN_POINT ( 'NONE',  ( -1.046936909428679563, -12.93351869073243243, 43.93225665392628088 ) ) ;
#3586 = CARTESIAN_POINT ( 'NONE',  ( 2.430230287190592531, -145.5073573687466819, 1.451610819317235013 ) ) ;
#3587 = CARTESIAN_POINT ( 'NONE',  ( 1.833838848569431246, 137.9525894882063426, -45.01064392477788800 ) ) ;
#3588 = CARTESIAN_POINT ( 'NONE',  ( 19.66333377628701840, 99.30798531455356226, 95.46107873288919166 ) ) ;
#3589 = CARTESIAN_POINT ( 'NONE',  ( -55.24728320129491266, -0.003868537197316565448, -0.01402509393918558236 ) ) ;
#3590 = LINE ( 'NONE', #5216, #22185 ) ;
#3591 = AXIS2_PLACEMENT_3D ( 'NONE', #3601, #12799, #16566 ) ;
#3592 = CARTESIAN_POINT ( 'NONE',  ( 2.108393763691167155, -16.46048390411897344, 144.3574619851892180 ) ) ;
#3593 = ORIENTED_EDGE ( 'NONE', *, *, #19676, .F. ) ;
#3594 = ORIENTED_EDGE ( 'NONE', *, *, #22532, .F. ) ;
#3595 = CARTESIAN_POINT ( 'NONE',  ( -1.323439229708139431, -43.04565903621273293, 16.42345129173381935 ) ) ;
#3596 = CARTESIAN_POINT ( 'NONE',  ( 10.93730112725990367, -92.80059208661606363, -119.3442956573281748 ) ) ;
#3597 = CARTESIAN_POINT ( 'NONE',  ( -1.048171036023497704, 13.17819047681665090, 43.86077206077055735 ) ) ;
#3598 = CARTESIAN_POINT ( 'NONE',  ( 2.430230287190581429, 137.9371479820462696, 46.34481016236870943 ) ) ;
#3599 = CARTESIAN_POINT ( 'NONE',  ( 55.79472521941426777, 72.27573336313952268, 8.328398066092010055 ) ) ;
#3600 = VERTEX_POINT ( 'NONE', #24217 ) ;
#3601 = CARTESIAN_POINT ( 'NONE',  ( 10.93730112725932635, 0.000000000000000000, 0.000000000000000000 ) ) ;
#3602 = CARTESIAN_POINT ( 'NONE',  ( 21.16825799904904315, -59.09063383105261380, -121.8625396241603056 ) ) ;
#3603 = CARTESIAN_POINT ( 'NONE',  ( 109.1592201516379674, 0.007566779963318552571, -0.002134489919774391464 ) ) ;
#3604 = B_SPLINE_CURVE_WITH_KNOTS ( 'NONE', 3,
 ( #3778, #17007, #19039, #12139, #27816, #1194 ),
 .UNSPECIFIED., .F., .F.,
 ( 4, 2, 4 ),
 ( 1.550807859811640467E-16, 0.003570751334075634390, 0.007141502668151113523 ),
 .UNSPECIFIED. ) ;
#3605 = B_SPLINE_CURVE_WITH_KNOTS ( 'NONE', 3,
 ( #18776, #5694, #23263, #18165, #26943, #22509 ),
 .UNSPECIFIED., .F., .F.,
 ( 4, 2, 4 ),
 ( 3.709064347514218400E-16, 0.003576372551511170905, 0.007152745103021971446 ),
 .UNSPECIFIED. ) ;
#3606 = CARTESIAN_POINT ( 'NONE',  ( 55.49584447822657296, 62.96491934286042635, -36.04376091928477166 ) ) ;
#3607 = CARTESIAN_POINT ( 'NONE',  ( 16.75465622695661239, -140.0080030360328180, 25.01894884133809427 ) ) ;
#3608 = VERTEX_POINT ( 'NONE', #17429 ) ;
#3609 = CARTESIAN_POINT ( 'NONE',  ( 2.263178607246689733, -46.26071628252355339, -137.8402782326816123 ) ) ;
#3610 = CARTESIAN_POINT ( 'NONE',  ( 32.73300124599735739, 51.32617430724909013, 105.8473486001052777 ) ) ;
#3611 = ORIENTED_EDGE ( 'NONE', *, *, #223, .T. ) ;
#3612 = ADVANCED_FACE ( 'NONE', ( #4625 ), #4040, .F. ) ;
#3613 =( BOUNDED_SURFACE ( )  B_SPLINE_SURFACE ( 3, 1, ( 
 ( #22684, #2953 ),
 ( #16324, #9713 ),
 ( #5385, #27103 ),
 ( #22973, #26966 ) ),
 .UNSPECIFIED., .F., .F., .F. ) 
 B_SPLINE_SURFACE_WITH_KNOTS ( ( 4, 4 ),
 ( 2, 2 ),
 ( 0.000000000000000000, 1.000000000000000000 ),
 ( 0.000000000000000000, 1.000000000000000000 ),
 .UNSPECIFIED. ) 
 GEOMETRIC_REPRESENTATION_ITEM ( )  RATIONAL_B_SPLINE_SURFACE ( (
 ( 1.000000000000000000, 1.000000000000000000),
 ( 0.7789835883360578528, 0.9689951854195403280),
 ( 0.7789835883360578528, 0.9689951854195403280),
 ( 1.000000000000000000, 1.000000000000000000) ) ) 
 REPRESENTATION_ITEM ( '' )  SURFACE ( )  );
#3614 = ORIENTED_EDGE ( 'NONE', *, *, #8710, .F. ) ;
#3615 = CONICAL_SURFACE ( 'NONE', #19685, 34.60786435723138510, 0.8559913436420825139 ) ;
#3616 = EDGE_LOOP ( 'NONE', ( #3250, #1865, #667, #27436 ) ) ;
#3617 = EDGE_CURVE ( 'NONE', #8000, #11148, #8373, .T. ) ;
#3618 = B_SPLINE_CURVE_WITH_KNOTS ( 'NONE', 3,
 ( #15295, #27758, #23447, #20852, #8555, #3710 ),
 .UNSPECIFIED., .F., .F.,
 ( 4, 2, 4 ),
 ( 9.875766617722657020E-18, 0.0006311571484586093669, 0.001262314296917208976 ),
 .UNSPECIFIED. ) ;
#3619 = CARTESIAN_POINT ( 'NONE',  ( -55.25719721206881729, 0.004044147484875269816, -0.01041086141212288138 ) ) ;
#3620 = CARTESIAN_POINT ( 'NONE',  ( 32.73300124599741423, -92.86301839379967760, -72.21147546950645335 ) ) ;
#3621 = CARTESIAN_POINT ( 'NONE',  ( 55.49584447822657296, -14.82242356767884672, -71.02133150427270891 ) ) ;
#3622 = CARTESIAN_POINT ( 'NONE',  ( 109.1624594426973118, -0.01263706729759551950, 0.009754804742280919622 ) ) ;
#3623 = CARTESIAN_POINT ( 'NONE',  ( -55.24271866751342941, -0.006757859501005985571, -0.006671293903669251422 ) ) ;
#3624 = CARTESIAN_POINT ( 'NONE',  ( 109.1721716018069657, 0.009868622090676173672, -0.01392660302850758265 ) ) ;
#3625 = DIRECTION ( 'NONE',  ( 0.000000000000000000, 0.000000000000000000, 1.000000000000000000 ) ) ;
#3626 = DIRECTION ( 'NONE',  ( -1.000000000000000000, -0.000000000000000000, -0.000000000000000000 ) ) ;
#3627 = CARTESIAN_POINT ( 'NONE',  ( -21.41427618760458174, -11.22988868156165410, 28.68857606049978415 ) ) ;
#3628 = CARTESIAN_POINT ( 'NONE',  ( 25.64681081121879203, -12.21581276189883170, 112.2483031020013016 ) ) ;
#3629 = CARTESIAN_POINT ( 'NONE',  ( 25.64681081121879203, -112.9102952884414464, -0.4157506337739698132 ) ) ;
#3630 = DIRECTION ( 'NONE',  ( 0.000000000000000000, 0.000000000000000000, 1.000000000000000000 ) ) ;
#3632 = CARTESIAN_POINT ( 'NONE',  ( 2.433796855181233454, 125.2830755159764777, -74.00833731765430912 ) ) ;
#3631 = CARTESIAN_POINT ( 'NONE',  ( 13.36082413113061307, -151.2941478187906341, -22.28175172543715732 ) ) ;
#3633 = CARTESIAN_POINT ( 'NONE',  ( -22.23342874802668234, -16.78332232459660389, -26.81018246605532340 ) ) ;
#3634 = CARTESIAN_POINT ( 'NONE',  ( 1.833485406944043827, -0.5339064996894915538, 145.1085452359073145 ) ) ;
#3635 = ORIENTED_EDGE ( 'NONE', *, *, #19535, .T. ) ;
#3636 = ORIENTED_EDGE ( 'NONE', *, *, #6568, .F. ) ;
#3637 = CARTESIAN_POINT ( 'NONE',  ( 32.73300124599735739, -20.69176323058707823, 115.8010721414082980 ) ) ;
#3639 = ORIENTED_EDGE ( 'NONE', *, *, #26965, .T. ) ;
#3638 = CARTESIAN_POINT ( 'NONE',  ( 1.832998868059858122, 138.1720401012273101, -44.33343224355090939 ) ) ;
#3640 = ORIENTED_EDGE ( 'NONE', *, *, #10331, .T. ) ;
#3641 = EDGE_CURVE ( 'NONE', #27505, #2120, #5290, .T. ) ;
#3642 = EDGE_LOOP ( 'NONE', ( #11235, #26460, #7786, #1287 ) ) ;
#3643 = B_SPLINE_CURVE_WITH_KNOTS ( 'NONE', 3,
 ( #13570, #26949, #19912, #11280, #22373, #15573, #17604, #26387 ),
 .UNSPECIFIED., .F., .F.,
 ( 4, 2, 2, 4 ),
 ( 0.000000000000000000, 0.0002429588503611229482, 0.0004859177007222458965, 0.0009718354014444972140 ),
 .UNSPECIFIED. ) ;
#3644 = ORIENTED_EDGE ( 'NONE', *, *, #15097, .T. ) ;
#3645 = EDGE_CURVE ( 'NONE', #27689, #17580, #3363, .T. ) ;
#3646 = ADVANCED_FACE ( 'NONE', ( #2164 ), #6770, .F. ) ;
#3647 = VECTOR ( 'NONE', #5153, 1000.000000000000114 ) ;
#3648 = CARTESIAN_POINT ( 'NONE',  ( 2.433796855181219243, -74.00833731765649759, 125.2830755159751703 ) ) ;
#3649 = B_SPLINE_CURVE_WITH_KNOTS ( 'NONE', 3,
 ( #13742, #22549, #15330, #2817, #11592, #20370, #19794, #18201 ),
 .UNSPECIFIED., .F., .F.,
 ( 4, 2, 2, 4 ),
 ( 6.938893903907228378E-18, 0.0002429588503611282337, 0.0004859177007222495286, 0.0009718354014444800836 ),
 .UNSPECIFIED. ) ;
#3650 = CARTESIAN_POINT ( 'NONE',  ( -55.24198130335446422, 0.004163123460806185221, -0.008310594958150844397 ) ) ;
#3651 = CARTESIAN_POINT ( 'NONE',  ( -20.20700224038492365, 8.199606986804329978, -28.44216453106539078 ) ) ;
#3652 = DIRECTION ( 'NONE',  ( 1.000000000000000000, -6.938893903907226837E-18, 1.734723475976806709E-18 ) ) ;
#3653 = DIRECTION ( 'NONE',  ( 0.000000000000000000, 0.000000000000000000, -1.000000000000000000 ) ) ;
#3654 = EDGE_CURVE ( 'NONE', #13961, #14330, #15210, .T. ) ;
#3655 = CARTESIAN_POINT ( 'NONE',  ( 2.430230287190589422, -31.67257033707400637, -142.0258656395025412 ) ) ;
#3656 = CARTESIAN_POINT ( 'NONE',  ( 1.893872463202053824, 58.16604752596723671, 132.9857054814982291 ) ) ;
#3657 = DIRECTION ( 'NONE',  ( 0.5914120900931444380, -0.7643865440136106137, -0.2567974902965117767 ) ) ;
#3658 = VERTEX_POINT ( 'NONE', #15853 ) ;
#3659 = B_SPLINE_CURVE_WITH_KNOTS ( 'NONE', 3,
 ( #26781, #11965, #20740, #13543, #1033, #17851, #22343, #2606, #2909, #9237 ),
 .UNSPECIFIED., .F., .F.,
 ( 4, 2, 2, 2, 4 ),
 ( 8.299636676276019848E-18, 0.0003346267210630991806, 0.0006692534421261901213, 0.001003880163189280845, 0.001338506884252371786 ),
 .UNSPECIFIED. ) ;
#3660 = ORIENTED_EDGE ( 'NONE', *, *, #21996, .F. ) ;
#3661 = CARTESIAN_POINT ( 'NONE',  ( 25.64692872815573210, -107.2850779876532101, -35.19724814978025051 ) ) ;
#3663 = DIRECTION ( 'NONE',  ( -1.000000000000000000, 6.938893903907226837E-18, 5.541455922705464902E-20 ) ) ;
#3662 = CARTESIAN_POINT ( 'NONE',  ( 2.108393763691184919, 144.6252321290184284, -13.91282116576829608 ) ) ;
#3664 = DIRECTION ( 'NONE',  ( 0.000000000000000000, 0.000000000000000000, 1.000000000000000000 ) ) ;
#3665 = DIRECTION ( 'NONE',  ( -1.000000000000000000, -0.000000000000000000, -0.000000000000000000 ) ) ;
#3666 = CARTESIAN_POINT ( 'NONE',  ( 1.833206310202337042, 96.54250248081145003, -108.3342540861869168 ) ) ;
#3667 = EDGE_CURVE ( 'NONE', #13496, #18216, #1178, .T. ) ;
#3668 = VERTEX_POINT ( 'NONE', #26780 ) ;
#3669 = DIRECTION ( 'NONE',  ( -1.000000000000000000, -0.000000000000000000, -0.000000000000000000 ) ) ;
#3670 = CARTESIAN_POINT ( 'NONE',  ( 26.04756280548353686, -36.02883009343563714, -107.2904246402798663 ) ) ;
#3671 = CARTESIAN_POINT ( 'NONE',  ( 25.64681081121879203, -66.03065707438874199, -91.59071981940638807 ) ) ;
#3672 = ORIENTED_EDGE ( 'NONE', *, *, #27552, .F. ) ;
#3673 = VERTEX_POINT ( 'NONE', #7094 ) ;
#3674 = EDGE_CURVE ( 'NONE', #10482, #16310, #4916, .T. ) ;
#3675 = B_SPLINE_CURVE_WITH_KNOTS ( 'NONE', 3,
 ( #4404, #13047, #2094, #15605, #10897, #8884, #19658, #4837 ),
 .UNSPECIFIED., .F., .F.,
 ( 4, 2, 2, 4 ),
 ( 2.194186273941487449E-16, 0.002761568181852863766, 0.005523136363705508090, 0.01104627272741078893 ),
 .UNSPECIFIED. ) ;
#3676 = B_SPLINE_CURVE_WITH_KNOTS ( 'NONE', 3,
 ( #1057, #3357, #22665, #12144, #18614, #1199, #9845, #27384 ),
 .UNSPECIFIED., .F., .F.,
 ( 4, 2, 2, 4 ),
 ( 3.469446951953614189E-18, 0.0002429592666046704447, 0.0004859185332093374199, 0.0009718370664186920787 ),
 .UNSPECIFIED. ) ;
#3677 = CARTESIAN_POINT ( 'NONE',  ( -1.619063947482197729, 38.92136151114943488, 25.20140673341330739 ) ) ;
#3678 = ADVANCED_FACE ( 'NONE', ( #11527 ), #6941, .F. ) ;
#3679 = ORIENTED_EDGE ( 'NONE', *, *, #12290, .T. ) ;
#3680 = VERTEX_POINT ( 'NONE', #18144 ) ;
#3681 = CARTESIAN_POINT ( 'NONE',  ( 26.11404676487257603, -1.130420376097928115, 113.2169081140373947 ) ) ;
#3682 = ORIENTED_EDGE ( 'NONE', *, *, #24001, .F. ) ;
#3683 = CARTESIAN_POINT ( 'NONE',  ( 109.1586900883932856, 0.007109207791180751322, 0.0006456433529069300226 ) ) ;
#3684 = CARTESIAN_POINT ( 'NONE',  ( 26.11404676487257603, 112.7148551500680469, 10.71016160607605627 ) ) ;
#3685 = VECTOR ( 'NONE', #23861, 1000.000000000000114 ) ;
#3686 = CONTEXT_DEPENDENT_SHAPE_REPRESENTATION ( #22810, #11079 ) ;
#3687 = B_SPLINE_CURVE_WITH_KNOTS ( 'NONE', 3,
 ( #1627, #27962, #8259, #6375, #4061, #12834, #1900, #10700, #17297, #602, #15551, #20167, #24223 ),
 .UNSPECIFIED., .F., .F.,
 ( 4, 3, 3, 3, 4 ),
 ( 1.084202172485504434E-17, 0.0007657099931970561164, 0.001531419946797918721, 0.002296279302920154267, 0.003061450627205758099 ),
 .UNSPECIFIED. ) ;
#3688 = CARTESIAN_POINT ( 'NONE',  ( -28.41354790283022069, -14.62505768302787779, 18.00456980371915705 ) ) ;
#3689 = CARTESIAN_POINT ( 'NONE',  ( 2.263178113027048521, -60.41552743271048342, 132.2496129425957747 ) ) ;
#3690 = CARTESIAN_POINT ( 'NONE',  ( -55.25297051322618813, 0.007247191603132027878, 0.01306918787467585205 ) ) ;
#3691 = CARTESIAN_POINT ( 'NONE',  ( 25.98107933586724982, -47.01057192495340331, 102.9042679418247417 ) ) ;
#3692 = CARTESIAN_POINT ( 'NONE',  ( -1.045287976400365970, 15.59869763335068171, -43.05558670614252037 ) ) ;
#3693 =( BOUNDED_SURFACE ( )  B_SPLINE_SURFACE ( 3, 1, ( 
 ( #12042, #22713 ),
 ( #2981, #5854 ),
 ( #27429, #23415 ),
 ( #25575, #27860 ) ),
 .UNSPECIFIED., .F., .F., .F. ) 
 B_SPLINE_SURFACE_WITH_KNOTS ( ( 4, 4 ),
 ( 2, 2 ),
 ( 0.000000000000000000, 1.000000000000000000 ),
 ( 0.000000000000000000, 1.000000000000000000 ),
 .UNSPECIFIED. ) 
 GEOMETRIC_REPRESENTATION_ITEM ( )  RATIONAL_B_SPLINE_SURFACE ( (
 ( 1.000000000000000000, 1.000000000000000000),
 ( 0.9956975270656955868, 0.8568959468854907557),
 ( 0.9956975270656955868, 0.8568959468854907557),
 ( 1.000000000000000000, 1.000000000000000000) ) ) 
 REPRESENTATION_ITEM ( '' )  SURFACE ( )  );
#3694 = CARTESIAN_POINT ( 'NONE',  ( 28.37599760073042887, -105.5302221302109729, 45.02094138570548409 ) ) ;
#3696 = CARTESIAN_POINT ( 'NONE',  ( -1.619063947482197729, -46.30105812165550105, -2.489035965909997206 ) ) ;
#3695 = CARTESIAN_POINT ( 'NONE',  ( 25.64703792032470631, -97.85829113439916682, -56.32669596053541028 ) ) ;
#3697 = CARTESIAN_POINT ( 'NONE',  ( -20.20612092514784308, -1.137292630518264680, -29.57813644637189299 ) ) ;
#3698 = ORIENTED_EDGE ( 'NONE', *, *, #21079, .T. ) ;
#3699 = ORIENTED_EDGE ( 'NONE', *, *, #25952, .F. ) ;
#3700 = CARTESIAN_POINT ( 'NONE',  ( 8.186469777910943435, -49.43817851233971084, -140.9315935720375421 ) ) ;
#3701 = CARTESIAN_POINT ( 'NONE',  ( -23.79248802219730052, -30.42578156345377849, 13.25839849636389367 ) ) ;
#3702 = CARTESIAN_POINT ( 'NONE',  ( 109.1586900883932856, -0.007109207791180745251, -0.0006456433529069797875 ) ) ;
#3703 = CARTESIAN_POINT ( 'NONE',  ( 16.75465622695653423, 53.58152542127676554, 131.7467602971410656 ) ) ;
#3704 = DIRECTION ( 'NONE',  ( 0.000000000000000000, 5.223019709707975211E-21, -1.000000000000000000 ) ) ;
#3705 = EDGE_LOOP ( 'NONE', ( #13581, #9028, #12256, #23948 ) ) ;
#3706 = CARTESIAN_POINT ( 'NONE',  ( -1.259920593601969729, 12.06711544331625596, 44.39818421957802741 ) ) ;
#3707 = CARTESIAN_POINT ( 'NONE',  ( -20.20997486282892552, 3.551351076220724598E-15, -29.60348406988233450 ) ) ;
#3708 = ADVANCED_FACE ( 'NONE', ( #22786 ), #9369, .T. ) ;
#3709 = VERTEX_POINT ( 'NONE', #13829 ) ;
#3710 = CARTESIAN_POINT ( 'NONE',  ( 2.433796855181233454, -1.451562450948615135, -145.5024947199069913 ) ) ;
#3711 = FACE_OUTER_BOUND ( 'NONE', #5895, .T. ) ;
#3712 = CARTESIAN_POINT ( 'NONE',  ( 25.64670758986457599, -66.76959937251515953, 91.05338785329418272 ) ) ;
#3713 = CARTESIAN_POINT ( 'NONE',  ( 6.224689322667647851, 97.14981701196477104, -111.7293398381254974 ) ) ;
#3714 = EDGE_CURVE ( 'NONE', #16059, #2788, #4752, .T. ) ;
#3715 = AXIS2_PLACEMENT_3D ( 'NONE', #25509, #5783, #23633 ) ;
#3716 = CARTESIAN_POINT ( 'NONE',  ( 109.1592201516379674, 0.006957642258155071965, 0.003661068210032695190 ) ) ;
#3717 = CARTESIAN_POINT ( 'NONE',  ( 32.73300124599735739, 75.82012867748483131, 89.94078864464094636 ) ) ;
#3718 = AXIS2_PLACEMENT_3D ( 'NONE', #18897, #27669, #3625 ) ;
#3720 = EDGE_CURVE ( 'NONE', #15305, #17251, #17268, .T. ) ;
#3719 = ORIENTED_EDGE ( 'NONE', *, *, #24230, .T. ) ;
#3721 = B_SPLINE_CURVE_WITH_KNOTS ( 'NONE', 3,
 ( #2420, #7198, #13651, #27020, #22305, #11215, #17816 ),
 .UNSPECIFIED., .F., .F.,
 ( 4, 3, 4 ),
 ( 3.469446951953614189E-18, 0.009512539173626420944, 0.02506242213020843865 ),
 .UNSPECIFIED. ) ;
#3722 = CARTESIAN_POINT ( 'NONE',  ( 109.1721716018069515, -0.01665253177025269662, -0.003746085893651981968 ) ) ;
#3723 = AXIS2_PLACEMENT_3D ( 'NONE', #27035, #24914, #13952 ) ;
#3724 = CARTESIAN_POINT ( 'NONE',  ( 1.833485406944057594, -137.8414413349088932, 45.34878176254188276 ) ) ;
#3725 = ORIENTED_EDGE ( 'NONE', *, *, #21466, .T. ) ;
#3726 = LINE ( 'NONE', #19262, #23927 ) ;
#3727 = ORIENTED_EDGE ( 'NONE', *, *, #13944, .F. ) ;
#3728 = CIRCLE ( 'NONE', #9706, 34.60786435723138510 ) ;
#3729 = EDGE_LOOP ( 'NONE', ( #6444, #19866, #25623, #2355 ) ) ;
#3730 = CARTESIAN_POINT ( 'NONE',  ( 2.263178607246678187, -71.48082837426089498, 126.6115608827435892 ) ) ;
#3731 = CARTESIAN_POINT ( 'NONE',  ( -15.02187109954798316, -40.82269973458204504, 21.95370994985608704 ) ) ;
#3732 = CONICAL_SURFACE ( 'NONE', #4180, 117.6351876552689504, 0.9945805576725580410 ) ;
#3733 = FACE_OUTER_BOUND ( 'NONE', #19088, .T. ) ;
#3734 = CARTESIAN_POINT ( 'NONE',  ( -24.53237795827028123, -14.09663893005605395, -30.86653739599992363 ) ) ;
#3735 = CARTESIAN_POINT ( 'NONE',  ( 28.37644542392843405, 123.1691345231582773, 17.02293047611404475 ) ) ;
#3736 = PRESENTATION_LAYER_ASSIGNMENT (  '', '', ( #12904 ) ) ;
#3737 = CARTESIAN_POINT ( 'NONE',  ( -8.259864102781673267, 38.68084189741949785, -36.24929574824924572 ) ) ;
#3738 = CARTESIAN_POINT ( 'NONE',  ( 32.73300124599735739, -55.46353551262085091, 103.7392577722174565 ) ) ;
#3739 = CARTESIAN_POINT ( 'NONE',  ( 10.93730112725985926, -150.7858122213662853, 10.89264110824944609 ) ) ;
#3740 = ORIENTED_EDGE ( 'NONE', *, *, #25673, .T. ) ;
#3741 =( BOUNDED_SURFACE ( )  B_SPLINE_SURFACE ( 3, 1, ( 
 ( #2090, #19653 ),
 ( #3980, #26280 ),
 ( #6577, #15328 ),
 ( #12476, #10475 ) ),
 .UNSPECIFIED., .F., .F., .F. ) 
 B_SPLINE_SURFACE_WITH_KNOTS ( ( 4, 4 ),
 ( 2, 2 ),
 ( 0.000000000000000000, 1.000000000000000000 ),
 ( 0.000000000000000000, 1.000000000000000000 ),
 .UNSPECIFIED. ) 
 GEOMETRIC_REPRESENTATION_ITEM ( )  RATIONAL_B_SPLINE_SURFACE ( (
 ( 1.000000000000000000, 1.000000000000000000),
 ( 0.9956975270656954757, 0.8568959468854893125),
 ( 0.9956975270656954757, 0.8568959468854893125),
 ( 1.000000000000000000, 1.000000000000000000) ) ) 
 REPRESENTATION_ITEM ( '' )  SURFACE ( )  );
#3742 = EDGE_CURVE ( 'NONE', #22569, #3673, #20595, .T. ) ;
#3743 = ORIENTED_EDGE ( 'NONE', *, *, #1731, .F. ) ;
#3744 = CARTESIAN_POINT ( 'NONE',  ( -1.464342487929857661, -43.13914623307948659, 16.57334911911557285 ) ) ;
#3745 = CARTESIAN_POINT ( 'NONE',  ( -28.13707043255157103, 22.88591869784691113, -0.7675454997507807908 ) ) ;
#3746 = CARTESIAN_POINT ( 'NONE',  ( 109.1586059443104944, -0.006260042619939258299, 0.003294606663363219227 ) ) ;
#3747 = CARTESIAN_POINT ( 'NONE',  ( -1.050230346682689664, 14.15203301556493010, 43.55772679531834513 ) ) ;
#3748 = CARTESIAN_POINT ( 'NONE',  ( -1.058197053496172213, 42.99116279335175506, 15.81317659443640444 ) ) ;
#3749 = LINE ( 'NONE', #8629, #24071 ) ;
#3750 = CARTESIAN_POINT ( 'NONE',  ( -1.045287976400383290, 28.14015102489806708, -36.12803364096618708 ) ) ;
#3751 = ORIENTED_EDGE ( 'NONE', *, *, #10476, .F. ) ;
#3752 = CARTESIAN_POINT ( 'NONE',  ( 13.84597867724973597, 112.1633818588838949, -94.55652763153713636 ) ) ;
#3753 = FACE_OUTER_BOUND ( 'NONE', #7965, .T. ) ;
#3754 = CARTESIAN_POINT ( 'NONE',  ( -1.045287976400386842, 37.92705037016744285, -25.66401692420027203 ) ) ;
#3755 = EDGE_CURVE ( 'NONE', #2053, #5932, #17622, .T. ) ;
#3756 = B_SPLINE_CURVE_WITH_KNOTS ( 'NONE', 3,
 ( #19588, #10826, #28356, #26205, #4333, #21897, #20444, #18266, #24924, #726, #11953, #16556, #7510 ),
 .UNSPECIFIED., .F., .F.,
 ( 4, 3, 3, 3, 4 ),
 ( 8.673617379884035472E-18, 0.0007657099931970579596, 0.001531419946797923492, 0.002296279302920159471, 0.003061450627205763737 ),
 .UNSPECIFIED. ) ;
#3757 = FACE_OUTER_BOUND ( 'NONE', #7184, .T. ) ;
#3758 = CARTESIAN_POINT ( 'NONE',  ( 26.11404676487257603, 65.63269960453241936, 92.25884714080432047 ) ) ;
#3759 = EDGE_CURVE ( 'NONE', #9428, #27430, #3552, .T. ) ;
#3760 = ORIENTED_EDGE ( 'NONE', *, *, #22807, .T. ) ;
#3761 = CARTESIAN_POINT ( 'NONE',  ( 25.64704443564078318, -112.2786464378872751, -11.93517308299253443 ) ) ;
#3762 = AXIS2_PLACEMENT_3D ( 'NONE', #20538, #9606, #18090 ) ;
#3763 = CARTESIAN_POINT ( 'NONE',  ( -1.048994561756802391, 0.7655149579823430361, -45.79144455904140187 ) ) ;
#3764 = ORIENTED_EDGE ( 'NONE', *, *, #1155, .F. ) ;
#3765 = CONICAL_SURFACE ( 'NONE', #25371, 117.6351876552689504, 0.9945805576725580410 ) ;
#3766 = ORIENTED_EDGE ( 'NONE', *, *, #6319, .T. ) ;
#3767 = ORIENTED_EDGE ( 'NONE', *, *, #3882, .T. ) ;
#3768 = CARTESIAN_POINT ( 'NONE',  ( -1.619063947482197729, -29.22875152547730337, 35.99532424477411041 ) ) ;
#3769 = FACE_OUTER_BOUND ( 'NONE', #14476, .T. ) ;
#3770 = CARTESIAN_POINT ( 'NONE',  ( 1.833838850855462610, 30.25705358195048689, -141.9202662332485261 ) ) ;
#3771 = CARTESIAN_POINT ( 'NONE',  ( 109.1624594426973260, -0.01531968460305926580, 0.004489871836309038827 ) ) ;
#3772 = ORIENTED_EDGE ( 'NONE', *, *, #6145, .F. ) ;
#3773 = EDGE_CURVE ( 'NONE', #10268, #9673, #7715, .T. ) ;
#3774 = CARTESIAN_POINT ( 'NONE',  ( -20.57838717382308147, 10.78122205917039977, 27.96569011373074076 ) ) ;
#3775 = CARTESIAN_POINT ( 'NONE',  ( -6.574463467970654840, 5.014313797967739461, 51.07975593197901532 ) ) ;
#3776 = ADVANCED_FACE ( 'NONE', ( #11964 ), #6994, .F. ) ;
#3777 = VECTOR ( 'NONE', #25871, 1000.000000000000000 ) ;
#3778 = CARTESIAN_POINT ( 'NONE',  ( -20.57838717382308502, 23.26537097894105699, -18.89542499756508320 ) ) ;
#3779 = CARTESIAN_POINT ( 'NONE',  ( -22.34422965417122597, 16.46028608106157876, 34.15536449444073241 ) ) ;
#3780 = CARTESIAN_POINT ( 'NONE',  ( 25.81918753295378721, -110.3582118788978903, 24.41190151229222138 ) ) ;
#3781 = CARTESIAN_POINT ( 'NONE',  ( 13.36082413113063083, 53.25066407421806502, 143.3553710183991541 ) ) ;
#3782 = VECTOR ( 'NONE', #5373, 1000.000000000000000 ) ;
#3783 = EDGE_CURVE ( 'NONE', #1503, #22323, #23166, .T. ) ;
#3784 = CARTESIAN_POINT ( 'NONE',  ( -9.156249394959706578, 53.74753343182702991, -9.022661520477960551 ) ) ;
#3785 = CARTESIAN_POINT ( 'NONE',  ( -1.619063947482201282, -44.80407745103776307, 11.94059994246206635 ) ) ;
#3786 = CARTESIAN_POINT ( 'NONE',  ( -55.24271866751342941, 0.008433070970614256479, -0.004365563123935527895 ) ) ;
#3787 = CARTESIAN_POINT ( 'NONE',  ( 28.37644542392844116, 124.0168596762487567, -8.957364412598916914 ) ) ;
#3788 = CARTESIAN_POINT ( 'NONE',  ( 21.16825799904902539, -133.3214686481436217, -23.82367662027958133 ) ) ;
#3789 =( BOUNDED_SURFACE ( )  B_SPLINE_SURFACE ( 3, 1, ( 
 ( #23437, #21401 ),
 ( #18819, #3425 ),
 ( #12752, #6168 ),
 ( #7911, #14498 ) ),
 .UNSPECIFIED., .F., .F., .F. ) 
 B_SPLINE_SURFACE_WITH_KNOTS ( ( 4, 4 ),
 ( 2, 2 ),
 ( 0.000000000000000000, 1.000000000000000000 ),
 ( 0.000000000000000000, 1.000000000000000000 ),
 .UNSPECIFIED. ) 
 GEOMETRIC_REPRESENTATION_ITEM ( )  RATIONAL_B_SPLINE_SURFACE ( (
 ( 1.000000000000000000, 1.000000000000000000),
 ( 0.9934239774497838349, 0.8357310067453913582),
 ( 0.9934239774497838349, 0.8357310067453913582),
 ( 1.000000000000000000, 1.000000000000000000) ) ) 
 REPRESENTATION_ITEM ( '' )  SURFACE ( )  );
#3790 = ORIENTED_EDGE ( 'NONE', *, *, #10132, .F. ) ;
#3791 = ORIENTED_EDGE ( 'NONE', *, *, #13652, .F. ) ;
#3792 = CARTESIAN_POINT ( 'NONE',  ( 1.833206310202338152, -108.3342540861872294, -96.54250248081103791 ) ) ;
#3793 = CARTESIAN_POINT ( 'NONE',  ( 28.43349137099834323, 34.52178142065691446, -119.3601175884732015 ) ) ;
#3794 = ORIENTED_EDGE ( 'NONE', *, *, #28165, .F. ) ;
#3795 = ORIENTED_EDGE ( 'NONE', *, *, #17061, .F. ) ;
#3796 = ORIENTED_EDGE ( 'NONE', *, *, #27894, .F. ) ;
#3797 = CIRCLE ( 'NONE', #25851, 151.1787379149930359 ) ;
#3798 = CIRCLE ( 'NONE', #110, 12.50000000000000178 ) ;
#3799 = CARTESIAN_POINT ( 'NONE',  ( 1.833721034905649194, -141.8643653601972119, 30.51809396650970996 ) ) ;
#3800 = LINE ( 'NONE', #27972, #18050 ) ;
#3801 = DIRECTION ( 'NONE',  ( -0.5914120900931443270, -0.7023121577978098662, -0.3962188444547314337 ) ) ;
#3802 = CARTESIAN_POINT ( 'NONE',  ( 26.11404676487257603, 55.62948129436244926, 98.61392875273382685 ) ) ;
#3803 = EDGE_CURVE ( 'NONE', #6049, #24611, #9393, .T. ) ;
#3804 = CARTESIAN_POINT ( 'NONE',  ( 6.224689322667630975, -139.9988794244329142, -48.18553814190173057 ) ) ;
#3805 = CARTESIAN_POINT ( 'NONE',  ( 26.04756280548355463, -112.6689254848258344, -10.72497307632908736 ) ) ;
#3807 = ORIENTED_EDGE ( 'NONE', *, *, #16762, .T. ) ;
#3806 = EDGE_CURVE ( 'NONE', #8074, #21771, #16258, .T. ) ;
#3808 = ORIENTED_EDGE ( 'NONE', *, *, #1369, .T. ) ;
#3809 = CARTESIAN_POINT ( 'NONE',  ( -1.048994561756789734, -27.53485040342867407, 36.59609844253159139 ) ) ;
#3811 = CARTESIAN_POINT ( 'NONE',  ( -55.24198130335446422, 0.004276389980780370345, -0.008252882783649044540 ) ) ;
#3810 = CARTESIAN_POINT ( 'NONE',  ( -1.155031165708883423, 28.62780465193363355, 35.88345263711016031 ) ) ;
#3812 = EDGE_CURVE ( 'NONE', #531, #9093, #19158, .T. ) ;
#3813 = CARTESIAN_POINT ( 'NONE',  ( 25.64692872815574631, -103.0182448446671089, -46.21877827526664362 ) ) ;
#3814 = DIRECTION ( 'NONE',  ( 0.5946245182733607137, 0.08697490616139455510, -0.7992853357633870059 ) ) ;
#3815 = CARTESIAN_POINT ( 'NONE',  ( 1.833206308920057426, -71.90885838897311544, -126.0392061186629888 ) ) ;
#3816 = VECTOR ( 'NONE', #8691, 1000.000000000000000 ) ;
#3817 = ORIENTED_EDGE ( 'NONE', *, *, #15974, .F. ) ;
#3818 = CARTESIAN_POINT ( 'NONE',  ( 25.64681081121879203, 91.10197563708035773, -66.70335573067774249 ) ) ;
#3820 =( BOUNDED_SURFACE ( )  B_SPLINE_SURFACE ( 3, 1, ( 
 ( #18339, #27557 ),
 ( #14030, #14313 ),
 ( #11743, #5402 ),
 ( #3520, #9878 ) ),
 .UNSPECIFIED., .F., .F., .F. ) 
 B_SPLINE_SURFACE_WITH_KNOTS ( ( 4, 4 ),
 ( 2, 2 ),
 ( 0.000000000000000000, 1.000000000000000000 ),
 ( 0.000000000000000000, 1.000000000000000000 ),
 .UNSPECIFIED. ) 
 GEOMETRIC_REPRESENTATION_ITEM ( )  RATIONAL_B_SPLINE_SURFACE ( (
 ( 1.000000000000000000, 1.000000000000000000),
 ( 0.9956975270656954757, 0.8568959468854893125),
 ( 0.9956975270656954757, 0.8568959468854893125),
 ( 1.000000000000000000, 1.000000000000000000) ) ) 
 REPRESENTATION_ITEM ( '' )  SURFACE ( )  );
#3819 = CIRCLE ( 'NONE', #24058, 34.60786435723138510 ) ;
#3821 = CARTESIAN_POINT ( 'NONE',  ( -7.711401346138400115, -25.75361633141456608, 45.70592430511747040 ) ) ;
#3822 = CARTESIAN_POINT ( 'NONE',  ( -55.24340739397742794, 0.0007387096945709508214, 0.01010924026184075245 ) ) ;
#3823 = ORIENTED_EDGE ( 'NONE', *, *, #25489, .F. ) ;
#3824 = ORIENTED_EDGE ( 'NONE', *, *, #18702, .F. ) ;
#3825 = B_SPLINE_CURVE_WITH_KNOTS ( 'NONE', 3,
 ( #25706, #19492, #23552, #5987, #14888, #10171, #23702, #16789 ),
 .UNSPECIFIED., .F., .F.,
 ( 4, 2, 2, 4 ),
 ( 1.387778780781445676E-17, 0.0002429588503611381271, 0.0004859177007222623764, 0.0009718354014445054539 ),
 .UNSPECIFIED. ) ;
#3826 = CARTESIAN_POINT ( 'NONE',  ( -8.259864102781671491, -52.06232470801718648, -9.986657004933428894 ) ) ;
#3827 = ORIENTED_EDGE ( 'NONE', *, *, #3510, .T. ) ;
#3828 = ORIENTED_EDGE ( 'NONE', *, *, #5615, .T. ) ;
#3829 = CARTESIAN_POINT ( 'NONE',  ( 2.108393763691200462, -13.91282116576881300, -144.6252321290183147 ) ) ;
#3830 = ORIENTED_EDGE ( 'NONE', *, *, #8140, .F. ) ;
#3831 = CARTESIAN_POINT ( 'NONE',  ( 25.86096068574580897, -45.07009591924492753, -103.6815822123523390 ) ) ;
#3832 = CARTESIAN_POINT ( 'NONE',  ( 1.831572820252009626, 29.20415387690763609, -142.1425225354577435 ) ) ;
#3833 = ITEM_DEFINED_TRANSFORMATION ( 'NONE', 'NONE', #17625,  #27263 ) ;
#3834 = CARTESIAN_POINT ( 'NONE',  ( 2.263178607246671081, -73.90841395012498083, -125.2099936970375609 ) ) ;
#3835 = AXIS2_PLACEMENT_3D ( 'NONE', #8901, #26575, #2392 ) ;
#3836 = CARTESIAN_POINT ( 'NONE',  ( 28.37644542392838432, -76.32685750075070530, 98.15613422114063269 ) ) ;
#3837 = AXIS2_PLACEMENT_3D ( 'NONE', #3856, #12484, #8186 ) ;
#3838 = CARTESIAN_POINT ( 'NONE',  ( 8.186469777911000278, 134.9918587298873547, -63.89871389959332504 ) ) ;
#3839 = CARTESIAN_POINT ( 'NONE',  ( 6.224689322667647851, -118.2566963816776848, 89.08920297664174370 ) ) ;
#3840 = CARTESIAN_POINT ( 'NONE',  ( 25.98107933586711127, 55.61918067932742815, 98.51796269673089057 ) ) ;
#3841 = CARTESIAN_POINT ( 'NONE',  ( 32.73300124599735028, 72.21147546950551543, 92.86301839380053025 ) ) ;
#3842 = EDGE_CURVE ( 'NONE', #12210, #19484, #3900, .T. ) ;
#3843 = CARTESIAN_POINT ( 'NONE',  ( -20.20612091757424622, 8.058516044219587116, 28.48192249925577357 ) ) ;
#3845 = CARTESIAN_POINT ( 'NONE',  ( 25.69398547355839213, -11.06723946918835644, 112.3990349503584838 ) ) ;
#3844 = CARTESIAN_POINT ( 'NONE',  ( 25.64700659047694842, -97.67001118499064205, -56.65258046470359687 ) ) ;
#3846 = CARTESIAN_POINT ( 'NONE',  ( -28.41354790283022069, -23.16239616762929998, 1.249099604787319295 ) ) ;
#3847 = VERTEX_POINT ( 'NONE', #1864 ) ;
#3848 = VERTEX_POINT ( 'NONE', #23915 ) ;
#3849 = CARTESIAN_POINT ( 'NONE',  ( 25.64692232868534560, 56.17236075412082386, -97.94691534265373889 ) ) ;
#3850 = DIRECTION ( 'NONE',  ( -0.5946245182733607137, -0.08697490616138379982, -0.7992853357633882272 ) ) ;
#3851 = CARTESIAN_POINT ( 'NONE',  ( 32.73300124599735028, 66.00340565729339914, 97.37344512919882789 ) ) ;
#3852 = DIRECTION ( 'NONE',  ( 0.000000000000000000, 5.223019709707975211E-21, -1.000000000000000000 ) ) ;
#3853 = DIRECTION ( 'NONE',  ( 0.5914120900931444380, -0.4674599267565346938, -0.6570486713847260019 ) ) ;
#3854 = ORIENTED_EDGE ( 'NONE', *, *, #8521, .F. ) ;
#3855 = CARTESIAN_POINT ( 'NONE',  ( -55.24271866751342941, 0.009369360294296125852, 0.001545935011630558513 ) ) ;
#3856 = CARTESIAN_POINT ( 'NONE',  ( -8.786685647604885574, 6.096987947571466530E-17, -1.524246986892866633E-17 ) ) ;
#3857 = ORIENTED_EDGE ( 'NONE', *, *, #935, .F. ) ;
#3858 = CARTESIAN_POINT ( 'NONE',  ( -55.24340739397742794, 0.006539691034608862037, 0.007744344507854531226 ) ) ;
#3859 = CARTESIAN_POINT ( 'NONE',  ( 1.832998868059890096, 142.0492247521722788, 29.64765804470122745 ) ) ;
#3860 = DIRECTION ( 'NONE',  ( -6.938893903907226837E-18, -1.000000000000000000, 0.000000000000000000 ) ) ;
#3861 = CARTESIAN_POINT ( 'NONE',  ( 25.64681081121879203, 107.5125461021402486, 34.49579773461821475 ) ) ;
#3862 = CARTESIAN_POINT ( 'NONE',  ( 109.1592201516379674, 0.003661068210032671338, -0.006957642258155084976 ) ) ;
#3863 = CARTESIAN_POINT ( 'NONE',  ( 1.833485406944043827, -45.34878176254329674, 137.8414413349084100 ) ) ;
#3864 = VERTEX_POINT ( 'NONE', #19020 ) ;
#3865 = CARTESIAN_POINT ( 'NONE',  ( 2.430230287190572103, 28.83279105684426113, 142.6294793592098813 ) ) ;
#3866 = AXIS2_PLACEMENT_3D ( 'NONE', #12189, #7455, #10189 ) ;
#3867 =( BOUNDED_SURFACE ( )  B_SPLINE_SURFACE ( 3, 1, ( 
 ( #25907, #19414 ),
 ( #8485, #17248 ),
 ( #21572, #17526 ),
 ( #26447, #24306 ) ),
 .UNSPECIFIED., .F., .F., .F. ) 
 B_SPLINE_SURFACE_WITH_KNOTS ( ( 4, 4 ),
 ( 2, 2 ),
 ( 0.000000000000000000, 1.000000000000000000 ),
 ( 0.000000000000000000, 1.000000000000000000 ),
 .UNSPECIFIED. ) 
 GEOMETRIC_REPRESENTATION_ITEM ( )  RATIONAL_B_SPLINE_SURFACE ( (
 ( 1.000000000000000000, 1.000000000000000000),
 ( 0.7789835883360578528, 0.9689951854195403280),
 ( 0.7789835883360578528, 0.9689951854195403280),
 ( 1.000000000000000000, 1.000000000000000000) ) ) 
 REPRESENTATION_ITEM ( '' )  SURFACE ( )  );
#3868 = CARTESIAN_POINT ( 'NONE',  ( 2.430230287190572103, -145.5073573687466819, -1.451610819319274270 ) ) ;
#3869 = VERTEX_POINT ( 'NONE', #27800 ) ;
#3870 = CARTESIAN_POINT ( 'NONE',  ( 10.93730112725990189, -97.44200844886194091, -115.5857507957714461 ) ) ;
#3871 = ORIENTED_EDGE ( 'NONE', *, *, #19884, .T. ) ;
#3872 = B_SPLINE_CURVE_WITH_KNOTS ( 'NONE', 3,
 ( #1179, #15893, #20060, #18039 ),
 .UNSPECIFIED., .F., .F.,
 ( 4, 4 ),
 ( 1.422050084071091177E-16, 0.008383748772659580309 ),
 .UNSPECIFIED. ) ;
#3873 = CARTESIAN_POINT ( 'NONE',  ( 2.433796855181233454, -1.451562450948615135, -145.5024947199069913 ) ) ;
#3874 = DIRECTION ( 'NONE',  ( -0.7563875759206388771, 0.3556158456312860094, -0.5490129373055293582 ) ) ;
#3875 =( BOUNDED_SURFACE ( )  B_SPLINE_SURFACE ( 3, 1, ( 
 ( #10943, #19708 ),
 ( #8782, #17547 ),
 ( #12224, #20864 ),
 ( #11799, #9498 ) ),
 .UNSPECIFIED., .F., .F., .F. ) 
 B_SPLINE_SURFACE_WITH_KNOTS ( ( 4, 4 ),
 ( 2, 2 ),
 ( 0.000000000000000000, 1.000000000000000000 ),
 ( 0.000000000000000000, 1.000000000000000000 ),
 .UNSPECIFIED. ) 
 GEOMETRIC_REPRESENTATION_ITEM ( )  RATIONAL_B_SPLINE_SURFACE ( (
 ( 1.000000000000000000, 1.000000000000000000),
 ( 0.9956975270656954757, 0.8568959468854893125),
 ( 0.9956975270656954757, 0.8568959468854893125),
 ( 1.000000000000000000, 1.000000000000000000) ) ) 
 REPRESENTATION_ITEM ( '' )  SURFACE ( )  );
#3876 = CARTESIAN_POINT ( 'NONE',  ( -1.048996300304502194, 37.49570739463922564, 26.29666317565261124 ) ) ;
#3877 = ADVANCED_FACE ( 'NONE', ( #16869, #8226 ), #4171, .F. ) ;
#3878 = CARTESIAN_POINT ( 'NONE',  ( -1.049817751779889008, -14.63752841325019105, 43.39729912094394848 ) ) ;
#3879 = EDGE_CURVE ( 'NONE', #20144, #9116, #22115, .T. ) ;
#3880 = CARTESIAN_POINT ( 'NONE',  ( 13.36082413113063083, -152.7944199136427983, 6.345145185217505812 ) ) ;
#3881 = CARTESIAN_POINT ( 'NONE',  ( 109.1589550718175161, -0.006826119083824107661, 0.003284595046935108106 ) ) ;
#3882 = EDGE_CURVE ( 'NONE', #14688, #17616, #10111, .T. ) ;
#3883 = CARTESIAN_POINT ( 'NONE',  ( -5.986830583229481917, 38.20088153919500229, -33.39046620690925238 ) ) ;
#3884 = CARTESIAN_POINT ( 'NONE',  ( -1.044557008772713402, -15.70482370518787718, 43.01636061109000053 ) ) ;
#3885 = CARTESIAN_POINT ( 'NONE',  ( 1.833206310202334599, -58.34025049825039844, 132.8652722326996809 ) ) ;
#3886 = VERTEX_POINT ( 'NONE', #10525 ) ;
#3887 = ORIENTED_EDGE ( 'NONE', *, *, #16584, .F. ) ;
#3888 = ORIENTED_EDGE ( 'NONE', *, *, #25609, .F. ) ;
#3889 = CARTESIAN_POINT ( 'NONE',  ( 28.37599760073042887, -112.5845136272806997, 22.09615888373918935 ) ) ;
#3890 = CARTESIAN_POINT ( 'NONE',  ( -25.21435515916043002, 31.17620025257588523, -15.02493970636157705 ) ) ;
#3891 = CARTESIAN_POINT ( 'NONE',  ( -1.050229599974486616, 13.90955673306187990, 43.63650726458048013 ) ) ;
#3892 = CARTESIAN_POINT ( 'NONE',  ( -1.259972190295298944, 43.01178231151332909, -16.33417789844387968 ) ) ;
#3893 = CARTESIAN_POINT ( 'NONE',  ( 1.832998868059890096, -142.0492247521720799, -29.64765804470219024 ) ) ;
#3894 = CARTESIAN_POINT ( 'NONE',  ( -20.20700224038492365, -8.199606986804534259, -28.44216453106533748 ) ) ;
#3895 = ORIENTED_EDGE ( 'NONE', *, *, #15644, .F. ) ;
#3896 = CARTESIAN_POINT ( 'NONE',  ( -10.86508079875782684, -9.118642906269649018, -50.32133009257454859 ) ) ;
#3897 = CARTESIAN_POINT ( 'NONE',  ( -1.031422197589711987, 28.14735071801795740, 36.13727897780095333 ) ) ;
#3898 = CARTESIAN_POINT ( 'NONE',  ( -1.049817751779873909, -36.75003908324312363, -27.33161971822185876 ) ) ;
#3899 = B_SPLINE_CURVE_WITH_KNOTS ( 'NONE', 3,
 ( #21992, #26310, #4014, #12785 ),
 .UNSPECIFIED., .F., .F.,
 ( 4, 4 ),
 ( 0.000000000000000000, 0.008383560773332720747 ),
 .UNSPECIFIED. ) ;
#3900 = LINE ( 'NONE', #10259, #25906 ) ;
#3901 = ORIENTED_EDGE ( 'NONE', *, *, #12736, .T. ) ;
#3902 = CARTESIAN_POINT ( 'NONE',  ( 25.64692232868535626, -45.62640214192334298, 103.2819624397966294 ) ) ;
#3903 = DIRECTION ( 'NONE',  ( -0.000000000000000000, 1.000000000000000000, -0.000000000000000000 ) ) ;
#3904 = ORIENTED_EDGE ( 'NONE', *, *, #1189, .T. ) ;
#3905 = ORIENTED_EDGE ( 'NONE', *, *, #21718, .F. ) ;
#3906 = ORIENTED_EDGE ( 'NONE', *, *, #10775, .T. ) ;
#3907 = EDGE_CURVE ( 'NONE', #15665, #14553, #8438, .T. ) ;
#3908 = CARTESIAN_POINT ( 'NONE',  ( -55.24390624410018802, 0.004896917417131886954, -0.009209468562452662738 ) ) ;
#3909 = ADVANCED_FACE ( 'NONE', ( #3757 ), #9943, .F. ) ;
#3910 = DIRECTION ( 'NONE',  ( 0.5914120900931444380, -0.8063295922669342364, -0.008020494142999035764 ) ) ;
#3911 =( BOUNDED_SURFACE ( )  B_SPLINE_SURFACE ( 3, 1, ( 
 ( #14944, #5914 ),
 ( #3589, #14670 ),
 ( #12368, #27483 ),
 ( #7795, #16552 ) ),
 .UNSPECIFIED., .F., .F., .F. ) 
 B_SPLINE_SURFACE_WITH_KNOTS ( ( 4, 4 ),
 ( 2, 2 ),
 ( 0.000000000000000000, 1.000000000000000000 ),
 ( 0.000000000000000000, 1.000000000000000000 ),
 .UNSPECIFIED. ) 
 GEOMETRIC_REPRESENTATION_ITEM ( )  RATIONAL_B_SPLINE_SURFACE ( (
 ( 1.000000000000000000, 1.000000000000000000),
 ( 0.7789835883360576307, 0.9689951854195403280),
 ( 0.7789835883360576307, 0.9689951854195403280),
 ( 1.000000000000000000, 1.000000000000000000) ) ) 
 REPRESENTATION_ITEM ( '' )  SURFACE ( )  );
#3912 = EDGE_CURVE ( 'NONE', #21594, #21998, #21022, .T. ) ;
#3913 = B_SPLINE_CURVE_WITH_KNOTS ( 'NONE', 3,
 ( #21704, #10779, #21849, #10495, #19264, #28033, #19672, #28443, #4001, #17100 ),
 .UNSPECIFIED., .F., .F.,
 ( 4, 2, 2, 2, 4 ),
 ( 2.947001115474787729E-16, 0.0003346187017559134843, 0.0006692374035115322825, 0.001003856105267151135, 0.001338474807022769879 ),
 .UNSPECIFIED. ) ;
#3914 = CARTESIAN_POINT ( 'NONE',  ( 1.833206308920065197, -132.8652726225756737, 58.34024961171186874 ) ) ;
#3915 = B_SPLINE_CURVE_WITH_KNOTS ( 'NONE', 3,
 ( #25240, #25678, #13994, #14270, #23091, #3351 ),
 .UNSPECIFIED., .F., .F.,
 ( 4, 2, 4 ),
 ( 4.341940435234061368E-16, 0.003576372551511239426, 0.007152745103022045171 ),
 .UNSPECIFIED. ) ;
#3916 = CARTESIAN_POINT ( 'NONE',  ( 26.28373643307405771, 82.21796085350790406, -97.52903534490786797 ) ) ;
#3917 = VERTEX_POINT ( 'NONE', #18873 ) ;
#3918 = CARTESIAN_POINT ( 'NONE',  ( -55.24340739397742084, -0.01010924026184288269, -0.0007387096945739216438 ) ) ;
#3919 = CARTESIAN_POINT ( 'NONE',  ( 109.1778270068192853, 0.007323887274071894798, 0.005755170886745451797 ) ) ;
#3920 = CARTESIAN_POINT ( 'NONE',  ( 28.37599760073042887, -25.60640155549242181, 111.8383885143454393 ) ) ;
#3921 = CARTESIAN_POINT ( 'NONE',  ( -1.050230347699842692, 5.964912479342754695E-15, -45.79907861674080749 ) ) ;
#3922 = CARTESIAN_POINT ( 'NONE',  ( -1.019300379054419947, 28.53917295602898463, -35.83762006677410028 ) ) ;
#3923 = B_SPLINE_CURVE_WITH_KNOTS ( 'NONE', 3,
 ( #25052, #23037, #9633, #20272, #9495, #3155, #5016, #564 ),
 .UNSPECIFIED., .F., .F.,
 ( 4, 2, 2, 4 ),
 ( 7.757919228897728493E-18, 0.0002429592666046773836, 0.0004859185332093470151, 0.0009718370664186765746 ),
 .UNSPECIFIED. ) ;
#3924 = CARTESIAN_POINT ( 'NONE',  ( 109.1624594426973260, -0.01595733256931099533, -0.0004639210235577357917 ) ) ;
#3925 = CARTESIAN_POINT ( 'NONE',  ( 30.58324630866342986, -95.47492154584209345, 74.24222250960207248 ) ) ;
#3926 = CARTESIAN_POINT ( 'NONE',  ( 13.84597867724971643, 140.9259526407714986, -40.76072889493610774 ) ) ;
#3927 = ORIENTED_EDGE ( 'NONE', *, *, #8523, .F. ) ;
#3928 = ORIENTED_EDGE ( 'NONE', *, *, #7453, .F. ) ;
#3929 = CARTESIAN_POINT ( 'NONE',  ( -1.044556982611269280, 37.98985389331847529, 25.56989963842161728 ) ) ;
#3930 = CARTESIAN_POINT ( 'NONE',  ( 2.433796855181233454, -57.85512797797981932, 133.5135467655516095 ) ) ;
#3931 = ORIENTED_EDGE ( 'NONE', *, *, #23934, .T. ) ;
#3932 = EDGE_LOOP ( 'NONE', ( #16801, #9094, #17016, #19192 ) ) ;
#3933 = VERTEX_POINT ( 'NONE', #8370 ) ;
#3934 = EDGE_CURVE ( 'NONE', #3864, #6911, #17131, .T. ) ;
#3935 = EDGE_CURVE ( 'NONE', #13364, #10267, #21398, .T. ) ;
#3936 = EDGE_CURVE ( 'NONE', #813, #11599, #5970, .T. ) ;
#3937 = CARTESIAN_POINT ( 'NONE',  ( 1.833838848569415925, -141.9017642089167168, 30.34409872482189030 ) ) ;
#3938 = B_SPLINE_CURVE_WITH_KNOTS ( 'NONE', 3,
 ( #27131, #24582, #16202, #25011, #5264, #26704, #14039, #3112, #11888, #20656 ),
 .UNSPECIFIED., .F., .F.,
 ( 4, 2, 2, 2, 4 ),
 ( 2.799429325053882983E-16, 0.0003346187017559012328, 0.0006692374035115225247, 0.001003856105267143762, 0.001338474807022765108 ),
 .UNSPECIFIED. ) ;
#3939 = EDGE_CURVE ( 'NONE', #24113, #4452, #19024, .T. ) ;
#3940 = CARTESIAN_POINT ( 'NONE',  ( -12.82751273423884442, 6.573887447703498310, 48.43568301531131937 ) ) ;
#3941 = CARTESIAN_POINT ( 'NONE',  ( -20.20700224038492721, 0.9908225410482660589, 29.58392382092671724 ) ) ;
#3942 = CARTESIAN_POINT ( 'NONE',  ( -25.21435515916042647, 25.00736669481023355, -23.92354251275945742 ) ) ;
#3943 =( BOUNDED_SURFACE ( )  B_SPLINE_SURFACE ( 3, 1, ( 
 ( #20316, #9400 ),
 ( #2471, #2758 ),
 ( #23191, #25336 ),
 ( #458, #5611 ) ),
 .UNSPECIFIED., .F., .F., .F. ) 
 B_SPLINE_SURFACE_WITH_KNOTS ( ( 4, 4 ),
 ( 2, 2 ),
 ( 0.000000000000000000, 1.000000000000000000 ),
 ( 0.000000000000000000, 1.000000000000000000 ),
 .UNSPECIFIED. ) 
 GEOMETRIC_REPRESENTATION_ITEM ( )  RATIONAL_B_SPLINE_SURFACE ( (
 ( 1.000000000000000000, 1.000000000000000000),
 ( 0.9593753223639863714, 0.9995975284513187731),
 ( 0.9593753223639863714, 0.9995975284513187731),
 ( 1.000000000000000000, 1.000000000000000000) ) ) 
 REPRESENTATION_ITEM ( '' )  SURFACE ( )  );
#3944 = CARTESIAN_POINT ( 'NONE',  ( 109.1721716018069657, 0.003350975118864183214, -0.01673651515803010678 ) ) ;
#3945 = CARTESIAN_POINT ( 'NONE',  ( 9.884929003653626367, -135.7578851563890510, 65.04493172071430251 ) ) ;
#3946 = CARTESIAN_POINT ( 'NONE',  ( 2.433796855181219243, -126.7346379669260443, 71.49415740225030902 ) ) ;
#3947 = ORIENTED_EDGE ( 'NONE', *, *, #12228, .F. ) ;
#3948 = ORIENTED_EDGE ( 'NONE', *, *, #4783, .F. ) ;
#3950 = CARTESIAN_POINT ( 'NONE',  ( -10.86508079875780730, -35.35100740321749413, 36.95527278096565027 ) ) ;
#3949 = CARTESIAN_POINT ( 'NONE',  ( 25.64708228042121263, 112.9112740241346984, 0.03938584558032432598 ) ) ;
#3951 = CARTESIAN_POINT ( 'NONE',  ( 10.93730112726003156, 97.44200844886434254, -115.5857507957695276 ) ) ;
#3952 = LINE ( 'NONE', #27712, #3308 ) ;
#3953 = FACE_OUTER_BOUND ( 'NONE', #10490, .T. ) ;
#3954 = ORIENTED_EDGE ( 'NONE', *, *, #13971, .F. ) ;
#3955 = DIRECTION ( 'NONE',  ( -1.000000000000000000, -0.000000000000000000, -0.000000000000000000 ) ) ;
#3956 = CARTESIAN_POINT ( 'NONE',  ( -1.045287976400379737, -37.92705037016725100, 25.66401692420055269 ) ) ;
#3957 = B_SPLINE_CURVE_WITH_KNOTS ( 'NONE', 3,
 ( #12208, #12070, #5882, #12480, #1259, #7767 ),
 .UNSPECIFIED., .F., .F.,
 ( 4, 2, 4 ),
 ( 0.000000000000000000, 0.0004335184443140232147, 0.0008670368886280464295 ),
 .UNSPECIFIED. ) ;
#3958 = CARTESIAN_POINT ( 'NONE',  ( -20.38016308990358638, 23.16952666206584155, -18.69911008768343663 ) ) ;
#3959 = EDGE_LOOP ( 'NONE', ( #16487, #12051, #5829, #21502 ) ) ;
#3960 = B_SPLINE_CURVE_WITH_KNOTS ( 'NONE', 3,
 ( #6195, #28450, #13335, #10918, #23895, #22134, #21987 ),
 .UNSPECIFIED., .F., .F.,
 ( 4, 3, 4 ),
 ( 0.000000000000000000, 0.02398743853561339720, 0.04000277880656220864 ),
 .UNSPECIFIED. ) ;
#3961 = ORIENTED_EDGE ( 'NONE', *, *, #13253, .T. ) ;
#3962 = CARTESIAN_POINT ( 'NONE',  ( -1.045287976400351981, -15.59869763335126436, -43.05558670614231431 ) ) ;
#3963 = ORIENTED_EDGE ( 'NONE', *, *, #27151, .T. ) ;
#3964 = ORIENTED_EDGE ( 'NONE', *, *, #22023, .T. ) ;
#3965 = ADVANCED_FACE ( 'NONE', ( #12947 ), #17586, .F. ) ;
#3966 = ORIENTED_EDGE ( 'NONE', *, *, #21382, .F. ) ;
#3967 = EDGE_CURVE ( 'NONE', #9705, #27648, #10458, .T. ) ;
#3968 = CARTESIAN_POINT ( 'NONE',  ( 2.108985857320913038, -73.75356715683001596, -125.1820688103229884 ) ) ;
#3969 = CARTESIAN_POINT ( 'NONE',  ( 25.64681081121879203, -0.4157506337719985012, -112.9102952884414606 ) ) ;
#3970 = DIRECTION ( 'NONE',  ( 0.000000000000000000, 0.000000000000000000, 1.000000000000000000 ) ) ;
#3971 = CARTESIAN_POINT ( 'NONE',  ( 2.108985857320924584, 138.5727354014057084, 43.67763756616700022 ) ) ;
#3972 = FACE_OUTER_BOUND ( 'NONE', #25658, .T. ) ;
#3973 = B_SPLINE_CURVE_WITH_KNOTS ( 'NONE', 3,
 ( #25845, #23555, #60, #8559, #19628, #14891 ),
 .UNSPECIFIED., .F., .F.,
 ( 4, 2, 4 ),
 ( 3.035766082959412415E-18, 0.0006311636237756726225, 0.001262327247551342860 ),
 .UNSPECIFIED. ) ;
#3974 = CARTESIAN_POINT ( 'NONE',  ( -1.239374126674604337, 11.92219841463829333, -44.48112152129351671 ) ) ;
#3975 = CARTESIAN_POINT ( 'NONE',  ( 1.833485406944043827, -117.7091014914955309, 84.86072343962528919 ) ) ;
#3976 = CARTESIAN_POINT ( 'NONE',  ( 1.833485406944057594, 30.69200235378934849, 141.8265699653868523 ) ) ;
#3977 = EDGE_LOOP ( 'NONE', ( #15739, #7297, #1489, #12788 ) ) ;
#3978 = VERTEX_POINT ( 'NONE', #24188 ) ;
#3979 = CARTESIAN_POINT ( 'NONE',  ( -20.20700224038492365, 10.08426345511628597, 27.82980252387807951 ) ) ;
#3980 = CARTESIAN_POINT ( 'NONE',  ( 109.1589550718174877, 0.001354998915261331188, 0.007453082872776644989 ) ) ;
#3982 = CARTESIAN_POINT ( 'NONE',  ( 25.64670758986457599, -98.03181353150523591, 56.02376616805386789 ) ) ;
#3981 = CARTESIAN_POINT ( 'NONE',  ( 6.224689322667630975, -28.26953958630515018, -145.3353551538644126 ) ) ;
#3983 = CARTESIAN_POINT ( 'NONE',  ( -8.786685647604890903, -48.22796981442753150, 23.24040270374441874 ) ) ;
#3984 = CARTESIAN_POINT ( 'NONE',  ( 14.74894986621300141, -1.023413983156985299E-16, 2.558534957892463246E-17 ) ) ;
#3985 = CARTESIAN_POINT ( 'NONE',  ( -55.24390624410018802, 0.009209468562452933355, 0.004896917417131438528 ) ) ;
#3986 = LINE ( 'NONE', #53, #7534 ) ;
#3987 = ORIENTED_EDGE ( 'NONE', *, *, #3537, .T. ) ;
#3988 = CARTESIAN_POINT ( 'NONE',  ( 25.64708228042122684, -112.2968511928419986, 11.76327187353777859 ) ) ;
#3989 = FACE_OUTER_BOUND ( 'NONE', #1437, .T. ) ;
#3990 = CARTESIAN_POINT ( 'NONE',  ( -55.24340739397742794, 0.002421372372456844640, -0.009842732675349010960 ) ) ;
#3991 = CARTESIAN_POINT ( 'NONE',  ( -1.583189561560256253, -46.33203782964459805, 2.490696082060350314 ) ) ;
#3992 = CARTESIAN_POINT ( 'NONE',  ( -20.37983603106074426, -1.508851015062371292, 29.73529213200292531 ) ) ;
#3993 = ORIENTED_EDGE ( 'NONE', *, *, #26831, .F. ) ;
#3994 = B_SPLINE_CURVE_WITH_KNOTS ( 'NONE', 3,
 ( #17774, #22544, #505, #24572, #26550, #9440, #6714, #18196 ),
 .UNSPECIFIED., .F., .F.,
 ( 4, 2, 2, 4 ),
 ( 5.421010862427522170E-20, 0.0002429588503611193433, 0.0004859177007222386323, 0.0009718354014444823604 ),
 .UNSPECIFIED. ) ;
#3995 = CARTESIAN_POINT ( 'NONE',  ( 13.84597867724971287, 64.00674338126026441, -132.0026437215594228 ) ) ;
#3996 = CARTESIAN_POINT ( 'NONE',  ( 109.1589550718174877, 0.003980125429499884598, -0.006445391216542585913 ) ) ;
#3997 = EDGE_CURVE ( 'NONE', #20945, #23678, #16618, .T. ) ;
#3998 = ORIENTED_EDGE ( 'NONE', *, *, #20899, .T. ) ;
#3999 = CARTESIAN_POINT ( 'NONE',  ( -1.044557008772707407, 37.98985164565329598, -25.56990300676994821 ) ) ;
#4000 = ADVANCED_FACE ( 'NONE', ( #28338 ), #18747, .F. ) ;
#4001 = CARTESIAN_POINT ( 'NONE',  ( -1.539763995773692828, -35.94321074656915016, -29.16712963492449973 ) ) ;
#4002 = EDGE_CURVE ( 'NONE', #28150, #654, #11078, .T. ) ;
#4003 = CARTESIAN_POINT ( 'NONE',  ( 2.108985857320888613, -116.7869613039525518, 86.43462668039097707 ) ) ;
#4004 = CARTESIAN_POINT ( 'NONE',  ( -8.786685647604887350, -25.35688121747534751, -47.14957014837345639 ) ) ;
#4005 = LINE ( 'NONE', #21710, #16607 ) ;
#4006 = LINE ( 'NONE', #8612, #18059 ) ;
#4007 = CARTESIAN_POINT ( 'NONE',  ( 10.93730112725990722, -136.0306644680979389, -65.95960219663263047 ) ) ;
#4008 = DIRECTION ( 'NONE',  ( -1.000000000000000000, 0.000000000000000000, -0.000000000000000000 ) ) ;
#4009 = CARTESIAN_POINT ( 'NONE',  ( 25.64708228042120908, 110.4357030047557799, 23.51409906510251346 ) ) ;
#4010 = B_SPLINE_CURVE_WITH_KNOTS ( 'NONE', 3,
 ( #12646, #2396, #4145, #15355, #13070, #24031 ),
 .UNSPECIFIED., .F., .F.,
 ( 4, 2, 4 ),
 ( 6.942281208919283290E-18, 0.0006311571484586124027, 0.001262314296917217216 ),
 .UNSPECIFIED. ) ;
#4011 = B_SPLINE_CURVE_WITH_KNOTS ( 'NONE', 3,
 ( #7728, #12029, #23131, #14166, #7873, #3389, #5256, #22700, #16632, #20937 ),
 .UNSPECIFIED., .F., .F.,
 ( 4, 2, 2, 2, 4 ),
 ( 2.799181570144685938E-16, 0.0003346187017559026423, 0.0006692374035115253436, 0.001003856105267148099, 0.001338474807022770746 ),
 .UNSPECIFIED. ) ;
#4012 = ADVANCED_FACE ( 'NONE', ( #13359 ), #20534, .F. ) ;
#4013 = CARTESIAN_POINT ( 'NONE',  ( -28.41354790283022069, -1.249099604787238249, -23.16239616762930353 ) ) ;
#4014 = CARTESIAN_POINT ( 'NONE',  ( 30.59141879584319312, 70.47510900703926495, -92.40465812955481795 ) ) ;
#4015 = CARTESIAN_POINT ( 'NONE',  ( -28.13707043255157103, 12.83104814250481596, 18.96624908365832596 ) ) ;
#4016 = CARTESIAN_POINT ( 'NONE',  ( -1.323439229708139875, 28.92147054731892908, 35.86372896917441722 ) ) ;
#4017 = ORIENTED_EDGE ( 'NONE', *, *, #5697, .T. ) ;
#4018 = VERTEX_POINT ( 'NONE', #11357 ) ;
#4019 = VERTEX_POINT ( 'NONE', #20130 ) ;
#4020 = CARTESIAN_POINT ( 'NONE',  ( 32.73300124599736449, -115.8010721414085253, 20.69176323058589162 ) ) ;
#4021 = CARTESIAN_POINT ( 'NONE',  ( -20.24399999263414784, 28.55700515887720670, -7.930419334766287243 ) ) ;
#4022 = CARTESIAN_POINT ( 'NONE',  ( -4.178947244162634966, 37.51424432987651159, -31.41809272265936315 ) ) ;
#4023 = FACE_OUTER_BOUND ( 'NONE', #15491, .T. ) ;
#4024 = CARTESIAN_POINT ( 'NONE',  ( 21.16825799904906447, 134.1581724640165305, -18.54093663547691051 ) ) ;
#4025 = ADVANCED_FACE ( 'NONE', ( #9201 ), #23509, .F. ) ;
#4026 = CARTESIAN_POINT ( 'NONE',  ( 1.831572820252008738, 132.9644823688603310, -58.11906524360346538 ) ) ;
#4027 = CARTESIAN_POINT ( 'NONE',  ( 1.831572820252009626, -0.9871191512904484711, -145.1082523917587537 ) ) ;
#4028 = VERTEX_POINT ( 'NONE', #15959 ) ;
#4029 = CARTESIAN_POINT ( 'NONE',  ( 10.93730112726003156, 115.5857507957718440, -97.44200844886164248 ) ) ;
#4030 = CARTESIAN_POINT ( 'NONE',  ( -1.239374126674604337, -45.98822239537608425, -2.406737988130961181 ) ) ;
#4031 = CARTESIAN_POINT ( 'NONE',  ( 14.74894986621300141, -12.50000000000000000, 6.523836839588689598E-17 ) ) ;
#4032 = B_SPLINE_CURVE_WITH_KNOTS ( 'NONE', 3,
 ( #20162, #13976, #16283, #4917, #15854, #22787, #27208, #25082, #879, #24936 ),
 .UNSPECIFIED., .F., .F.,
 ( 4, 3, 3, 4 ),
 ( 0.000000000000000000, 0.0002669560319015713877, 0.0005492286108966342980, 0.0008315040496093477167 ),
 .UNSPECIFIED. ) ;
#4033 = CARTESIAN_POINT ( 'NONE',  ( -20.24419206586953734, -28.55732805495821225, -7.929973069813295972 ) ) ;
#4034 = ADVANCED_FACE ( 'NONE', ( #4881 ), #9884, .F. ) ;
#4035 = ORIENTED_EDGE ( 'NONE', *, *, #26734, .T. ) ;
#4036 = CARTESIAN_POINT ( 'NONE',  ( -2.265401668238146815, 29.73100299756566756, -36.42007794497261841 ) ) ;
#4037 = CARTESIAN_POINT ( 'NONE',  ( 10.93730112725932635, 0.000000000000000000, 0.000000000000000000 ) ) ;
#4038 = ORIENTED_EDGE ( 'NONE', *, *, #2042, .T. ) ;
#4039 = EDGE_CURVE ( 'NONE', #11142, #14288, #847, .T. ) ;
#4040 =( BOUNDED_SURFACE ( )  B_SPLINE_SURFACE ( 3, 1, ( 
 ( #2605, #24082 ),
 ( #26358, #17572 ),
 ( #17994, #10970 ),
 ( #11387, #8663 ) ),
 .UNSPECIFIED., .F., .F., .F. ) 
 B_SPLINE_SURFACE_WITH_KNOTS ( ( 4, 4 ),
 ( 2, 2 ),
 ( 0.000000000000000000, 1.000000000000000000 ),
 ( 0.000000000000000000, 1.000000000000000000 ),
 .UNSPECIFIED. ) 
 GEOMETRIC_REPRESENTATION_ITEM ( )  RATIONAL_B_SPLINE_SURFACE ( (
 ( 1.000000000000000000, 1.000000000000000000),
 ( 0.9593753223639863714, 0.9995975284513187731),
 ( 0.9593753223639863714, 0.9995975284513187731),
 ( 1.000000000000000000, 1.000000000000000000) ) ) 
 REPRESENTATION_ITEM ( '' )  SURFACE ( )  );
#4041 = EDGE_CURVE ( 'NONE', #3038, #9740, #3923, .T. ) ;
#4042 = ORIENTED_EDGE ( 'NONE', *, *, #1496, .F. ) ;
#4043 = EDGE_LOOP ( 'NONE', ( #19556, #7045, #11501, #19826 ) ) ;
#4044 = CARTESIAN_POINT ( 'NONE',  ( 109.1587776205901577, -0.006388631651928916751, 0.003592288931009581399 ) ) ;
#4045 = CARTESIAN_POINT ( 'NONE',  ( 32.73300124599740002, 66.00340565729470654, -97.37344512919790418 ) ) ;
#4046 = DIRECTION ( 'NONE',  ( 0.000000000000000000, -5.223019709708116647E-21, 1.000000000000000000 ) ) ;
#4047 = CARTESIAN_POINT ( 'NONE',  ( 32.73300124599734318, 115.8010721414084117, 20.69176323058669809 ) ) ;
#4048 = ORIENTED_EDGE ( 'NONE', *, *, #17410, .T. ) ;
#4049 = CARTESIAN_POINT ( 'NONE',  ( -1.583189561560255143, 11.94859433442965546, 44.83405390829658188 ) ) ;
#4050 = DIRECTION ( 'NONE',  ( 0.7637818620346800147, 0.6068965246771059752, 0.2198041754873819864 ) ) ;
#4051 = CARTESIAN_POINT ( 'NONE',  ( -1.048996300304498419, -0.7649764263854993418, -45.79145529752469201 ) ) ;
#4052 = CARTESIAN_POINT ( 'NONE',  ( 10.93730112725943293, 128.3908183996590537, 79.81734490845931873 ) ) ;
#4053 = CARTESIAN_POINT ( 'NONE',  ( 28.37603512858453669, 98.45183098818061751, -58.91311972676436426 ) ) ;
#4054 = CARTESIAN_POINT ( 'NONE',  ( 1.834118845439484335, 85.43746956709850338, 117.2918069668803724 ) ) ;
#4055 = VECTOR ( 'NONE', #12893, 1000.000000000000000 ) ;
#4056 = EDGE_CURVE ( 'NONE', #4028, #7451, #24537, .T. ) ;
#4057 = EDGE_LOOP ( 'NONE', ( #21116, #1829, #11427, #63 ) ) ;
#4058 = ADVANCED_FACE ( 'NONE', ( #9359 ), #876, .F. ) ;
#4059 = ORIENTED_EDGE ( 'NONE', *, *, #14405, .F. ) ;
#4060 = CARTESIAN_POINT ( 'NONE',  ( -7.711401346138401003, -52.11446537925908018, 6.030154970217441956 ) ) ;
#4062 = EDGE_LOOP ( 'NONE', ( #24061, #25405, #12345, #15857 ) ) ;
#4061 = CARTESIAN_POINT ( 'NONE',  ( -1.049819825607581691, 45.79654196517400777, -0.5097917909110309953 ) ) ;
#4063 = B_SPLINE_CURVE_WITH_KNOTS ( 'NONE', 3,
 ( #19305, #12018, #18491, #1081, #9869, #18638, #16474, #16541, #2615, #15705 ),
 .UNSPECIFIED., .F., .F.,
 ( 4, 2, 2, 2, 4 ),
 ( 2.602085213965210642E-18, 0.0003346267210630942475, 0.0006692534421261858929, 0.001003880163189277593, 0.001338506884252369184 ),
 .UNSPECIFIED. ) ;
#4064 = ORIENTED_EDGE ( 'NONE', *, *, #6443, .T. ) ;
#4065 = ORIENTED_EDGE ( 'NONE', *, *, #20012, .T. ) ;
#4066 = ORIENTED_EDGE ( 'NONE', *, *, #3220, .F. ) ;
#4067 =( BOUNDED_SURFACE ( )  B_SPLINE_SURFACE ( 3, 1, ( 
 ( #4299, #28454 ),
 ( #1709, #23898 ),
 ( #14947, #17249 ),
 ( #28048, #26173 ) ),
 .UNSPECIFIED., .F., .F., .F. ) 
 B_SPLINE_SURFACE_WITH_KNOTS ( ( 4, 4 ),
 ( 2, 2 ),
 ( 0.000000000000000000, 1.000000000000000000 ),
 ( 0.000000000000000000, 1.000000000000000000 ),
 .UNSPECIFIED. ) 
 GEOMETRIC_REPRESENTATION_ITEM ( )  RATIONAL_B_SPLINE_SURFACE ( (
 ( 1.000000000000000000, 1.000000000000000000),
 ( 0.6386103224230302855, 0.9954351624131538845),
 ( 0.6386103224230302855, 0.9954351624131538845),
 ( 1.000000000000000000, 1.000000000000000000) ) ) 
 REPRESENTATION_ITEM ( '' )  SURFACE ( )  );
#4068 = CARTESIAN_POINT ( 'NONE',  ( 8.186469777910888368, -122.8338388711456872, -84.95702201436542111 ) ) ;
#4069 = B_SPLINE_CURVE_WITH_KNOTS ( 'NONE', 3,
 ( #24631, #13655, #8781, #22455, #2428, #2723 ),
 .UNSPECIFIED., .F., .F.,
 ( 4, 2, 4 ),
 ( 2.602085213965210642E-18, 0.0006311636237756740320, 0.001262327247551345679 ),
 .UNSPECIFIED. ) ;
#4070 = CARTESIAN_POINT ( 'NONE',  ( -55.24271866751342941, 0.009369360294296125852, 0.001545935011630558513 ) ) ;
#4071 = VECTOR ( 'NONE', #13855, 1000.000000000000114 ) ;
#4072 = CARTESIAN_POINT ( 'NONE',  ( -25.21435515916043713, 4.655591116594827383, 34.29329011225949841 ) ) ;
#4073 = CARTESIAN_POINT ( 'NONE',  ( -20.47566338032523348, 7.708089572830403746, -28.85746366088566361 ) ) ;
#4074 = CARTESIAN_POINT ( 'NONE',  ( -23.77929240705206482, -4.877832571065186862, -35.93174012244169546 ) ) ;
#4075 = CARTESIAN_POINT ( 'NONE',  ( -6.588769196390773963, 47.06982923582537381, 20.50531526814514294 ) ) ;
#4076 = B_SPLINE_CURVE_WITH_KNOTS ( 'NONE', 3,
 ( #13503, #2561, #15228, #19984 ),
 .UNSPECIFIED., .F., .F.,
 ( 4, 4 ),
 ( 1.920770561445796063E-16, 0.001982023823822942447 ),
 .UNSPECIFIED. ) ;
#4077 = B_SPLINE_CURVE_WITH_KNOTS ( 'NONE', 3,
 ( #21988, #26170, #26035, #28318, #11196, #10643, #15075, #21858, #2115, #4565 ),
 .UNSPECIFIED., .F., .F.,
 ( 4, 3, 3, 4 ),
 ( 0.001530725384384964971, 0.001531419946797918505, 0.002296279302920153399, 0.003061450627205758099 ),
 .UNSPECIFIED. ) ;
#4078 = CARTESIAN_POINT ( 'NONE',  ( 109.1586900883932856, 0.002301750759607898694, 0.006757191295056137574 ) ) ;
#4079 = CARTESIAN_POINT ( 'NONE',  ( -8.786685647604894456, -23.24040270374358030, 48.22796981442792230 ) ) ;
#4080 = CARTESIAN_POINT ( 'NONE',  ( 2.063896406836609909, -46.16709813092528947, -137.7380992975107290 ) ) ;
#4081 = EDGE_CURVE ( 'NONE', #5582, #21108, #16737, .T. ) ;
#4082 = ORIENTED_EDGE ( 'NONE', *, *, #16857, .F. ) ;
#4083 = VERTEX_POINT ( 'NONE', #18116 ) ;
#4084 = EDGE_CURVE ( 'NONE', #12482, #20441, #705, .T. ) ;
#4086 = CARTESIAN_POINT ( 'NONE',  ( 25.64692872815577118, -91.53575854059458550, 66.10702795113384411 ) ) ;
#4085 = FACE_OUTER_BOUND ( 'NONE', #16480, .T. ) ;
#4087 = CARTESIAN_POINT ( 'NONE',  ( -10.86508079875786414, -50.32133009257452727, 9.118642906269784021 ) ) ;
#4088 = CARTESIAN_POINT ( 'NONE',  ( -1.056502255334265339, -45.80535052436398757, -0.5104472526218417627 ) ) ;
#4089 = CARTESIAN_POINT ( 'NONE',  ( 26.11404676487257603, 110.5078194225161070, 24.64483677384886917 ) ) ;
#4090 = FACE_OUTER_BOUND ( 'NONE', #17882, .T. ) ;
#4091 = ORIENTED_EDGE ( 'NONE', *, *, #992, .F. ) ;
#4092 = CARTESIAN_POINT ( 'NONE',  ( -4.162674018437150458, -3.424137510344606117, 48.79210541969628423 ) ) ;
#4093 = EDGE_CURVE ( 'NONE', #20968, #25314, #24905, .T. ) ;
#4094 = CARTESIAN_POINT ( 'NONE',  ( 25.64681081121879203, -91.59071981940616070, 66.03065707438906884 ) ) ;
#4095 = CARTESIAN_POINT ( 'NONE',  ( -28.41354790283022069, -1.249099604786914286, 23.16239616762932130 ) ) ;
#4096 = ORIENTED_EDGE ( 'NONE', *, *, #21188, .T. ) ;
#4097 = ORIENTED_EDGE ( 'NONE', *, *, #13412, .T. ) ;
#4098 = DIRECTION ( 'NONE',  ( -0.000000000000000000, 1.000000000000000000, 0.000000000000000000 ) ) ;
#4099 = EDGE_CURVE ( 'NONE', #8520, #24828, #7345, .T. ) ;
#4100 = VERTEX_POINT ( 'NONE', #20860 ) ;
#4101 = LINE ( 'NONE', #12866, #18918 ) ;
#4102 = ORIENTED_EDGE ( 'NONE', *, *, #27827, .T. ) ;
#4103 = CARTESIAN_POINT ( 'NONE',  ( -2.911734481061400537, 30.23325065583413718, 36.84482841982617884 ) ) ;
#4104 = ORIENTED_EDGE ( 'NONE', *, *, #24256, .T. ) ;
#4105 = CARTESIAN_POINT ( 'NONE',  ( -1.259920593601971950, 2.243284667987781589, -45.95412615877140894 ) ) ;
#4106 =( BOUNDED_SURFACE ( )  B_SPLINE_SURFACE ( 3, 1, ( 
 ( #27111, #2808 ),
 ( #20360, #3097 ),
 ( #12684, #27409 ),
 ( #11874, #28084 ) ),
 .UNSPECIFIED., .F., .F., .F. ) 
 B_SPLINE_SURFACE_WITH_KNOTS ( ( 4, 4 ),
 ( 2, 2 ),
 ( 0.000000000000000000, 1.000000000000000000 ),
 ( 0.000000000000000000, 1.000000000000000000 ),
 .UNSPECIFIED. ) 
 GEOMETRIC_REPRESENTATION_ITEM ( )  RATIONAL_B_SPLINE_SURFACE ( (
 ( 1.000000000000000000, 1.000000000000000000),
 ( 0.6386103224230316178, 0.9954351624131538845),
 ( 0.6386103224230316178, 0.9954351624131538845),
 ( 1.000000000000000000, 1.000000000000000000) ) ) 
 REPRESENTATION_ITEM ( '' )  SURFACE ( )  );
#4107 = CARTESIAN_POINT ( 'NONE',  ( 109.1721716018069657, -0.01706748904932341507, 0.0002019688922674831401 ) ) ;
#4108 = CARTESIAN_POINT ( 'NONE',  ( -55.24198130335446422, 0.006617369590172447053, -0.006527480770973747085 ) ) ;
#4109 = CARTESIAN_POINT ( 'NONE',  ( -1.048171036023517688, 15.11933492062827966, -43.23005599774305807 ) ) ;
#4110 = CARTESIAN_POINT ( 'NONE',  ( 26.11404676487257603, -112.4785329405481065, -12.95861723607569438 ) ) ;
#4111 = ORIENTED_EDGE ( 'NONE', *, *, #26802, .T. ) ;
#4112 = B_SPLINE_CURVE_WITH_KNOTS ( 'NONE', 3,
 ( #23666, #21334, #3779, #19178, #1613, #10414, #21475 ),
 .UNSPECIFIED., .F., .F.,
 ( 4, 3, 4 ),
 ( 0.000000000000000000, 0.006568092053401836973, 0.02506242213020846987 ),
 .UNSPECIFIED. ) ;
#4113 = B_SPLINE_CURVE_WITH_KNOTS ( 'NONE', 3,
 ( #8427, #8697, #2197, #22229, #17461, #26395, #19349, #11004, #25980, #1923 ),
 .UNSPECIFIED., .F., .F.,
 ( 4, 3, 3, 4 ),
 ( 1.962615573354718958E-17, 0.0002669560319015810371, 0.0005492286108966412369, 0.0008315040496093431630 ),
 .UNSPECIFIED. ) ;
#4114 = DIRECTION ( 'NONE',  ( -1.000000000000000000, -0.000000000000000000, -0.000000000000000000 ) ) ;
#4115 = DIRECTION ( 'NONE',  ( -0.7637818620346801257, 0.02150485345384840416, 0.6451161201712179993 ) ) ;
#4116 = DIRECTION ( 'NONE',  ( 0.000000000000000000, 0.000000000000000000, 1.000000000000000000 ) ) ;
#4117 = ADVANCED_FACE ( 'NONE', ( #1142 ), #4954, .F. ) ;
#4118 = ORIENTED_EDGE ( 'NONE', *, *, #6864, .T. ) ;
#4119 = ORIENTED_EDGE ( 'NONE', *, *, #16176, .T. ) ;
#4120 = CARTESIAN_POINT ( 'NONE',  ( -20.57838717382308147, 7.715628353034087894, 28.96176188950209962 ) ) ;
#4121 = CARTESIAN_POINT ( 'NONE',  ( -1.045287976400362417, 25.66401692420069125, 37.92705037016716574 ) ) ;
#4122 = ADVANCED_FACE ( 'NONE', ( #21281 ), #18402, .F. ) ;
#4124 = CARTESIAN_POINT ( 'NONE',  ( 14.74894986621300141, 20.00000000000000000, 2.618615375249201539E-15 ) ) ;
#4123 = CARTESIAN_POINT ( 'NONE',  ( -25.21435515916025594, 1.749597353048488237E-16, -4.373993382621220594E-17 ) ) ;
#4125 = CARTESIAN_POINT ( 'NONE',  ( 5.340103556456569756, 100.3626145793577678, -108.0219267027620447 ) ) ;
#4126 = CARTESIAN_POINT ( 'NONE',  ( -4.780792508754321268, 3.764354093953580449, -49.38761389561002346 ) ) ;
#4127 = DIRECTION ( 'NONE',  ( -0.5914120900931443270, -0.008020494142990605008, -0.8063295922669344584 ) ) ;
#4128 = ORIENTED_EDGE ( 'NONE', *, *, #10366, .T. ) ;
#4129 = CARTESIAN_POINT ( 'NONE',  ( -1.583189561560255143, -2.490696082059541627, 46.33203782964464068 ) ) ;
#4130 = EDGE_CURVE ( 'NONE', #23678, #3338, #11107, .T. ) ;
#4131 = CARTESIAN_POINT ( 'NONE',  ( -5.986830583229376224, -38.20088153919473939, 33.39046620690945844 ) ) ;
#4132 = CARTESIAN_POINT ( 'NONE',  ( -9.156249394959706578, 48.78605533024773422, 24.29252099376439489 ) ) ;
#4133 = CARTESIAN_POINT ( 'NONE',  ( 1.833809397773873640, 117.2915757704557080, 85.43729755723188646 ) ) ;
#4134 = ORIENTED_EDGE ( 'NONE', *, *, #5570, .T. ) ;
#4135 = CARTESIAN_POINT ( 'NONE',  ( 2.430230287190572103, -133.5180086894995100, 57.85706160874098458 ) ) ;
#4136 = CARTESIAN_POINT ( 'NONE',  ( -2.911734481061388102, 46.11606034418780098, 12.03743348210733011 ) ) ;
#4137 = ORIENTED_EDGE ( 'NONE', *, *, #3641, .F. ) ;
#4138 = CARTESIAN_POINT ( 'NONE',  ( 19.66333377628710366, -88.78556591841228851, -105.3186440504705104 ) ) ;
#4139 = CARTESIAN_POINT ( 'NONE',  ( 26.11404676487257603, -90.92995828888153653, -67.46175819463459788 ) ) ;
#4140 = FACE_BOUND ( 'NONE', #26124, .T. ) ;
#4141 = CARTESIAN_POINT ( 'NONE',  ( -22.23342874802668589, -20.31166691703108285, 24.24669006619395617 ) ) ;
#4142 = CARTESIAN_POINT ( 'NONE',  ( 32.73300124599732186, 0.000000000000000000, 0.000000000000000000 ) ) ;
#4143 = DIRECTION ( 'NONE',  ( 0.000000000000000000, -5.223019709708190374E-21, 1.000000000000000000 ) ) ;
#4144 =( BOUNDED_SURFACE ( )  B_SPLINE_SURFACE ( 3, 1, ( 
 ( #20270, #2272 ),
 ( #22451, #7059 ),
 ( #8932, #24625 ),
 ( #26743, #562 ) ),
 .UNSPECIFIED., .F., .F., .F. ) 
 B_SPLINE_SURFACE_WITH_KNOTS ( ( 4, 4 ),
 ( 2, 2 ),
 ( 0.000000000000000000, 1.000000000000000000 ),
 ( 0.000000000000000000, 1.000000000000000000 ),
 .UNSPECIFIED. ) 
 GEOMETRIC_REPRESENTATION_ITEM ( )  RATIONAL_B_SPLINE_SURFACE ( (
 ( 1.000000000000000000, 1.000000000000000000),
 ( 0.6386103224230302855, 0.9954351624131538845),
 ( 0.6386103224230302855, 0.9954351624131538845),
 ( 1.000000000000000000, 1.000000000000000000) ) ) 
 REPRESENTATION_ITEM ( '' )  SURFACE ( )  );
#4145 = CARTESIAN_POINT ( 'NONE',  ( 1.894214914920965276, 132.2104617488244855, -59.90782071839061729 ) ) ;
#4146 = CARTESIAN_POINT ( 'NONE',  ( 13.36082413113063083, 142.1654513177088006, 56.35051087435012818 ) ) ;
#4147 = CARTESIAN_POINT ( 'NONE',  ( 16.05277956358201763, 25.20902801311569164, -141.0713346807232824 ) ) ;
#4148 = CARTESIAN_POINT ( 'NONE',  ( 109.1592201516379674, 0.007376275279030877242, 0.002720803050361335265 ) ) ;
#4149 = CARTESIAN_POINT ( 'NONE',  ( -8.786685647604890903, -25.35688121747466184, 47.14957014837381166 ) ) ;
#4150 = CARTESIAN_POINT ( 'NONE',  ( -20.20700224038492721, -23.35150625415671755, -18.19058640100215385 ) ) ;
#4151 = DIRECTION ( 'NONE',  ( -0.7637818620346801257, -0.3965875333584914508, -0.5092696688508597802 ) ) ;
#4152 = CARTESIAN_POINT ( 'NONE',  ( -1.259920593601975058, -45.95412615877143026, -2.243284667987618608 ) ) ;
#4153 = ORIENTED_EDGE ( 'NONE', *, *, #24527, .F. ) ;
#4154 = CONICAL_SURFACE ( 'NONE', #473, 34.60786435723138510, 0.8559913436420825139 ) ;
#4155 = ORIENTED_EDGE ( 'NONE', *, *, #26437, .F. ) ;
#4156 = CARTESIAN_POINT ( 'NONE',  ( 25.64703792032471341, 103.2099561461823924, 45.78915563622597062 ) ) ;
#4157 = CARTESIAN_POINT ( 'NONE',  ( 21.16825799904898986, -121.8625396241600782, 59.09063383105294776 ) ) ;
#4158 = EDGE_CURVE ( 'NONE', #28263, #1461, #18987, .T. ) ;
#4159 = CARTESIAN_POINT ( 'NONE',  ( 1.832998868059890096, -85.72499093308179852, 117.0819875546692685 ) ) ;
#4160 = CARTESIAN_POINT ( 'NONE',  ( 1.832998868059858122, 59.50898020732511640, 132.3466930259795618 ) ) ;
#4161 = CARTESIAN_POINT ( 'NONE',  ( -55.24390624410018802, 0.01032895241566708991, 0.001451500391952845713 ) ) ;
#4162 = CARTESIAN_POINT ( 'NONE',  ( 1.834118845439484335, -141.9759513273462517, -29.99597360113214961 ) ) ;
#4163 = CARTESIAN_POINT ( 'NONE',  ( 30.58324630866341209, -45.56259622822436484, 112.0331114996533870 ) ) ;
#4164 = ORIENTED_EDGE ( 'NONE', *, *, #20786, .T. ) ;
#4165 = CARTESIAN_POINT ( 'NONE',  ( -21.41430102051751305, -23.81424706376350287, 19.54553566814611898 ) ) ;
#4166 = DIRECTION ( 'NONE',  ( 0.000000000000000000, -1.000000000000000000, 0.000000000000000000 ) ) ;
#4167 = CIRCLE ( 'NONE', #30, 12.50000000000000178 ) ;
#4168 = CARTESIAN_POINT ( 'NONE',  ( 25.64692872815576052, 23.79008960806752881, -110.3764733653606100 ) ) ;
#4169 = ADVANCED_FACE ( 'NONE', ( #8068 ), #15447, .F. ) ;
#4170 = ADVANCED_FACE ( 'NONE', ( #12355 ), #2013, .F. ) ;
#4171 = PLANE ( 'NONE',  #15311 ) ;
#4172 = ORIENTED_EDGE ( 'NONE', *, *, #492, .F. ) ;
#4173 = CARTESIAN_POINT ( 'NONE',  ( 2.108393763691172040, 43.67806918959143303, 138.5721856399486569 ) ) ;
#4174 = CARTESIAN_POINT ( 'NONE',  ( -1.046935749539996907, 1.275486069320473481, -45.77872888003166452 ) ) ;
#4175 = ORIENTED_EDGE ( 'NONE', *, *, #18823, .F. ) ;
#4176 = B_SPLINE_CURVE_WITH_KNOTS ( 'NONE', 3,
 ( #7575, #9870, #25125, #5393 ),
 .UNSPECIFIED., .F., .F.,
 ( 4, 4 ),
 ( 1.895855152355442610E-16, 0.001982023823822946784 ),
 .UNSPECIFIED. ) ;
#4177 = B_SPLINE_CURVE_WITH_KNOTS ( 'NONE', 3,
 ( #15732, #24545, #4808, #24112, #13574, #22376, #19763, #2639 ),
 .UNSPECIFIED., .F., .F.,
 ( 4, 2, 2, 4 ),
 ( 0.000000000000000000, 0.002761524886576656283, 0.005523049773153312567, 0.01104609954630661126 ),
 .UNSPECIFIED. ) ;
#4178 = VERTEX_POINT ( 'NONE', #5760 ) ;
#4179 = ORIENTED_EDGE ( 'NONE', *, *, #25398, .F. ) ;
#4180 = AXIS2_PLACEMENT_3D ( 'NONE', #15022, #12860, #2198 ) ;
#4181 = VECTOR ( 'NONE', #13356, 1000.000000000000000 ) ;
#4182 = CARTESIAN_POINT ( 'NONE',  ( 10.93730112725932635, 0.000000000000000000, 0.000000000000000000 ) ) ;
#4183 = CARTESIAN_POINT ( 'NONE',  ( -25.21435515916043713, 30.48034229288662544, 16.39063784838709736 ) ) ;
#4184 = AXIS2_PLACEMENT_3D ( 'NONE', #27737, #25725, #16659 ) ;
#4185 = CARTESIAN_POINT ( 'NONE',  ( 10.93730112725932635, 0.000000000000000000, 0.000000000000000000 ) ) ;
#4186 = DIRECTION ( 'NONE',  ( -0.5946245182733608248, -0.5994612328333145390, -0.5357871896547512502 ) ) ;
#4187 = EDGE_LOOP ( 'NONE', ( #24508, #21758, #21090, #24399 ) ) ;
#4188 = EDGE_LOOP ( 'NONE', ( #17368, #5551, #26613, #20631 ) ) ;
#4189 = CARTESIAN_POINT ( 'NONE',  ( -55.24300891470648622, -0.007734635432132420246, -0.006048736206180634067 ) ) ;
#4190 = CARTESIAN_POINT ( 'NONE',  ( -25.21435515916043713, 23.92354251275973809, 25.00736669480994934 ) ) ;
#4191 = EDGE_CURVE ( 'NONE', #8983, #14341, #17904, .T. ) ;
#4192 = CARTESIAN_POINT ( 'NONE',  ( -25.21435515916043002, 4.655591116594353984, -34.29329011225956947 ) ) ;
#4193 = CARTESIAN_POINT ( 'NONE',  ( 109.1586900883932856, 0.006819617742893400482, 0.002109621908814826672 ) ) ;
#4194 = DIRECTION ( 'NONE',  ( 0.7563875759206388771, -0.3556158456312938365, -0.5490129373055243622 ) ) ;
#4195 = CIRCLE ( 'NONE', #24429, 151.1787379149930359 ) ;
#4196 = VECTOR ( 'NONE', #21161, 999.9999999999998863 ) ;
#4197 = CARTESIAN_POINT ( 'NONE',  ( -1.045287976400383290, -44.00138577190632816, 12.68782741917368106 ) ) ;
#4198 = CARTESIAN_POINT ( 'NONE',  ( -24.53237795827005741, 30.86653739599987745, -14.09663893005569513 ) ) ;
#4199 = ORIENTED_EDGE ( 'NONE', *, *, #19249, .T. ) ;
#4200 = CIRCLE ( 'NONE', #2354, 37.50000000000001421 ) ;
#4201 = ORIENTED_EDGE ( 'NONE', *, *, #16418, .F. ) ;
#4202 = FACE_OUTER_BOUND ( 'NONE', #3222, .T. ) ;
#4203 = CARTESIAN_POINT ( 'NONE',  ( 26.11404676487257603, -36.06104232266378062, -107.3263591096434197 ) ) ;
#4204 = B_SPLINE_CURVE_WITH_KNOTS ( 'NONE', 3,
 ( #8079, #20999, #1154, #18999, #21143, #18850 ),
 .UNSPECIFIED., .F., .F.,
 ( 4, 2, 4 ),
 ( 1.396102177145585797E-16, 0.003570751334075633089, 0.007141502668151126533 ),
 .UNSPECIFIED. ) ;
#4205 = ORIENTED_EDGE ( 'NONE', *, *, #28000, .T. ) ;
#4206 = APPLICATION_CONTEXT ( 'automotive_design' ) ;
#4207 = ORIENTED_EDGE ( 'NONE', *, *, #26690, .F. ) ;
#4208 = ORIENTED_EDGE ( 'NONE', *, *, #10241, .T. ) ;
#4209 = CARTESIAN_POINT ( 'NONE',  ( 1.832998868059890096, -85.72499093308022111, -117.0819875546704054 ) ) ;
#4210 = CARTESIAN_POINT ( 'NONE',  ( 109.1586900883932856, 0.006231977675084991036, 0.003481399864218453783 ) ) ;
#4211 = CARTESIAN_POINT ( 'NONE',  ( -1.539763995773683503, 2.469814354917492238, -46.22267697748602444 ) ) ;
#4212 = CARTESIAN_POINT ( 'NONE',  ( 109.1586059443104944, -0.001740416220250516881, 0.006856640434645976979 ) ) ;
#4213 = EDGE_CURVE ( 'NONE', #24090, #4630, #14146, .T. ) ;
#4214 = CARTESIAN_POINT ( 'NONE',  ( -20.57838717382308147, -25.16001208503093522, 16.28767523336148315 ) ) ;
#4215 = ADVANCED_FACE ( 'NONE', ( #19258 ), #1666, .F. ) ;
#4216 = CARTESIAN_POINT ( 'NONE',  ( 109.1589550718175161, -0.007453082872782207380, -0.001354998915253747844 ) ) ;
#4217 = CARTESIAN_POINT ( 'NONE',  ( 10.93730112725932635, 0.000000000000000000, 0.000000000000000000 ) ) ;
#4218 = CARTESIAN_POINT ( 'NONE',  ( -12.82751273423881777, 23.15139349681311387, -43.04932478553539710 ) ) ;
#4219 = ADVANCED_FACE ( 'NONE', ( #13056 ), #19659, .F. ) ;
#4220 = CARTESIAN_POINT ( 'NONE',  ( 2.430230287190572103, -137.9371479820459570, -46.34481016236966155 ) ) ;
#4221 = CARTESIAN_POINT ( 'NONE',  ( -1.050229599974477290, 26.71319688967688322, 37.20249516760145525 ) ) ;
#4222 = VERTEX_POINT ( 'NONE', #20089 ) ;
#4223 = ORIENTED_EDGE ( 'NONE', *, *, #14943, .T. ) ;
#4224 = CARTESIAN_POINT ( 'NONE',  ( 25.98107933586721074, -57.50946808479307037, 97.42660475433937961 ) ) ;
#4225 = FACE_OUTER_BOUND ( 'NONE', #9612, .T. ) ;
#4226 = CARTESIAN_POINT ( 'NONE',  ( 109.1592201516379674, 0.002720803050370466849, 0.007376275279032907736 ) ) ;
#4227 = DIRECTION ( 'NONE',  ( -1.000000000000000000, -0.000000000000000000, -0.000000000000000000 ) ) ;
#4228 = CARTESIAN_POINT ( 'NONE',  ( 55.79472521941426777, 54.55111121764146986, -48.13855120843829383 ) ) ;
#4229 = VERTEX_POINT ( 'NONE', #2104 ) ;
#4230 = CARTESIAN_POINT ( 'NONE',  ( 5.340103579038292025, 146.3832392131354538, -17.70136536264517346 ) ) ;
#4231 = CARTESIAN_POINT ( 'NONE',  ( -8.259864102781673267, 25.58601832199082793, -46.42816643551579148 ) ) ;
#4232 = CARTESIAN_POINT ( 'NONE',  ( 28.37603512858358101, 113.9023475466376993, -13.77584568114176911 ) ) ;
#4233 = ORIENTED_EDGE ( 'NONE', *, *, #14255, .F. ) ;
#4234 = ORIENTED_EDGE ( 'NONE', *, *, #15831, .T. ) ;
#4235 = B_SPLINE_CURVE_WITH_KNOTS ( 'NONE', 3,
 ( #13600, #2517, #11309, #7506 ),
 .UNSPECIFIED., .F., .F.,
 ( 4, 4 ),
 ( 1.309227883336067538E-16, 0.008383748772659583778 ),
 .UNSPECIFIED. ) ;
#4236 = CARTESIAN_POINT ( 'NONE',  ( -4.780792508754325709, -11.68149851467495637, -48.13366140756553335 ) ) ;
#4237 = AXIS2_PLACEMENT_3D ( 'NONE', #21930, #26242, #8985 ) ;
#4238 = CARTESIAN_POINT ( 'NONE',  ( 1.832998868059858122, 117.7096351258387870, 84.86110816369641441 ) ) ;
#4239 = CIRCLE ( 'NONE', #6118, 151.1787379149930359 ) ;
#4240 = VERTEX_POINT ( 'NONE', #28301 ) ;
#4241 = CARTESIAN_POINT ( 'NONE',  ( 2.433796855181219243, -125.2830755159749003, -74.00833731765692391 ) ) ;
#4242 = ADVANCED_FACE ( 'NONE', ( #4273 ), #7938, .F. ) ;
#4243 = EDGE_LOOP ( 'NONE', ( #17406, #14074, #28264, #6167 ) ) ;
#4244 = CARTESIAN_POINT ( 'NONE',  ( 1.833485406944043827, 125.9346397303445286, -72.09189602597577107 ) ) ;
#4245 = CARTESIAN_POINT ( 'NONE',  ( 109.1624594426973118, -0.003771499231554190090, -0.01551217196237749882 ) ) ;
#4246 = EDGE_CURVE ( 'NONE', #10890, #1025, #8601, .T. ) ;
#4247 = CARTESIAN_POINT ( 'NONE',  ( -1.056502255334265339, -27.33667001641142846, 36.75727364034761990 ) ) ;
#4248 = B_SPLINE_CURVE_WITH_KNOTS ( 'NONE', 3,
 ( #1349, #19063, #4068, #5685 ),
 .UNSPECIFIED., .F., .F.,
 ( 4, 4 ),
 ( 3.406435548571490246E-16, 0.01077107486149829138 ),
 .UNSPECIFIED. ) ;
#4249 = CARTESIAN_POINT ( 'NONE',  ( 1.833485406944057594, -125.9346397303430223, -72.09189602597842850 ) ) ;
#4250 = CARTESIAN_POINT ( 'NONE',  ( -1.045287976400351981, 12.68782741917293855, -44.00138577190654132 ) ) ;
#4251 = LINE ( 'NONE', #26270, #6966 ) ;
#4252 = ORIENTED_EDGE ( 'NONE', *, *, #25667, .F. ) ;
#4253 = AXIS2_PLACEMENT_3D ( 'NONE', #22795, #5351, #13691 ) ;
#4254 = ADVANCED_FACE ( 'NONE', ( #10906 ), #18591, .F. ) ;
#4255 = CARTESIAN_POINT ( 'NONE',  ( 2.433796855181205476, 145.5024947199069629, 1.451562450950146133 ) ) ;
#4256 = CARTESIAN_POINT ( 'NONE',  ( -1.619063947482197729, 46.30105812165548684, -2.489035965910316506 ) ) ;
#4257 = CARTESIAN_POINT ( 'NONE',  ( 25.64681081121880624, -56.81519825470823548, 97.57530875170583329 ) ) ;
#4258 = CONICAL_SURFACE ( 'NONE', #10278, 117.6351876552689504, 0.9945805576725580410 ) ;
#4259 = ORIENTED_EDGE ( 'NONE', *, *, #21504, .F. ) ;
#4260 = EDGE_LOOP ( 'NONE', ( #28343, #1817, #15465, #11529 ) ) ;
#4261 = CARTESIAN_POINT ( 'NONE',  ( 26.28373643307439167, 122.5382646256984600, 35.44121223574892099 ) ) ;
#4262 = CARTESIAN_POINT ( 'NONE',  ( 1.833838850093452599, -72.55487854850780138, 125.6687428896156575 ) ) ;
#4263 = CARTESIAN_POINT ( 'NONE',  ( 25.98552792386800903, -76.50165414343506143, -83.35136888841310565 ) ) ;
#4264 = CARTESIAN_POINT ( 'NONE',  ( -1.619063947482197729, 2.489035965910159298, -46.30105812165548684 ) ) ;
#4265 = CARTESIAN_POINT ( 'NONE',  ( 1.893872463202044054, -137.7483215415845450, -45.75900850850141666 ) ) ;
#4266 = VERTEX_POINT ( 'NONE', #17234 ) ;
#4267 = CARTESIAN_POINT ( 'NONE',  ( 109.1586900883932856, -0.004113747441000954568, -0.005833932871487501094 ) ) ;
#4268 = DIRECTION ( 'NONE',  ( 0.000000000000000000, 5.223019709707975211E-21, -1.000000000000000000 ) ) ;
#4269 = CARTESIAN_POINT ( 'NONE',  ( 109.1587776205901577, -0.005880209827417018538, -0.004375189885414149799 ) ) ;
#4270 = DIRECTION ( 'NONE',  ( -0.5914120900931443270, -0.6045864222316674752, -0.5335794202785283380 ) ) ;
#4271 = CARTESIAN_POINT ( 'NONE',  ( 25.64692232868535626, 75.30916867847216167, -84.12764974007949093 ) ) ;
#4272 = VERTEX_POINT ( 'NONE', #17365 ) ;
#4273 = FACE_OUTER_BOUND ( 'NONE', #12342, .T. ) ;
#4274 = CARTESIAN_POINT ( 'NONE',  ( 1.833809397773842553, 15.34508223002640293, -144.2961330457378324 ) ) ;
#4275 = CARTESIAN_POINT ( 'NONE',  ( -1.619063947482197729, -35.99532424477357750, 29.22875152547795707 ) ) ;
#4277 =( BOUNDED_SURFACE ( )  B_SPLINE_SURFACE ( 3, 1, ( 
 ( #6656, #15403 ),
 ( #24213, #12551 ),
 ( #23668, #3922 ),
 ( #12690, #21476 ) ),
 .UNSPECIFIED., .F., .F., .F. ) 
 B_SPLINE_SURFACE_WITH_KNOTS ( ( 4, 4 ),
 ( 2, 2 ),
 ( 0.000000000000000000, 1.000000000000000000 ),
 ( 0.000000000000000000, 1.000000000000000000 ),
 .UNSPECIFIED. ) 
 GEOMETRIC_REPRESENTATION_ITEM ( )  RATIONAL_B_SPLINE_SURFACE ( (
 ( 1.000000000000000000, 1.000000000000000000),
 ( 0.9934239774497837239, 0.8357310067453919133),
 ( 0.9934239774497837239, 0.8357310067453919133),
 ( 1.000000000000000000, 1.000000000000000000) ) ) 
 REPRESENTATION_ITEM ( '' )  SURFACE ( )  );
#4276 = AXIS2_PLACEMENT_3D ( 'NONE', #14490, #23010, #25593 ) ;
#4278 = EDGE_LOOP ( 'NONE', ( #2965, #23842, #21093, #10180 ) ) ;
#4279 = CARTESIAN_POINT ( 'NONE',  ( 26.11404676487257603, 33.91085499298520034, -108.0249973236464314 ) ) ;
#4280 = CIRCLE ( 'NONE', #19920, 151.1787379149930359 ) ;
#4281 = ADVANCED_FACE ( 'NONE', ( #23882 ), #921, .F. ) ;
#4282 = CARTESIAN_POINT ( 'NONE',  ( 2.430230287190572103, -57.85706160874057247, -133.5180086894997089 ) ) ;
#4283 = DIRECTION ( 'NONE',  ( -1.000000000000000000, -0.000000000000000000, -0.000000000000000000 ) ) ;
#4284 = AXIS2_PLACEMENT_3D ( 'NONE', #20582, #3456, #9378 ) ;
#4285 = ADVANCED_FACE ( 'NONE', ( #6870 ), #15606, .F. ) ;
#4286 = ORIENTED_EDGE ( 'NONE', *, *, #20495, .F. ) ;
#4287 = CARTESIAN_POINT ( 'NONE',  ( 1.833485406944057594, -117.0814567582550154, 85.72460230293657446 ) ) ;
#4288 = CARTESIAN_POINT ( 'NONE',  ( -1.259972190295306715, 35.85909728507050431, -28.82609802125271514 ) ) ;
#4289 = EDGE_CURVE ( 'NONE', #20108, #24250, #4884, .T. ) ;
#4290 = CARTESIAN_POINT ( 'NONE',  ( 26.11404676487257603, -76.59696442953135431, -83.38016054979861735 ) ) ;
#4291 = CARTESIAN_POINT ( 'NONE',  ( 1.833838850855474600, -137.9800888515320025, -44.92600961247803326 ) ) ;
#4292 = CARTESIAN_POINT ( 'NONE',  ( 26.28373643307403285, 22.43832507403829979, -125.5716026420345628 ) ) ;
#4293 = CARTESIAN_POINT ( 'NONE',  ( -8.786685647604890903, 7.199674155858966529, -53.04920435127184675 ) ) ;
#4294 = B_SPLINE_CURVE_WITH_KNOTS ( 'NONE', 3,
 ( #26012, #23873, #1959, #6300, #26284, #22110 ),
 .UNSPECIFIED., .F., .F.,
 ( 4, 2, 4 ),
 ( 1.734723475976806902E-18, 0.0006311636237756703457, 0.001262327247551338957 ),
 .UNSPECIFIED. ) ;
#4295 = CARTESIAN_POINT ( 'NONE',  ( 109.1592201516379674, 0.001934867487012827689, -0.007620268632968149602 ) ) ;
#4296 = ADVANCED_FACE ( 'NONE', ( #26991 ), #952, .T. ) ;
#4297 = AXIS2_PLACEMENT_3D ( 'NONE', #18698, #9933, #20423 ) ;
#4298 = CARTESIAN_POINT ( 'NONE',  ( 6.224689322667630975, 97.14981701196322206, 111.7293398381268332 ) ) ;
#4299 = CARTESIAN_POINT ( 'NONE',  ( 109.1592201516379674, -0.004194960840990111066, -0.006649399203953448162 ) ) ;
#4300 = CARTESIAN_POINT ( 'NONE',  ( -8.786685647604898008, 48.22796981442802178, 23.24040270374343464 ) ) ;
#4301 = ORIENTED_EDGE ( 'NONE', *, *, #15886, .F. ) ;
#4302 = ORIENTED_EDGE ( 'NONE', *, *, #5207, .F. ) ;
#4303 = ORIENTED_EDGE ( 'NONE', *, *, #27041, .T. ) ;
#4304 = CARTESIAN_POINT ( 'NONE',  ( -20.90916690077944295, 39.20864005633548999, -5.322316104228152156 ) ) ;
#4305 = CARTESIAN_POINT ( 'NONE',  ( -1.045287976400365970, -36.12803364096568259, 28.14015102489869591 ) ) ;
#4306 = CARTESIAN_POINT ( 'NONE',  ( 30.59141879584286627, -95.58042137919495929, 66.10404588653759106 ) ) ;
#4307 = CARTESIAN_POINT ( 'NONE',  ( 26.11404676487259024, 103.8885755249569485, 45.01677474591446781 ) ) ;
#4308 = CARTESIAN_POINT ( 'NONE',  ( 26.11404676487259024, -12.95861723607377414, -112.4785329405483338 ) ) ;
#4309 = CARTESIAN_POINT ( 'NONE',  ( -24.53239521893647890, -24.99972072650158950, -22.94500969220225883 ) ) ;
#4310 = ORIENTED_EDGE ( 'NONE', *, *, #28261, .F. ) ;
#4311 = CARTESIAN_POINT ( 'NONE',  ( -18.41936578851711204, -7.566034416291083531, -41.75701384111729197 ) ) ;
#4312 = CARTESIAN_POINT ( 'NONE',  ( 6.224689322667630975, 57.86870174583425808, 136.2818611715192390 ) ) ;
#4313 = CARTESIAN_POINT ( 'NONE',  ( -1.048994561756786625, -36.59609844253148481, -27.53485040342882328 ) ) ;
#4314 = LINE ( 'NONE', #27820, #22526 ) ;
#4315 = CARTESIAN_POINT ( 'NONE',  ( -1.259972190295305827, -43.01178231151318698, 16.33417789844418522 ) ) ;
#4316 = VERTEX_POINT ( 'NONE', #810 ) ;
#4317 = DIRECTION ( 'NONE',  ( 0.000000000000000000, 0.000000000000000000, 1.000000000000000000 ) ) ;
#4318 = CARTESIAN_POINT ( 'NONE',  ( -1.031422197589716205, -12.69107518035533211, -44.01264471863842687 ) ) ;
#4319 = VERTEX_POINT ( 'NONE', #2830 ) ;
#4320 = B_SPLINE_CURVE_WITH_KNOTS ( 'NONE', 3,
 ( #9038, #4991, #26577, #18089, #387, #6881, #26867, #15625, #7176, #13767 ),
 .UNSPECIFIED., .F., .F.,
 ( 4, 3, 3, 4 ),
 ( 6.938893903907228378E-18, 0.0002669560319015712793, 0.0005492286108966453568, 0.0008315040496093611608 ),
 .UNSPECIFIED. ) ;
#4321 = ORIENTED_EDGE ( 'NONE', *, *, #4888, .T. ) ;
#4322 = ORIENTED_EDGE ( 'NONE', *, *, #1372, .F. ) ;
#4323 = EDGE_CURVE ( 'NONE', #24455, #4923, #10042, .T. ) ;
#4324 = CARTESIAN_POINT ( 'NONE',  ( -22.23342874802668589, 11.82490389046315116, -29.33662284748865900 ) ) ;
#4325 = CARTESIAN_POINT ( 'NONE',  ( 109.1624594426973260, -0.01154818537150952180, -0.01102230012606015934 ) ) ;
#4326 = CARTESIAN_POINT ( 'NONE',  ( -7.733045908741340568, 21.80378472388487054, -47.75066202881800592 ) ) ;
#4327 = EDGE_CURVE ( 'NONE', #6430, #24062, #26830, .T. ) ;
#4328 = B_SPLINE_CURVE_WITH_KNOTS ( 'NONE', 3,
 ( #2679, #9458, #26855, #26993, #14044, #16063, #24864 ),
 .UNSPECIFIED., .F., .F.,
 ( 4, 3, 4 ),
 ( 0.000000000000000000, 0.02398743853561337291, 0.04000277880656209761 ),
 .UNSPECIFIED. ) ;
#4329 = VERTEX_POINT ( 'NONE', #18511 ) ;
#4330 = CARTESIAN_POINT ( 'NONE',  ( -6.588769196390752647, 34.04709086065316370, -38.42957692275855663 ) ) ;
#4331 = CARTESIAN_POINT ( 'NONE',  ( 5.340103556456461398, -111.1041836730285013, 96.93942141426026637 ) ) ;
#4332 = VERTEX_POINT ( 'NONE', #9456 ) ;
#4333 = CARTESIAN_POINT ( 'NONE',  ( -1.049819825607587909, -43.71263398674761191, -13.66706894614421408 ) ) ;
#4334 = CARTESIAN_POINT ( 'NONE',  ( 1.833691583653552115, -44.50270951807451070, -138.1170938425796351 ) ) ;
#4335 = CARTESIAN_POINT ( 'NONE',  ( 2.433796855181205476, -96.28145139437610567, -109.1007109081235882 ) ) ;
#4336 = CARTESIAN_POINT ( 'NONE',  ( 1.831572820252009626, -144.4165162501762154, -14.18623102066916175 ) ) ;
#4337 = CARTESIAN_POINT ( 'NONE',  ( 1.833809397773857208, 97.22957127128982791, -107.7184108265653748 ) ) ;
#4338 = CARTESIAN_POINT ( 'NONE',  ( -1.155031165708885199, -35.88345263711027400, 28.62780465193348789 ) ) ;
#4339 = CARTESIAN_POINT ( 'NONE',  ( -7.078251931573406708, 26.33626633876224332, -44.92740138729174504 ) ) ;
#4340 = FACE_OUTER_BOUND ( 'NONE', #25012, .T. ) ;
#4341 = CARTESIAN_POINT ( 'NONE',  ( 1.894214914920945070, 141.7768822502890487, -31.11059045488991970 ) ) ;
#4342 = CARTESIAN_POINT ( 'NONE',  ( 109.1624594426973118, 0.007576898892907089726, -0.01405141589344816727 ) ) ;
#4343 = VERTEX_POINT ( 'NONE', #22854 ) ;
#4344 = ORIENTED_EDGE ( 'NONE', *, *, #23367, .F. ) ;
#4345 = CARTESIAN_POINT ( 'NONE',  ( 25.98552792386799482, -24.57669147553907152, -110.4352299692912851 ) ) ;
#4346 = DIRECTION ( 'NONE',  ( 0.000000000000000000, 0.000000000000000000, 1.000000000000000000 ) ) ;
#4347 = VERTEX_POINT ( 'NONE', #15923 ) ;
#4348 = B_SPLINE_CURVE_WITH_KNOTS ( 'NONE', 3,
 ( #17709, #6794, #162, #15538, #24353, #26626 ),
 .UNSPECIFIED., .F., .F.,
 ( 4, 2, 4 ),
 ( 1.389302603484999005E-17, 0.0006311571484586108848, 0.001262314296917207892 ),
 .UNSPECIFIED. ) ;
#4349 = ORIENTED_EDGE ( 'NONE', *, *, #16479, .F. ) ;
#4350 = ORIENTED_EDGE ( 'NONE', *, *, #3879, .F. ) ;
#4351 = EDGE_CURVE ( 'NONE', #25928, #16492, #5613, .T. ) ;
#4352 = B_SPLINE_CURVE_WITH_KNOTS ( 'NONE', 3,
 ( #16486, #27274, #1091, #1509 ),
 .UNSPECIFIED., .F., .F.,
 ( 4, 4 ),
 ( 3.743959683027022744E-16, 0.01077107486149797219 ),
 .UNSPECIFIED. ) ;
#4353 = CARTESIAN_POINT ( 'NONE',  ( 109.1592201516379674, 0.007748443302128555504, -0.001331853079208340871 ) ) ;
#4354 = EDGE_CURVE ( 'NONE', #7314, #24805, #6270, .T. ) ;
#4355 = CARTESIAN_POINT ( 'NONE',  ( 1.894214914920941739, -144.2521558665608836, 16.12044375672241614 ) ) ;
#4356 = CARTESIAN_POINT ( 'NONE',  ( 8.186469777910877710, -148.8557359139593359, -12.15801985874125712 ) ) ;
#4357 = ADVANCED_FACE ( 'NONE', ( #25014 ), #21787, .T. ) ;
#4358 = CARTESIAN_POINT ( 'NONE',  ( -1.323830074806773283, -46.01435746200692023, -2.318057800980537930 ) ) ;
#4359 = CARTESIAN_POINT ( 'NONE',  ( -1.031422197589711987, 37.93675465142509040, 25.67058493451400381 ) ) ;
#4360 = CARTESIAN_POINT ( 'NONE',  ( 109.1587776205901861, -0.004240403845331913203, 0.005978137617721826502 ) ) ;
#4361 = B_SPLINE_CURVE_WITH_KNOTS ( 'NONE', 3,
 ( #17009, #15116, #1747, #14856, #4337, #8393, #17289, #26076, #21901, #10 ),
 .UNSPECIFIED., .F., .F.,
 ( 4, 3, 3, 4 ),
 ( 5.003707553108401214E-17, 0.0002669559177086260862, 0.0005339118354151285457, 0.001067817517169155576 ),
 .UNSPECIFIED. ) ;
#4362 = CARTESIAN_POINT ( 'NONE',  ( 5.340103579038192549, -133.7487108093468180, 62.06990748397801383 ) ) ;
#4363 = CARTESIAN_POINT ( 'NONE',  ( -2.904412668506661355, 36.79926976721492338, 30.27712468694946679 ) ) ;
#4364 = ADVANCED_FACE ( 'NONE', ( #24862 ), #3693, .F. ) ;
#4365 = CARTESIAN_POINT ( 'NONE',  ( -4.473127245936431073, 49.22197550883368677, 3.196405119333978639 ) ) ;
#4366 = CARTESIAN_POINT ( 'NONE',  ( 25.81918753295378366, 113.0221398901142180, -0.9336804662331048554 ) ) ;
#4367 = CARTESIAN_POINT ( 'NONE',  ( 25.64681081121879203, -107.5125461021405044, 34.49579773461748999 ) ) ;
#4368 = EDGE_LOOP ( 'NONE', ( #129, #17004, #23082, #1339 ) ) ;
#4369 = ORIENTED_EDGE ( 'NONE', *, *, #1466, .F. ) ;
#4371 = CARTESIAN_POINT ( 'NONE',  ( -1.050230347699842692, 1.897926697972695375E-16, 45.79907861674080749 ) ) ;
#4370 = CARTESIAN_POINT ( 'NONE',  ( -55.24300891470648622, 0.005486913146696770563, 0.008142823778062024953 ) ) ;
#4372 = DIRECTION ( 'NONE',  ( -1.000000000000000000, -0.000000000000000000, -0.000000000000000000 ) ) ;
#4373 = CARTESIAN_POINT ( 'NONE',  ( -4.162674018437136247, 11.82104147411627970, 47.46216648493545165 ) ) ;
#4374 = CARTESIAN_POINT ( 'NONE',  ( -1.259972190295306715, 35.85909728507050431, -28.82609802125271514 ) ) ;
#4375 = ORIENTED_EDGE ( 'NONE', *, *, #8741, .F. ) ;
#4376 = CARTESIAN_POINT ( 'NONE',  ( -6.588769196390775740, -4.956336548259307584, 51.10255870850478033 ) ) ;
#4377 = CARTESIAN_POINT ( 'NONE',  ( -6.574463467970654840, -25.96726214983158698, 44.27173031830760408 ) ) ;
#4378 = B_SPLINE_CURVE_WITH_KNOTS ( 'NONE', 3,
 ( #25364, #27799, #14548, #12115 ),
 .UNSPECIFIED., .F., .F.,
 ( 4, 4 ),
 ( 3.408235012970691066E-16, 0.01077107486149795484 ),
 .UNSPECIFIED. ) ;
#4379 = CARTESIAN_POINT ( 'NONE',  ( -1.048994561756786625, -36.59609844253148481, -27.53485040342882328 ) ) ;
#4380 = EDGE_LOOP ( 'NONE', ( #18765, #21029, #17766, #19437 ) ) ;
#4381 = ORIENTED_EDGE ( 'NONE', *, *, #23992, .F. ) ;
#4382 = CARTESIAN_POINT ( 'NONE',  ( 109.1586059443104944, 0.0004635842312796052884, -0.007058870754606104241 ) ) ;
#4383 = EDGE_CURVE ( 'NONE', #5017, #2997, #28219, .T. ) ;
#4384 = VERTEX_POINT ( 'NONE', #16643 ) ;
#4385 = CARTESIAN_POINT ( 'NONE',  ( 25.64670758986456889, 107.2298587623395747, 35.36461833156559464 ) ) ;
#4386 = ORIENTED_EDGE ( 'NONE', *, *, #22231, .T. ) ;
#4387 = EDGE_CURVE ( 'NONE', #3680, #14349, #16798, .T. ) ;
#4388 = CARTESIAN_POINT ( 'NONE',  ( -55.24271866751342941, -0.009369360294295348696, -0.001545935011630817420 ) ) ;
#4389 = AXIS2_PLACEMENT_3D ( 'NONE', #25541, #12279, #3360 ) ;
#4390 = EDGE_LOOP ( 'NONE', ( #12911, #6574, #19206, #11360 ) ) ;
#4391 = CARTESIAN_POINT ( 'NONE',  ( -1.045287976400365970, 1.530335034933814731, -45.76855895860946788 ) ) ;
#4392 = CARTESIAN_POINT ( 'NONE',  ( -20.57838717382308147, 18.89542499756500149, -23.26537097894111383 ) ) ;
#4393 = CARTESIAN_POINT ( 'NONE',  ( 109.1589550718174877, -0.003980125429499926232, 0.006445391216542559892 ) ) ;
#4394 = CARTESIAN_POINT ( 'NONE',  ( 26.11404676487257603, 55.62948129436244926, 98.61392875273382685 ) ) ;
#4395 = CARTESIAN_POINT ( 'NONE',  ( 25.65782528836479415, -112.2379831684171592, -12.37768345530092162 ) ) ;
#4396 = CARTESIAN_POINT ( 'NONE',  ( 25.64681081121879203, -103.3177883989776547, -45.54494737132326776 ) ) ;
#4397 = DIRECTION ( 'NONE',  ( 0.7563875759206388771, 0.2351350468682867345, -0.6104009704506935252 ) ) ;
#4398 = CARTESIAN_POINT ( 'NONE',  ( 25.64708010899963853, -56.40825696968328629, 97.81137751680981296 ) ) ;
#4399 = CARTESIAN_POINT ( 'NONE',  ( 26.11404676487259024, -67.46175819463304890, -90.92995828888270182 ) ) ;
#4401 = CARTESIAN_POINT ( 'NONE',  ( -7.711401346138398338, 21.83927363365101115, 47.70038152767067885 ) ) ;
#4400 = CARTESIAN_POINT ( 'NONE',  ( -20.57838717382308147, 29.92853265176831812, -1.611677988432464126 ) ) ;
#4402 = CARTESIAN_POINT ( 'NONE',  ( 16.75465622695659818, 67.05928661304356808, 125.4242432475195272 ) ) ;
#4403 = CARTESIAN_POINT ( 'NONE',  ( 24.01988960052077005, 129.0012934948648535, -23.05141021591152750 ) ) ;
#4404 = CARTESIAN_POINT ( 'NONE',  ( -1.619063947482201282, 16.67502769180561728, -43.26576862488438735 ) ) ;
#4405 = EDGE_LOOP ( 'NONE', ( #25662, #3057, #2102, #24293 ) ) ;
#4406 = CARTESIAN_POINT ( 'NONE',  ( 25.64692232868534560, -35.20209749635233720, -107.2834780834839137 ) ) ;
#4407 = CARTESIAN_POINT ( 'NONE',  ( 109.1592201516379674, 0.002720803050370466849, 0.007376275279032907736 ) ) ;
#4408 = DIRECTION ( 'NONE',  ( -1.000000000000000000, 6.938893903907226837E-18, -1.734723475976806709E-18 ) ) ;
#4409 = CARTESIAN_POINT ( 'NONE',  ( 25.64708010899965984, 112.2984447178532719, 11.74803558238322410 ) ) ;
#4410 = CARTESIAN_POINT ( 'NONE',  ( 25.64704443564075120, 110.4715096490036075, -23.34498572103212410 ) ) ;
#4411 = ORIENTED_EDGE ( 'NONE', *, *, #16647, .F. ) ;
#4412 = CARTESIAN_POINT ( 'NONE',  ( 1.831572820252008738, 29.20415387690568210, 142.1425225354580846 ) ) ;
#4413 = EDGE_CURVE ( 'NONE', #9705, #2306, #14614, .T. ) ;
#4414 = EDGE_CURVE ( 'NONE', #5134, #1484, #21335, .T. ) ;
#4415 = CARTESIAN_POINT ( 'NONE',  ( 9.884929003653608603, -97.56484214660547138, -114.6392083957127994 ) ) ;
#4416 = CARTESIAN_POINT ( 'NONE',  ( 14.74894986621300319, -1.025372615548127706E-16, 37.50000000000001421 ) ) ;
#4417 = ORIENTED_EDGE ( 'NONE', *, *, #14095, .F. ) ;
#4418 = CARTESIAN_POINT ( 'NONE',  ( 2.433796855181219243, 31.67151202413165478, -142.0211193075552956 ) ) ;
#4419 = CARTESIAN_POINT ( 'NONE',  ( 2.063896406836609909, -98.19887492195788070, -107.0521644432427593 ) ) ;
#4420 = ORIENTED_EDGE ( 'NONE', *, *, #16578, .F. ) ;
#4421 = CARTESIAN_POINT ( 'NONE',  ( -7.078251931573400491, 51.82710018979476274, 5.101176922830847893 ) ) ;
#4422 = CARTESIAN_POINT ( 'NONE',  ( 2.433796855181233454, -98.43889364293788447, -107.1581411821795626 ) ) ;
#4423 = CARTESIAN_POINT ( 'NONE',  ( -1.539760825549685519, -46.22267384399379608, 2.469813586483570855 ) ) ;
#4424 = CARTESIAN_POINT ( 'NONE',  ( 55.49584447822657296, -48.74506217377918205, 53.73688382046248080 ) ) ;
#4425 = CARTESIAN_POINT ( 'NONE',  ( 28.37599760073042532, 22.09615888373955528, 112.5845136272806428 ) ) ;
#4426 = CARTESIAN_POINT ( 'NONE',  ( 1.833809397773871419, -132.6366580004811340, 58.85883548850542013 ) ) ;
#4427 = CARTESIAN_POINT ( 'NONE',  ( 25.64681081121880624, -112.3352186517031441, 11.38886654529637887 ) ) ;
#4428 = CARTESIAN_POINT ( 'NONE',  ( -20.90916690077962414, -7.054312691028722604, 38.93431874629081335 ) ) ;
#4429 = DIRECTION ( 'NONE',  ( 0.5914120900931444380, 0.7023121577978154173, -0.3962188444547216082 ) ) ;
#4430 = CARTESIAN_POINT ( 'NONE',  ( -15.02187109954782507, 41.75590530176335591, 20.12219089991046772 ) ) ;
#4431 = EDGE_LOOP ( 'NONE', ( #6276, #12961, #6313, #22162, #18688, #8431, #27158, #10091, #2470, #5610, #8737, #14048, #1153, #27707, #4887, #24334, #24264, #5022, #23742, #6988, #15471, #14898, #20508, #26497, #18801, #20527, #26502, #20113, #11498, #15763, #22030, #12006, #13227, #7405, #26020, #22858, #2911, #4017, #22291, #20008, #12905, #12007, #17086, #1366, #13395, #15127, #15827, #25654, #9398, #4980, #26215, #14720, #15165, #7769, #6031, #19298, #19635, #26676, #12025, #27991, #8603, #10889, #27269, #18075 ) ) ;
#4432 = VERTEX_POINT ( 'NONE', #3962 ) ;
#4433 = CARTESIAN_POINT ( 'NONE',  ( -1.050230346682680782, -26.91946103437133431, -37.05264119692680680 ) ) ;
#4434 = DIRECTION ( 'NONE',  ( 0.5914120900931444380, -0.3352908775637255534, 0.7333565075147320256 ) ) ;
#4435 = LINE ( 'NONE', #27919, #15562 ) ;
#4436 = CARTESIAN_POINT ( 'NONE',  ( -15.02187109954788191, -45.60876405941872491, 8.264310930412850809 ) ) ;
#4437 = DIRECTION ( 'NONE',  ( -1.000000000000000000, -0.000000000000000000, -0.000000000000000000 ) ) ;
#4438 = CARTESIAN_POINT ( 'NONE',  ( 25.64692872815577473, -91.15762468787696093, -66.62748454953252519 ) ) ;
#4439 = ORIENTED_EDGE ( 'NONE', *, *, #26328, .F. ) ;
#4440 = CARTESIAN_POINT ( 'NONE',  ( -8.786685647604887350, 53.04920435127183254, -7.199674155859138835 ) ) ;
#4441 = CARTESIAN_POINT ( 'NONE',  ( -8.786685647604885574, 6.096987947571466530E-17, -1.524246986892866633E-17 ) ) ;
#4442 = CARTESIAN_POINT ( 'NONE',  ( -1.045287976400383290, -36.12803364096628655, -28.14015102489793918 ) ) ;
#4443 = EDGE_CURVE ( 'NONE', #744, #5523, #24097, .T. ) ;
#4444 = CARTESIAN_POINT ( 'NONE',  ( 109.1624594426973118, 0.008380433676412918365, 0.01358749486988785130 ) ) ;
#4445 = EDGE_CURVE ( 'NONE', #12449, #6247, #6631, .T. ) ;
#4446 = CARTESIAN_POINT ( 'NONE',  ( 1.833691583653554336, -0.3559373310805032387, 145.1092556475514073 ) ) ;
#4447 = CARTESIAN_POINT ( 'NONE',  ( 32.73300124599738581, 51.32617430725051832, -105.8473486001045387 ) ) ;
#4448 =( BOUNDED_SURFACE ( )  B_SPLINE_SURFACE ( 3, 1, ( 
 ( #13585, #22384 ),
 ( #26540, #22241 ),
 ( #9000, #343 ),
 ( #20062, #2649 ) ),
 .UNSPECIFIED., .F., .F., .F. ) 
 B_SPLINE_SURFACE_WITH_KNOTS ( ( 4, 4 ),
 ( 2, 2 ),
 ( 0.000000000000000000, 1.000000000000000000 ),
 ( 0.000000000000000000, 1.000000000000000000 ),
 .UNSPECIFIED. ) 
 GEOMETRIC_REPRESENTATION_ITEM ( )  RATIONAL_B_SPLINE_SURFACE ( (
 ( 1.000000000000000000, 1.000000000000000000),
 ( 0.9956975270656955868, 0.8568959468854907557),
 ( 0.9956975270656955868, 0.8568959468854907557),
 ( 1.000000000000000000, 1.000000000000000000) ) ) 
 REPRESENTATION_ITEM ( '' )  SURFACE ( )  );
#4449 = ORIENTED_EDGE ( 'NONE', *, *, #16387, .T. ) ;
#4451 = EDGE_CURVE ( 'NONE', #14777, #5273, #21240, .T. ) ;
#4450 = CARTESIAN_POINT ( 'NONE',  ( -20.47566338032516597, 18.81547714195514232, 23.19796701701855213 ) ) ;
#4452 = VERTEX_POINT ( 'NONE', #3677 ) ;
#4453 = EDGE_CURVE ( 'NONE', #3161, #21238, #25714, .T. ) ;
#4454 = ORIENTED_EDGE ( 'NONE', *, *, #26196, .T. ) ;
#4455 = ORIENTED_EDGE ( 'NONE', *, *, #4745, .F. ) ;
#4456 = CARTESIAN_POINT ( 'NONE',  ( -23.79223135445720061, 13.25822371132295352, -30.42557260166815780 ) ) ;
#4457 = CARTESIAN_POINT ( 'NONE',  ( 2.063896406836605024, 98.19887492196005496, -107.0521644432407129 ) ) ;
#4458 = CARTESIAN_POINT ( 'NONE',  ( -1.619063947482201282, 16.67502769180561728, -43.26576862488438735 ) ) ;
#4459 = ORIENTED_EDGE ( 'NONE', *, *, #3935, .F. ) ;
#4460 = CARTESIAN_POINT ( 'NONE',  ( 55.49584447822657296, 42.42793568432957585, 58.85239198729202315 ) ) ;
#4461 = CARTESIAN_POINT ( 'NONE',  ( -20.20612091757422490, -1.137293889216157705, 29.57813639663779171 ) ) ;
#4462 = CARTESIAN_POINT ( 'NONE',  ( -20.57838717382308147, -25.16001208503117326, -16.28767523336112433 ) ) ;
#4463 = VERTEX_POINT ( 'NONE', #6146 ) ;
#4464 = CARTESIAN_POINT ( 'NONE',  ( 25.64681081121879203, 91.59071981940572016, 66.03065707438965148 ) ) ;
#4465 = ORIENTED_EDGE ( 'NONE', *, *, #21086, .T. ) ;
#4466 = FACE_OUTER_BOUND ( 'NONE', #10979, .T. ) ;
#4467 = CARTESIAN_POINT ( 'NONE',  ( -1.056502255334265339, -13.66916755949880802, -43.72121397317219049 ) ) ;
#4468 = DIRECTION ( 'NONE',  ( 0.000000000000000000, 0.000000000000000000, 1.000000000000000000 ) ) ;
#4469 = B_SPLINE_CURVE_WITH_KNOTS ( 'NONE', 3,
 ( #19661, #234, #13049, #4547, #367, #2374, #8733, #6863, #15608, #4696 ),
 .UNSPECIFIED., .F., .F.,
 ( 4, 2, 2, 2, 4 ),
 ( 2.879654849182128713E-16, 0.0003346187017559071959, 0.0006692374035115264278, 0.001003856105267145714, 0.001338474807022764891 ),
 .UNSPECIFIED. ) ;
#4470 = LINE ( 'NONE', #2298, #16619 ) ;
#4471 = CARTESIAN_POINT ( 'NONE',  ( -1.045287976400365970, -36.12803364096568259, 28.14015102489869591 ) ) ;
#4472 = CARTESIAN_POINT ( 'NONE',  ( -20.37983603106074426, -24.94323704205426040, 16.25728007463434110 ) ) ;
#4473 = ADVANCED_FACE ( 'NONE', ( #1521 ), #11775, .F. ) ;
#4474 = CARTESIAN_POINT ( 'NONE',  ( -55.25719721206881729, -0.008651607285659737578, -0.007063345920777289004 ) ) ;
#4475 = DIRECTION ( 'NONE',  ( -1.000000000000000000, -0.000000000000000000, -0.000000000000000000 ) ) ;
#4476 = CARTESIAN_POINT ( 'NONE',  ( 2.263178607246655982, -43.59477707254128376, 138.7064943909644228 ) ) ;
#4477 = ORIENTED_EDGE ( 'NONE', *, *, #561, .F. ) ;
#4478 =( BOUNDED_SURFACE ( )  B_SPLINE_SURFACE ( 3, 1, ( 
 ( #13783, #22886 ),
 ( #9620, #27166 ),
 ( #18103, #11923 ),
 ( #406, #18383 ) ),
 .UNSPECIFIED., .F., .F., .F. ) 
 B_SPLINE_SURFACE_WITH_KNOTS ( ( 4, 4 ),
 ( 2, 2 ),
 ( 0.000000000000000000, 1.000000000000000000 ),
 ( 0.000000000000000000, 1.000000000000000000 ),
 .UNSPECIFIED. ) 
 GEOMETRIC_REPRESENTATION_ITEM ( )  RATIONAL_B_SPLINE_SURFACE ( (
 ( 1.000000000000000000, 1.000000000000000000),
 ( 0.9934239774497838349, 0.8357310067453913582),
 ( 0.9934239774497838349, 0.8357310067453913582),
 ( 1.000000000000000000, 1.000000000000000000) ) ) 
 REPRESENTATION_ITEM ( '' )  SURFACE ( )  );
#4479 = ORIENTED_EDGE ( 'NONE', *, *, #22480, .F. ) ;
#4481 = ADVANCED_FACE ( 'NONE', ( #8030 ), #14756, .T. ) ;
#4480 = DIRECTION ( 'NONE',  ( -1.000000000000000000, -0.000000000000000000, -0.000000000000000000 ) ) ;
#4482 = CARTESIAN_POINT ( 'NONE',  ( 32.73300124599740002, 97.37344512919945316, -66.00340565729239017 ) ) ;
#4483 = ORIENTED_EDGE ( 'NONE', *, *, #17565, .F. ) ;
#4484 = EDGE_LOOP ( 'NONE', ( #10422, #24697, #1564, #454 ) ) ;
#4485 = ORIENTED_EDGE ( 'NONE', *, *, #19473, .T. ) ;
#4486 = CARTESIAN_POINT ( 'NONE',  ( 1.834118845439484335, -85.43746956709772178, -117.2918069668809409 ) ) ;
#4487 = B_SPLINE_CURVE_WITH_KNOTS ( 'NONE', 3,
 ( #25618, #14514, #3016, #11796, #14365, #3572, #5894, #12353 ),
 .UNSPECIFIED., .F., .F.,
 ( 4, 2, 2, 4 ),
 ( 6.938893903907228378E-18, 0.0002429592666046848646, 0.0004859185332093627903, 0.0009718370664186809114 ),
 .UNSPECIFIED. ) ;
#4488 = CARTESIAN_POINT ( 'NONE',  ( 1.831572820252009626, -138.3111855986058174, -43.90210991190762257 ) ) ;
#4489 = CARTESIAN_POINT ( 'NONE',  ( 109.1624594426973260, 0.005372302061310704584, -0.01503296564240499435 ) ) ;
#4490 = CARTESIAN_POINT ( 'NONE',  ( 1.832998868059858122, -145.1092030902949830, 0.5339089137742969449 ) ) ;
#4491 = CARTESIAN_POINT ( 'NONE',  ( -1.031422197589711764, 25.67058493451497725, 37.93675465142443670 ) ) ;
#4492 = CARTESIAN_POINT ( 'NONE',  ( -20.90916690077962414, -7.054312691028722604, 38.93431874629081335 ) ) ;
#4493 = CARTESIAN_POINT ( 'NONE',  ( -1.046936909428682005, 1.275306677858881743, 45.77873603877004882 ) ) ;
#4494 = CARTESIAN_POINT ( 'NONE',  ( -4.780792508754322157, 37.74278713234441796, 32.07473752860738614 ) ) ;
#4495 = CARTESIAN_POINT ( 'NONE',  ( 30.58324630866342275, -102.7123253644120240, 63.85566901681581697 ) ) ;
#4496 = CARTESIAN_POINT ( 'NONE',  ( -1.046935749540015115, 37.78548154587994645, -25.87617179820928826 ) ) ;
#4497 = CARTESIAN_POINT ( 'NONE',  ( -6.588769196390775740, -4.956336548259307584, 51.10255870850478033 ) ) ;
#4498 = ORIENTED_EDGE ( 'NONE', *, *, #2627, .T. ) ;
#4499 = ORIENTED_EDGE ( 'NONE', *, *, #21053, .T. ) ;
#4501 = CARTESIAN_POINT ( 'NONE',  ( -4.473127245936431073, 41.70021447285055416, -26.34600523034553277 ) ) ;
#4500 = CARTESIAN_POINT ( 'NONE',  ( 25.64681081121879203, 91.10197563707947666, 66.70335573067896462 ) ) ;
#4502 = EDGE_CURVE ( 'NONE', #21576, #22983, #13798, .T. ) ;
#4503 = CARTESIAN_POINT ( 'NONE',  ( 28.37599760073042887, 78.09498850373518053, -84.05168479399007708 ) ) ;
#4504 = CARTESIAN_POINT ( 'NONE',  ( -1.155001620486265645, 38.31519699443499150, -25.28075036143234300 ) ) ;
#4505 = CARTESIAN_POINT ( 'NONE',  ( -20.57838717382308147, 10.78122205917000365, -27.96569011373090063 ) ) ;
#4506 = CARTESIAN_POINT ( 'NONE',  ( 26.28373643307404706, -119.9673604189460150, 43.35364178852736217 ) ) ;
#4507 = ORIENTED_EDGE ( 'NONE', *, *, #14591, .T. ) ;
#4508 = CARTESIAN_POINT ( 'NONE',  ( 1.833206308920111161, 145.1075835660717530, 0.7447049373416791962 ) ) ;
#4509 = ORIENTED_EDGE ( 'NONE', *, *, #26096, .F. ) ;
#4511 = EDGE_CURVE ( 'NONE', #16646, #11340, #16569, .T. ) ;
#4510 = CARTESIAN_POINT ( 'NONE',  ( 2.430230287190581429, 84.35270093935257307, 118.5711603495684301 ) ) ;
#4512 = CARTESIAN_POINT ( 'NONE',  ( -55.24340739397742084, -0.0007387096945734077319, 0.01010924026184317238 ) ) ;
#4513 = ORIENTED_EDGE ( 'NONE', *, *, #25597, .F. ) ;
#4514 = ORIENTED_EDGE ( 'NONE', *, *, #18115, .T. ) ;
#4515 = ADVANCED_FACE ( 'NONE', ( #13019 ), #24479, .F. ) ;
#4516 = CARTESIAN_POINT ( 'NONE',  ( -55.24271866751342941, -0.006757859501009782881, 0.006671293903667897471 ) ) ;
#4517 = ORIENTED_EDGE ( 'NONE', *, *, #3394, .T. ) ;
#4518 = EDGE_LOOP ( 'NONE', ( #10149, #3727, #9614, #26366 ) ) ;
#4519 = B_SPLINE_CURVE_WITH_KNOTS ( 'NONE', 3,
 ( #1353, #27264, #10158, #14022, #14596, #9572 ),
 .UNSPECIFIED., .F., .F.,
 ( 4, 2, 4 ),
 ( 0.000000000000000000, 0.003570751334075647834, 0.007141502668151295669 ),
 .UNSPECIFIED. ) ;
#4520 = AXIS2_PLACEMENT_3D ( 'NONE', #21412, #10484, #12625 ) ;
#4521 =( BOUNDED_SURFACE ( )  B_SPLINE_SURFACE ( 3, 1, ( 
 ( #26616, #20433 ),
 ( #16108, #15969 ),
 ( #22764, #3028 ),
 ( #11806, #15672 ) ),
 .UNSPECIFIED., .F., .F., .F. ) 
 B_SPLINE_SURFACE_WITH_KNOTS ( ( 4, 4 ),
 ( 2, 2 ),
 ( 0.000000000000000000, 1.000000000000000000 ),
 ( 0.000000000000000000, 1.000000000000000000 ),
 .UNSPECIFIED. ) 
 GEOMETRIC_REPRESENTATION_ITEM ( )  RATIONAL_B_SPLINE_SURFACE ( (
 ( 1.000000000000000000, 1.000000000000000000),
 ( 0.9934239774497838349, 0.8357310067453913582),
 ( 0.9934239774497838349, 0.8357310067453913582),
 ( 1.000000000000000000, 1.000000000000000000) ) ) 
 REPRESENTATION_ITEM ( '' )  SURFACE ( )  );
#4522 = CARTESIAN_POINT ( 'NONE',  ( -55.24300891470650754, -0.009439835024158502175, -0.002702093572893477045 ) ) ;
#4523 = CIRCLE ( 'NONE', #4982, 117.6351876552689504 ) ;
#4524 = ORIENTED_EDGE ( 'NONE', *, *, #23885, .T. ) ;
#4525 = CARTESIAN_POINT ( 'NONE',  ( 2.063896406836609909, 98.19887492195857703, 107.0521644432420771 ) ) ;
#4526 = EDGE_CURVE ( 'NONE', #14115, #18577, #22426, .T. ) ;
#4527 = LINE ( 'NONE', #11298, #23527 ) ;
#4528 = CARTESIAN_POINT ( 'NONE',  ( 14.74894986621300319, -1.023413983156987147E-16, 2.558534957892467869E-17 ) ) ;
#4529 = CARTESIAN_POINT ( 'NONE',  ( -90.83090735639699176, 0.000000000000000000, 0.000000000000000000 ) ) ;
#4530 = CARTESIAN_POINT ( 'NONE',  ( -19.53423201713129842, 1.355459634611817431E-16, -3.388649086529543578E-17 ) ) ;
#4531 = CARTESIAN_POINT ( 'NONE',  ( -55.24340739397742794, -0.0007387096945702591004, -0.01010924026184094153 ) ) ;
#4532 = EDGE_CURVE ( 'NONE', #28478, #24539, #20398, .T. ) ;
#4533 = CARTESIAN_POINT ( 'NONE',  ( -25.21435515916043357, -25.00736669481038987, -23.92354251275926558 ) ) ;
#4535 = CARTESIAN_POINT ( 'NONE',  ( 6.224689322667647851, -28.26953958630718944, 145.3353551538640716 ) ) ;
#4534 = CARTESIAN_POINT ( 'NONE',  ( 109.1587776205901577, 0.007151389024634738009, 0.001605238040359060429 ) ) ;
#4536 = CARTESIAN_POINT ( 'NONE',  ( 32.73300124599732186, 0.000000000000000000, 0.000000000000000000 ) ) ;
#4537 = B_SPLINE_CURVE_WITH_KNOTS ( 'NONE', 3,
 ( #11701, #27073, #24813, #10122, #1325, #3065, #18891, #27663, #13848, #25232 ),
 .UNSPECIFIED., .F., .F.,
 ( 4, 2, 2, 2, 4 ),
 ( 3.104682540412587095E-18, 0.0003346267210630946812, 0.0006692534421261863266, 0.001003880163189277809, 0.001338506884252369401 ),
 .UNSPECIFIED. ) ;
#4538 = VERTEX_POINT ( 'NONE', #23844 ) ;
#4539 = DIRECTION ( 'NONE',  ( 1.000000000000000000, -6.938893903907226837E-18, 1.734723475976806709E-18 ) ) ;
#4540 = CARTESIAN_POINT ( 'NONE',  ( -1.050229599974477512, -27.12684363859229109, 36.90196321294325799 ) ) ;
#4541 = ADVANCED_FACE ( 'NONE', ( #19500 ), #21945, .T. ) ;
#4542 = CARTESIAN_POINT ( 'NONE',  ( 10.93730112725990367, -145.2260730187398678, -42.00474393596407197 ) ) ;
#4543 = FACE_OUTER_BOUND ( 'NONE', #4746, .T. ) ;
#4544 = CARTESIAN_POINT ( 'NONE',  ( -1.619063947482197729, 11.94059994246222622, 44.80407745103770623 ) ) ;
#4545 = ADVANCED_FACE ( 'NONE', ( #21657 ), #21517, .F. ) ;
#4546 = ORIENTED_EDGE ( 'NONE', *, *, #22833, .F. ) ;
#4547 = CARTESIAN_POINT ( 'NONE',  ( -1.113548883309557924, 16.03115934825529010, -42.96943836789110094 ) ) ;
#4548 = CARTESIAN_POINT ( 'NONE',  ( -1.239374126674604337, -45.98822239537607715, 2.406737988131604666 ) ) ;
#4549 = CARTESIAN_POINT ( 'NONE',  ( 109.1586059443104944, -0.004378796245583073746, 0.005555961672780045102 ) ) ;
#4550 = VERTEX_POINT ( 'NONE', #21516 ) ;
#4551 = B_SPLINE_CURVE_WITH_KNOTS ( 'NONE', 3,
 ( #25342, #16844, #5767, #27620, #1573, #7941 ),
 .UNSPECIFIED., .F., .F.,
 ( 4, 2, 4 ),
 ( 3.565531997320606436E-16, 0.003576372551511159629, 0.007152745103021962772 ),
 .UNSPECIFIED. ) ;
#4552 = CARTESIAN_POINT ( 'NONE',  ( -28.13707043255157103, -22.88591869784691823, -0.7675454997506192534 ) ) ;
#4553 = VERTEX_POINT ( 'NONE', #8997 ) ;
#4554 = CARTESIAN_POINT ( 'NONE',  ( 25.64699802086726166, -112.9109702078779804, 0.2377811728593887397 ) ) ;
#4555 = DIRECTION ( 'NONE',  ( 0.5946245182733607137, -0.3297108033645317349, 0.7332888028688893112 ) ) ;
#4556 = CARTESIAN_POINT ( 'NONE',  ( 2.433796855181233454, 74.00833731765563073, 125.2830755159756677 ) ) ;
#4557 = VERTEX_POINT ( 'NONE', #6407 ) ;
#4558 = CARTESIAN_POINT ( 'NONE',  ( 10.93730112725932813, 146.7718404940640085, 36.23586118136551448 ) ) ;
#4559 = EDGE_CURVE ( 'NONE', #1868, #8689, #22246, .T. ) ;
#4560 = CARTESIAN_POINT ( 'NONE',  ( 25.81918753295378721, 55.70247894228311480, -98.34688456803341694 ) ) ;
#4561 = VECTOR ( 'NONE', #21442, 1000.000000000000114 ) ;
#4562 = DIRECTION ( 'NONE',  ( 0.5914120900931444380, -0.5335794202785220097, -0.6045864222316730263 ) ) ;
#4563 = CARTESIAN_POINT ( 'NONE',  ( 10.93730112725932635, 149.7554878793145576, 20.69552240458357062 ) ) ;
#4564 = CARTESIAN_POINT ( 'NONE',  ( -4.178947244162636743, -3.367451375481460563, -48.81675275154075422 ) ) ;
#4565 = CARTESIAN_POINT ( 'NONE',  ( -1.045287976400362417, -1.530335034933495653, 45.76855895860946788 ) ) ;
#4566 = ORIENTED_EDGE ( 'NONE', *, *, #11450, .T. ) ;
#4567 = CARTESIAN_POINT ( 'NONE',  ( 109.1586900883932856, -0.0008465529156635612316, -0.007088091345229652514 ) ) ;
#4568 = EDGE_CURVE ( 'NONE', #26336, #5981, #8652, .T. ) ;
#4569 = CARTESIAN_POINT ( 'NONE',  ( 109.1592201516379674, 0.001934867487021726170, 0.007620268632971113378 ) ) ;
#4570 = DIRECTION ( 'NONE',  ( 0.000000000000000000, -1.000000000000000000, -3.469446951953603342E-16 ) ) ;
#4571 = CARTESIAN_POINT ( 'NONE',  ( 25.69398547355839924, -98.18017599249800753, -55.82723250638873225 ) ) ;
#4572 = ORIENTED_EDGE ( 'NONE', *, *, #17863, .F. ) ;
#4573 = EDGE_CURVE ( 'NONE', #5967, #565, #19632, .T. ) ;
#4574 = ORIENTED_EDGE ( 'NONE', *, *, #22168, .F. ) ;
#4575 = ORIENTED_EDGE ( 'NONE', *, *, #7110, .T. ) ;
#4576 = CARTESIAN_POINT ( 'NONE',  ( 25.64699802086725811, 103.2460182674617073, 45.70780507840472495 ) ) ;
#4577 = CARTESIAN_POINT ( 'NONE',  ( 2.433796855181205476, -43.58222566461547132, -138.8296532063092457 ) ) ;
#4578 = CARTESIAN_POINT ( 'NONE',  ( -1.323830074806762402, -38.58891736138512840, 25.17121255494518550 ) ) ;
#4579 = EDGE_CURVE ( 'NONE', #12327, #22671, #15898, .T. ) ;
#4580 = CARTESIAN_POINT ( 'NONE',  ( 109.1587776205901577, 0.005978137617714225811, -0.004240403845337380184 ) ) ;
#4581 = CARTESIAN_POINT ( 'NONE',  ( -1.619063947482197729, 43.26576862488456499, 16.67502769180516964 ) ) ;
#4582 = CARTESIAN_POINT ( 'NONE',  ( 32.73300124599738581, -97.37344512919901263, 66.00340565729310072 ) ) ;
#4583 = EDGE_LOOP ( 'NONE', ( #7020, #24783, #23179, #25598 ) ) ;
#4584 = CARTESIAN_POINT ( 'NONE',  ( 25.64681081121879203, -34.49579773461710630, -107.5125461021406181 ) ) ;
#4585 = CARTESIAN_POINT ( 'NONE',  ( -7.711401346138398338, -10.36923727626085423, 51.42722225669433556 ) ) ;
#4586 = CARTESIAN_POINT ( 'NONE',  ( 25.64704443564076897, -0.1334765861211750504, 112.9111375659905718 ) ) ;
#4587 = CARTESIAN_POINT ( 'NONE',  ( 109.1586900883932856, 0.002301750759599777586, -0.006757191295060853420 ) ) ;
#4588 = CARTESIAN_POINT ( 'NONE',  ( 55.49584447822657296, 72.55110015779771970, 0.2676470673959223112 ) ) ;
#4589 = CARTESIAN_POINT ( 'NONE',  ( 13.36082413113063083, 150.7747251079861996, 25.56125765253504412 ) ) ;
#4590 = ORIENTED_EDGE ( 'NONE', *, *, #12843, .F. ) ;
#4591 = CARTESIAN_POINT ( 'NONE',  ( -8.786685647604890903, 23.24040270374391426, -48.22796981442777309 ) ) ;
#4592 = B_SPLINE_CURVE_WITH_KNOTS ( 'NONE', 3,
 ( #8842, #24960, #23355, #26813, #763, #5223, #16161 ),
 .UNSPECIFIED., .F., .F.,
 ( 4, 3, 4 ),
 ( 8.845388854693243284E-18, 0.009512539173626400127, 0.02506242213020845599 ),
 .UNSPECIFIED. ) ;
#4593 = CARTESIAN_POINT ( 'NONE',  ( -4.473127245936434626, 26.34600523034538355, -41.70021447285062521 ) ) ;
#4594 = ORIENTED_EDGE ( 'NONE', *, *, #25940, .T. ) ;
#4595 = ORIENTED_EDGE ( 'NONE', *, *, #22315, .T. ) ;
#4596 = ORIENTED_EDGE ( 'NONE', *, *, #5243, .T. ) ;
#4597 = DIRECTION ( 'NONE',  ( -1.000000000000000000, -0.000000000000000000, -0.000000000000000000 ) ) ;
#4598 = FACE_OUTER_BOUND ( 'NONE', #817, .T. ) ;
#4599 = CARTESIAN_POINT ( 'NONE',  ( -2.265401668238149036, 17.02144111536879123, -43.82493763960390254 ) ) ;
#4600 = EDGE_CURVE ( 'NONE', #6599, #9129, #3872, .T. ) ;
#4601 = AXIS2_PLACEMENT_3D ( 'NONE', #15131, #6880, #2111 ) ;
#4602 =( BOUNDED_SURFACE ( )  B_SPLINE_SURFACE ( 3, 1, ( 
 ( #26235, #6533 ),
 ( #1500, #15286 ),
 ( #24102, #4365 ),
 ( #10311, #17870 ) ),
 .UNSPECIFIED., .F., .F., .F. ) 
 B_SPLINE_SURFACE_WITH_KNOTS ( ( 4, 4 ),
 ( 2, 2 ),
 ( 0.000000000000000000, 1.000000000000000000 ),
 ( 0.000000000000000000, 1.000000000000000000 ),
 .UNSPECIFIED. ) 
 GEOMETRIC_REPRESENTATION_ITEM ( )  RATIONAL_B_SPLINE_SURFACE ( (
 ( 1.000000000000000000, 1.000000000000000000),
 ( 0.7789835883360578528, 0.9689951854195403280),
 ( 0.7789835883360578528, 0.9689951854195403280),
 ( 1.000000000000000000, 1.000000000000000000) ) ) 
 REPRESENTATION_ITEM ( '' )  SURFACE ( )  );
#4603 = EDGE_LOOP ( 'NONE', ( #3516, #20386, #5146, #158 ) ) ;
#4604 = LINE ( 'NONE', #26343, #15667 ) ;
#4605 = AXIS2_PLACEMENT_3D ( 'NONE', #8744, #17513, #26297 ) ;
#4606 = CARTESIAN_POINT ( 'NONE',  ( -1.619063947482201282, -44.80407745103776307, 11.94059994246206635 ) ) ;
#4607 = ORIENTED_EDGE ( 'NONE', *, *, #3162, .T. ) ;
#4608 = EDGE_CURVE ( 'NONE', #744, #27143, #85, .T. ) ;
#4609 = CARTESIAN_POINT ( 'NONE',  ( -1.619063947482197729, -25.20140673341345305, 38.92136151114934961 ) ) ;
#4610 = ORIENTED_EDGE ( 'NONE', *, *, #24001, .T. ) ;
#4611 = CARTESIAN_POINT ( 'NONE',  ( 1.833485406944057594, 141.8265699653871366, -30.69200235378795227 ) ) ;
#4612 = CARTESIAN_POINT ( 'NONE',  ( 25.64708228042122329, -45.88917180166207288, -103.1656011680036897 ) ) ;
#4613 = CARTESIAN_POINT ( 'NONE',  ( 26.11404676487257603, 84.89295829319590325, -74.91683232330889552 ) ) ;
#4614 = B_SPLINE_CURVE_WITH_KNOTS ( 'NONE', 3,
 ( #10312, #27844, #16908, #10159, #18493, #25699, #5978, #5394, #7865, #14306 ),
 .UNSPECIFIED., .F., .F.,
 ( 4, 2, 2, 2, 4 ),
 ( 7.961322465290408245E-18, 0.0003346267210630986927, 0.0006692534421261893624, 0.001003880163189280195, 0.001338506884252370919 ),
 .UNSPECIFIED. ) ;
#4615 = CARTESIAN_POINT ( 'NONE',  ( -12.94347594948481728, -21.16159467081325474, 43.91326021875537577 ) ) ;
#4616 = CARTESIAN_POINT ( 'NONE',  ( 28.37603512858449761, 104.0705994281843090, -48.29936889363852259 ) ) ;
#4617 =( BOUNDED_SURFACE ( )  B_SPLINE_SURFACE ( 3, 1, ( 
 ( #16890, #25682 ),
 ( #12409, #14577 ),
 ( #16756, #7698 ),
 ( #1335, #14709 ) ),
 .UNSPECIFIED., .F., .F., .F. ) 
 B_SPLINE_SURFACE_WITH_KNOTS ( ( 4, 4 ),
 ( 2, 2 ),
 ( 0.000000000000000000, 1.000000000000000000 ),
 ( 0.000000000000000000, 1.000000000000000000 ),
 .UNSPECIFIED. ) 
 GEOMETRIC_REPRESENTATION_ITEM ( )  RATIONAL_B_SPLINE_SURFACE ( (
 ( 1.000000000000000000, 1.000000000000000000),
 ( 0.9956975270656954757, 0.8568959468854893125),
 ( 0.9956975270656954757, 0.8568959468854893125),
 ( 1.000000000000000000, 1.000000000000000000) ) ) 
 REPRESENTATION_ITEM ( '' )  SURFACE ( )  );
#4618 = EDGE_CURVE ( 'NONE', #449, #6339, #5238, .T. ) ;
#4619 = CARTESIAN_POINT ( 'NONE',  ( 109.1778270068192853, -0.008743876326153485548, -0.003210287141656848614 ) ) ;
#4620 = FACE_OUTER_BOUND ( 'NONE', #6202, .T. ) ;
#4621 = DIRECTION ( 'NONE',  ( 1.000000000000000000, -6.938893903907226837E-18, 1.734723475976806709E-18 ) ) ;
#4622 = B_SPLINE_CURVE_WITH_KNOTS ( 'NONE', 3,
 ( #9873, #12166, #12297, #1219, #19071, #10018, #18778, #27551 ),
 .UNSPECIFIED., .F., .F.,
 ( 4, 2, 2, 4 ),
 ( 2.194186273941487942E-16, 0.002761568181852859863, 0.005523136363705500283, 0.01104627272741079066 ),
 .UNSPECIFIED. ) ;
#4623 = CARTESIAN_POINT ( 'NONE',  ( -20.38016308990358638, -24.94368798801364662, -16.25718651464972098 ) ) ;
#4624 = CARTESIAN_POINT ( 'NONE',  ( 25.64670758986456889, -65.96397693491100256, -91.63870681572889509 ) ) ;
#4625 = FACE_OUTER_BOUND ( 'NONE', #16870, .T. ) ;
#4626 = VERTEX_POINT ( 'NONE', #25369 ) ;
#4627 = ORIENTED_EDGE ( 'NONE', *, *, #5300, .T. ) ;
#4628 = CARTESIAN_POINT ( 'NONE',  ( -1.619063947482197729, -29.22875152547781852, -35.99532424477369830 ) ) ;
#4629 = CARTESIAN_POINT ( 'NONE',  ( -55.25719721206881729, 0.004044147484878754875, 0.01041086141212503938 ) ) ;
#4630 = VERTEX_POINT ( 'NONE', #5646 ) ;
#4631 = VECTOR ( 'NONE', #2772, 1000.000000000000114 ) ;
#4632 = ORIENTED_EDGE ( 'NONE', *, *, #6742, .T. ) ;
#4633 = ORIENTED_EDGE ( 'NONE', *, *, #8578, .T. ) ;
#4634 = VECTOR ( 'NONE', #20101, 1000.000000000000000 ) ;
#4635 = CARTESIAN_POINT ( 'NONE',  ( 2.063896406836609909, -138.5688025270875698, -43.61045647697833516 ) ) ;
#4636 = EDGE_CURVE ( 'NONE', #3085, #27654, #14410, .T. ) ;
#4637 = EDGE_CURVE ( 'NONE', #24758, #14951, #11428, .T. ) ;
#4638 = DIRECTION ( 'NONE',  ( 0.5946245182733607137, -0.6521823330503053739, 0.4701913299128708257 ) ) ;
#4639 = CARTESIAN_POINT ( 'NONE',  ( -1.323830074806772616, -25.17121255494502563, -38.58891736138520656 ) ) ;
#4640 = FACE_OUTER_BOUND ( 'NONE', #20196, .T. ) ;
#4641 = EDGE_CURVE ( 'NONE', #9315, #5518, #10765, .T. ) ;
#4642 = CARTESIAN_POINT ( 'NONE',  ( 25.64692232868535626, 66.63160215461263647, 91.15460455808850782 ) ) ;
#4643 = AXIS2_PLACEMENT_3D ( 'NONE', #18762, #16313, #9852 ) ;
#4644 = CARTESIAN_POINT ( 'NONE',  ( -20.57838717382308502, 28.96176188950218844, -7.715628353033780584 ) ) ;
#4645 = CIRCLE ( 'NONE', #20258, 53.53553390275978785 ) ;
#4646 = CARTESIAN_POINT ( 'NONE',  ( -2.904412668506656026, 44.35433137608966092, 17.42365698954652586 ) ) ;
#4647 = B_SPLINE_CURVE_WITH_KNOTS ( 'NONE', 3,
 ( #10479, #8592, #25874, #23739 ),
 .UNSPECIFIED., .F., .F.,
 ( 4, 4 ),
 ( 3.371304645218077370E-16, 0.01077107486149766341 ),
 .UNSPECIFIED. ) ;
#4648 = EDGE_CURVE ( 'NONE', #17203, #11340, #13582, .T. ) ;
#4649 = CARTESIAN_POINT ( 'NONE',  ( 10.93730112726006176, 142.1801301103792809, -51.37919228020152929 ) ) ;
#4650 = CARTESIAN_POINT ( 'NONE',  ( 1.831572820252008738, -97.82994539998453831, 107.1759352627503148 ) ) ;
#4651 = CARTESIAN_POINT ( 'NONE',  ( -8.786685647604896232, -7.199674155858612146, 53.04920435127190359 ) ) ;
#4653 = CIRCLE ( 'NONE', #1897, 117.6351876552689504 ) ;
#4652 =( BOUNDED_SURFACE ( )  B_SPLINE_SURFACE ( 3, 1, ( 
 ( #5219, #18296 ),
 ( #3070, #9682 ),
 ( #27229, #7543 ),
 ( #16300, #25095 ) ),
 .UNSPECIFIED., .F., .F., .F. ) 
 B_SPLINE_SURFACE_WITH_KNOTS ( ( 4, 4 ),
 ( 2, 2 ),
 ( 0.000000000000000000, 1.000000000000000000 ),
 ( 0.000000000000000000, 1.000000000000000000 ),
 .UNSPECIFIED. ) 
 GEOMETRIC_REPRESENTATION_ITEM ( )  RATIONAL_B_SPLINE_SURFACE ( (
 ( 1.000000000000000000, 1.000000000000000000),
 ( 0.9956975270656954757, 0.8568959468854893125),
 ( 0.9956975270656954757, 0.8568959468854893125),
 ( 1.000000000000000000, 1.000000000000000000) ) ) 
 REPRESENTATION_ITEM ( '' )  SURFACE ( )  );
#4654 = ORIENTED_EDGE ( 'NONE', *, *, #18793, .T. ) ;
#4656 = CARTESIAN_POINT ( 'NONE',  ( 109.1592201516379674, 0.006174480289200316024, 0.004867031887010233454 ) ) ;
#4655 = FACE_OUTER_BOUND ( 'NONE', #18444, .T. ) ;
#4657 = CARTESIAN_POINT ( 'NONE',  ( -1.058197053496162887, 36.00048521498994347, 28.32422455455037991 ) ) ;
#4658 = DIRECTION ( 'NONE',  ( -1.000000000000000000, 6.938893903907226837E-18, -1.734723475976806709E-18 ) ) ;
#4659 = CARTESIAN_POINT ( 'NONE',  ( -55.24271866751342941, 0.009388511352200529583, -0.001425019990779194824 ) ) ;
#4660 = CARTESIAN_POINT ( 'NONE',  ( 21.16825799904900052, -127.3716170292826746, 46.02882515936445174 ) ) ;
#4661 = ORIENTED_EDGE ( 'NONE', *, *, #20627, .T. ) ;
#4662 = CARTESIAN_POINT ( 'NONE',  ( -55.24390624410018802, -0.004896917417131185259, 0.009209468562452437224 ) ) ;
#4663 = VERTEX_POINT ( 'NONE', #5489 ) ;
#4664 = CARTESIAN_POINT ( 'NONE',  ( -1.049819825607605672, 43.39756533277881800, -14.63675055554395321 ) ) ;
#4665 = CARTESIAN_POINT ( 'NONE',  ( 1.893872463202059153, 141.7768406633803693, 31.10971550360632421 ) ) ;
#4666 = VERTEX_POINT ( 'NONE', #23076 ) ;
#4667 = ORIENTED_EDGE ( 'NONE', *, *, #19230, .T. ) ;
#4668 = CARTESIAN_POINT ( 'NONE',  ( -1.155001620486246550, -16.13799328198394178, 42.97366440495927975 ) ) ;
#4669 = VERTEX_POINT ( 'NONE', #3335 ) ;
#4670 = ORIENTED_EDGE ( 'NONE', *, *, #11184, .F. ) ;
#4671 = B_SPLINE_CURVE_WITH_KNOTS ( 'NONE', 3,
 ( #6843, #6992, #24704, #2502, #4950, #24557, #18043, #13440, #26827, #4819 ),
 .UNSPECIFIED., .F., .F.,
 ( 4, 3, 3, 4 ),
 ( 1.962615573354718958E-17, 0.0002669559177086215868, 0.0005339118354150813829, 0.001067817517169175959 ),
 .UNSPECIFIED. ) ;
#4672 = B_SPLINE_CURVE_WITH_KNOTS ( 'NONE', 3,
 ( #9072, #15830, #5316, #16107 ),
 .UNSPECIFIED., .F., .F.,
 ( 4, 4 ),
 ( 2.133075126106637135E-16, 0.008383748772659693066 ),
 .UNSPECIFIED. ) ;
#4673 = CONICAL_SURFACE ( 'NONE', #18457, 28.92774122539760384, 0.7853981625000054922 ) ;
#4674 = CARTESIAN_POINT ( 'NONE',  ( 26.11404676487259024, 67.46175819463365997, 90.92995828888226129 ) ) ;
#4675 = VECTOR ( 'NONE', #25742, 1000.000000000000114 ) ;
#4676 = EDGE_CURVE ( 'NONE', #15665, #11364, #22049, .T. ) ;
#4677 = CARTESIAN_POINT ( 'NONE',  ( -10.86508079875779842, -24.22249093393332231, -45.04061326950863275 ) ) ;
#4678 = CARTESIAN_POINT ( 'NONE',  ( 1.833485406944043827, 137.8414413349085521, 45.34878176254281357 ) ) ;
#4679 = CARTESIAN_POINT ( 'NONE',  ( -20.20700224038492010, 27.82980252387833886, 10.08426345511560207 ) ) ;
#4680 = ADVANCED_FACE ( 'NONE', ( #13722 ), #23564, .F. ) ;
#4681 = B_SPLINE_CURVE_WITH_KNOTS ( 'NONE', 3,
 ( #24501, #4770, #24655, #18429, #13676, #7363, #3048, #14243, #9966, #18587 ),
 .UNSPECIFIED., .F., .F.,
 ( 4, 3, 3, 4 ),
 ( 4.443059973708341306E-17, 0.0002669559177086373619, 0.0005339118354151127163, 0.001067817517169160346 ),
 .UNSPECIFIED. ) ;
#4682 = CARTESIAN_POINT ( 'NONE',  ( 1.833809397773874750, -72.40070666294502644, -125.7576368866150887 ) ) ;
#4683 = DIRECTION ( 'NONE',  ( -1.000000000000000000, -0.000000000000000000, -0.000000000000000000 ) ) ;
#4684 = ADVANCED_FACE ( 'NONE', ( #19025 ), #21172, .F. ) ;
#4685 = CARTESIAN_POINT ( 'NONE',  ( 25.86096068574578410, -110.3716997142157084, -24.48003142199199544 ) ) ;
#4687 = CARTESIAN_POINT ( 'NONE',  ( -1.048996300304493978, 26.29666317565303046, -37.49570739463894142 ) ) ;
#4686 = CARTESIAN_POINT ( 'NONE',  ( -55.24728320129491266, 0.008013189884950885564, -0.01214321324516771938 ) ) ;
#4688 = CARTESIAN_POINT ( 'NONE',  ( 32.73300124599738581, -44.31599526637883457, -108.9684813982493097 ) ) ;
#4689 = ORIENTED_EDGE ( 'NONE', *, *, #24151, .T. ) ;
#4690 = CARTESIAN_POINT ( 'NONE',  ( 32.73300124599739291, 81.52272205837319063, -84.80615050150287004 ) ) ;
#4691 = LINE ( 'NONE', #6718, #10705 ) ;
#4692 = CARTESIAN_POINT ( 'NONE',  ( -23.79248802219729697, -22.01156985585185311, -24.83956736572401525 ) ) ;
#4693 = B_SPLINE_CURVE_WITH_KNOTS ( 'NONE', 3,
 ( #11711, #24962, #7839, #27086, #10134, #9692, #5225, #13998 ),
 .UNSPECIFIED., .F., .F.,
 ( 4, 2, 2, 4 ),
 ( 3.469446951953614189E-18, 0.0002429592666046825878, 0.0004859185332093617061, 0.0009718370664187031376 ),
 .UNSPECIFIED. ) ;
#4694 = CARTESIAN_POINT ( 'NONE',  ( -1.583189561560252701, 43.29471907393764951, 16.68617981233657943 ) ) ;
#4695 = ORIENTED_EDGE ( 'NONE', *, *, #26959, .F. ) ;
#4696 = CARTESIAN_POINT ( 'NONE',  ( -1.619063947482201282, 16.67502769180561728, -43.26576862488438735 ) ) ;
#4697 = CONICAL_SURFACE ( 'NONE', #7466, 117.6351876552689504, 0.9945805576725580410 ) ;
#4698 = CARTESIAN_POINT ( 'NONE',  ( -21.81686047589424859, -38.17230180719262478, -5.181745222995322919 ) ) ;
#4699 = DIRECTION ( 'NONE',  ( 0.5914120900931444380, -0.5455001977188131956, 0.5938529060132602400 ) ) ;
#4700 = LINE ( 'NONE', #4978, #24308 ) ;
#4701 = ORIENTED_EDGE ( 'NONE', *, *, #23071, .F. ) ;
#4702 = CARTESIAN_POINT ( 'NONE',  ( 1.834118845439484335, -137.9527673765108489, 45.01070051384546389 ) ) ;
#4703 =( BOUNDED_SURFACE ( )  B_SPLINE_SURFACE ( 3, 1, ( 
 ( #6120, #14726 ),
 ( #19196, #23820 ),
 ( #5830, #12708 ),
 ( #14448, #21060 ) ),
 .UNSPECIFIED., .F., .F., .F. ) 
 B_SPLINE_SURFACE_WITH_KNOTS ( ( 4, 4 ),
 ( 2, 2 ),
 ( 0.000000000000000000, 1.000000000000000000 ),
 ( 0.000000000000000000, 1.000000000000000000 ),
 .UNSPECIFIED. ) 
 GEOMETRIC_REPRESENTATION_ITEM ( )  RATIONAL_B_SPLINE_SURFACE ( (
 ( 1.000000000000000000, 1.000000000000000000),
 ( 0.9960225298536222738, 0.9999952330161893110),
 ( 0.9960225298536222738, 0.9999952330161893110),
 ( 1.000000000000000000, 1.000000000000000000) ) ) 
 REPRESENTATION_ITEM ( '' )  SURFACE ( )  );
#4704 = LINE ( 'NONE', #4416, #7394 ) ;
#4705 = ORIENTED_EDGE ( 'NONE', *, *, #19676, .T. ) ;
#4706 = CARTESIAN_POINT ( 'NONE',  ( 25.64681081121879203, -112.9102952884414464, -0.4157506337739698132 ) ) ;
#4707 = CARTESIAN_POINT ( 'NONE',  ( 10.93730112725932635, 0.000000000000000000, 0.000000000000000000 ) ) ;
#4708 = ADVANCED_FACE ( 'NONE', ( #17405 ), #15253, .T. ) ;
#4709 = EDGE_LOOP ( 'NONE', ( #12241, #28457, #10627, #17138 ) ) ;
#4710 = AXIS2_PLACEMENT_3D ( 'NONE', #2622, #21921, #11405 ) ;
#4711 = CARTESIAN_POINT ( 'NONE',  ( -4.473127245936431073, 12.17046501147583548, 47.80062405537787384 ) ) ;
#4712 = CONICAL_SURFACE ( 'NONE', #14348, 34.60786435723138510, 0.8559913436420825139 ) ;
#4713 = EDGE_CURVE ( 'NONE', #16334, #25087, #10411, .T. ) ;
#4714 = CARTESIAN_POINT ( 'NONE',  ( 10.93730112725983439, -148.8212007290663621, 26.59437931460704263 ) ) ;
#4715 = CARTESIAN_POINT ( 'NONE',  ( -1.045287976400365970, -37.92705037016778391, -25.66401692419976399 ) ) ;
#4716 = CARTESIAN_POINT ( 'NONE',  ( -18.41936578851709072, 7.566034416291376630, 41.75701384111728487 ) ) ;
#4717 = CARTESIAN_POINT ( 'NONE',  ( 1.834118845439484335, -58.85894970555005301, 132.6369225636072144 ) ) ;
#4718 = ORIENTED_EDGE ( 'NONE', *, *, #16727, .F. ) ;
#4719 = CARTESIAN_POINT ( 'NONE',  ( -9.156249394959713683, -48.32878616081028866, -25.18996226954597972 ) ) ;
#4720 = CARTESIAN_POINT ( 'NONE',  ( 10.93730112725932990, 151.0983828010088530, 4.928439153520527860 ) ) ;
#4721 = CARTESIAN_POINT ( 'NONE',  ( -12.94347594948480484, 43.91326021875542551, 21.16159467081307710 ) ) ;
#4722 = ORIENTED_EDGE ( 'NONE', *, *, #20997, .F. ) ;
#4723 = ORIENTED_EDGE ( 'NONE', *, *, #22907, .T. ) ;
#4725 = ORIENTED_EDGE ( 'NONE', *, *, #27288, .F. ) ;
#4724 = B_SPLINE_CURVE_WITH_KNOTS ( 'NONE', 3,
 ( #16654, #25857, #12187, #20956, #14623, #23425, #27998 ),
 .UNSPECIFIED., .F., .F.,
 ( 4, 3, 4 ),
 ( 0.000000000000000000, 0.006568092053401801411, 0.02506242213020845253 ),
 .UNSPECIFIED. ) ;
#4726 = CARTESIAN_POINT ( 'NONE',  ( -1.048171036023499925, -43.86077206077059998, 13.17819047681649103 ) ) ;
#4727 = CARTESIAN_POINT ( 'NONE',  ( 2.263178113027026761, -43.59477710889630231, -138.7064940342182808 ) ) ;
#4728 = CARTESIAN_POINT ( 'NONE',  ( -4.473127245936434626, -18.25038884639903003, -45.82513704981538183 ) ) ;
#4729 = CARTESIAN_POINT ( 'NONE',  ( -25.21435515916043713, -15.02493970636168896, -31.17620025257581062 ) ) ;
#4730 = DIRECTION ( 'NONE',  ( -0.7563875759206388771, 0.5490129373055280260, 0.3556158456312881189 ) ) ;
#4731 = CARTESIAN_POINT ( 'NONE',  ( 10.93730112725978287, -125.1380233598484182, 84.82621002473399585 ) ) ;
#4732 = ORIENTED_EDGE ( 'NONE', *, *, #26697, .T. ) ;
#4733 = CARTESIAN_POINT ( 'NONE',  ( 26.11404676487257603, 1.130420376097130086, 113.2169081140374090 ) ) ;
#4734 = FACE_OUTER_BOUND ( 'NONE', #3251, .T. ) ;
#4735 = CARTESIAN_POINT ( 'NONE',  ( 2.430230287190589422, 145.5073573687466819, -1.451610819318246648 ) ) ;
#4736 = CARTESIAN_POINT ( 'NONE',  ( 13.36082413113061307, 106.9547846563650637, -109.3026516754221547 ) ) ;
#4737 = CARTESIAN_POINT ( 'NONE',  ( 2.108985857320907265, 142.3791757917253165, 28.95357181520875045 ) ) ;
#4738 = ORIENTED_EDGE ( 'NONE', *, *, #22167, .T. ) ;
#4739 = CARTESIAN_POINT ( 'NONE',  ( 109.1586900883932856, -0.004701023939953894587, -0.005371970278523948913 ) ) ;
#4741 =( BOUNDED_SURFACE ( )  B_SPLINE_SURFACE ( 3, 1, ( 
 ( #9927, #23451 ),
 ( #5753, #16532 ),
 ( #3150, #3713 ),
 ( #27319, #12350 ) ),
 .UNSPECIFIED., .F., .F., .F. ) 
 B_SPLINE_SURFACE_WITH_KNOTS ( ( 4, 4 ),
 ( 2, 2 ),
 ( 0.000000000000000000, 1.000000000000000000 ),
 ( 0.000000000000000000, 1.000000000000000000 ),
 .UNSPECIFIED. ) 
 GEOMETRIC_REPRESENTATION_ITEM ( )  RATIONAL_B_SPLINE_SURFACE ( (
 ( 1.000000000000000000, 1.000000000000000000),
 ( 0.6386103224230316178, 0.9954351624131538845),
 ( 0.6386103224230316178, 0.9954351624131538845),
 ( 1.000000000000000000, 1.000000000000000000) ) ) 
 REPRESENTATION_ITEM ( '' )  SURFACE ( )  );
#4740 = AXIS2_PLACEMENT_3D ( 'NONE', #15340, #2233, #12902 ) ;
#4742 = CARTESIAN_POINT ( 'NONE',  ( -20.24419206586952669, 18.44224248888906814, 23.20105925399704461 ) ) ;
#4743 = CARTESIAN_POINT ( 'NONE',  ( 25.64681081121879203, -56.81519825470687834, -97.57530875170664331 ) ) ;
#4744 = ORIENTED_EDGE ( 'NONE', *, *, #261, .T. ) ;
#4745 = EDGE_CURVE ( 'NONE', #27833, #18502, #8103, .T. ) ;
#4746 = EDGE_LOOP ( 'NONE', ( #11477, #6519, #21372, #20747 ) ) ;
#4747 = EDGE_CURVE ( 'NONE', #19015, #21184, #26058, .T. ) ;
#4748 = EDGE_CURVE ( 'NONE', #15804, #13619, #12963, .T. ) ;
#4749 = CARTESIAN_POINT ( 'NONE',  ( -20.21097721650786383, 28.05863614620939472, -9.464413208035171721 ) ) ;
#4750 = CARTESIAN_POINT ( 'NONE',  ( 25.64692872815574631, -23.16082795281176843, -110.5102270591925588 ) ) ;
#4751 = EDGE_CURVE ( 'NONE', #15303, #12261, #27735, .T. ) ;
#4752 = CIRCLE ( 'NONE', #13951, 34.60786435723138510 ) ;
#4753 = CARTESIAN_POINT ( 'NONE',  ( 25.87036335909428075, 57.38512068813009392, 97.41424496619539752 ) ) ;
#4754 = CARTESIAN_POINT ( 'NONE',  ( -20.57838717382308147, 25.16001208503129760, 16.28767523336092893 ) ) ;
#4755 = ORIENTED_EDGE ( 'NONE', *, *, #24190, .T. ) ;
#4756 = CARTESIAN_POINT ( 'NONE',  ( -20.37983603106074426, -24.94323704205426040, 16.25728007463434110 ) ) ;
#4757 = CONICAL_SURFACE ( 'NONE', #14403, 34.60786435723138510, 0.8559913436420825139 ) ;
#4758 = CARTESIAN_POINT ( 'NONE',  ( 1.893872463202035616, -142.1730500379302100, 29.24569695044196749 ) ) ;
#4759 = ORIENTED_EDGE ( 'NONE', *, *, #14124, .F. ) ;
#4760 = CARTESIAN_POINT ( 'NONE',  ( 30.59141879584324997, 107.2355637993510413, -44.78722686469095038 ) ) ;
#4761 = ORIENTED_EDGE ( 'NONE', *, *, #17089, .T. ) ;
#4762 = LINE ( 'NONE', #13239, #25853 ) ;
#4763 = CARTESIAN_POINT ( 'NONE',  ( -1.155031165708874985, 42.97366960678603931, -16.13806347973012834 ) ) ;
#4764 = CARTESIAN_POINT ( 'NONE',  ( 1.833485406944043827, -145.1085452359073145, -0.5339064996899981486 ) ) ;
#4765 = LINE ( 'NONE', #18422, #16109 ) ;
#4766 = B_SPLINE_CURVE_WITH_KNOTS ( 'NONE', 3,
 ( #17593, #26376, #13561, #6680, #2625, #4644 ),
 .UNSPECIFIED., .F., .F.,
 ( 4, 2, 4 ),
 ( 1.072867218403649326E-17, 0.003576372551510812684, 0.007152745103021620164 ),
 .UNSPECIFIED. ) ;
#4767 = CARTESIAN_POINT ( 'NONE',  ( -1.044556982611271279, -12.57890920527746381, 44.03203163107538387 ) ) ;
#4768 = DIRECTION ( 'NONE',  ( -0.5946245182733607137, 0.7637359336799438569, -0.2512550613902095331 ) ) ;
#4769 = FACE_OUTER_BOUND ( 'NONE', #10038, .T. ) ;
#4770 = CARTESIAN_POINT ( 'NONE',  ( 1.833603222531971833, 58.61467103263744605, 132.7445893798459906 ) ) ;
#4771 = CARTESIAN_POINT ( 'NONE',  ( -25.21435515916025594, 1.749597353048488237E-16, -4.373993382621220594E-17 ) ) ;
#4772 = CARTESIAN_POINT ( 'NONE',  ( -20.47566338032522992, -25.06314818626703200, -16.24827550219816885 ) ) ;
#4773 = CARTESIAN_POINT ( 'NONE',  ( -1.539763995773683503, 44.72359274866481371, -11.93465967526309868 ) ) ;
#4774 = CARTESIAN_POINT ( 'NONE',  ( -25.21435515916043002, -4.655591116594591128, -34.29329011225954105 ) ) ;
#4775 = CARTESIAN_POINT ( 'NONE',  ( -1.056502255334265339, 43.40574022158794065, 14.64009593116057317 ) ) ;
#4776 = ORIENTED_EDGE ( 'NONE', *, *, #28032, .T. ) ;
#4777 = EDGE_CURVE ( 'NONE', #15104, #5027, #22651, .T. ) ;
#4778 = ORIENTED_EDGE ( 'NONE', *, *, #22391, .F. ) ;
#4779 = CARTESIAN_POINT ( 'NONE',  ( 26.04756280548352976, 24.61655718144339389, 110.4687147111160357 ) ) ;
#4780 = FACE_OUTER_BOUND ( 'NONE', #14497, .T. ) ;
#4781 = ORIENTED_EDGE ( 'NONE', *, *, #10805, .F. ) ;
#4782 = VERTEX_POINT ( 'NONE', #1867 ) ;
#4783 = EDGE_CURVE ( 'NONE', #9740, #10557, #13290, .T. ) ;
#4784 = VERTEX_POINT ( 'NONE', #3610 ) ;
#4785 = CARTESIAN_POINT ( 'NONE',  ( 109.1586900883932856, 0.005236795036868161120, 0.004851151255031871216 ) ) ;
#4786 = CARTESIAN_POINT ( 'NONE',  ( 109.1721716018069657, -0.01699510305644696614, -0.001583175916619995001 ) ) ;
#4787 = EDGE_CURVE ( 'NONE', #15548, #2734, #14968, .T. ) ;
#4788 = B_SPLINE_CURVE_WITH_KNOTS ( 'NONE', 3,
 ( #17381, #10787, #10919, #19411, #21716, #6326, #1987, #4293 ),
 .UNSPECIFIED., .F., .F.,
 ( 4, 2, 2, 4 ),
 ( 2.251264292202123005E-16, 0.002761568181852863766, 0.005523136363705502885, 0.01104627272741079413 ),
 .UNSPECIFIED. ) ;
#4789 = CARTESIAN_POINT ( 'NONE',  ( 109.1586900883932856, -0.006757191295056145380, 0.002301750759607874407 ) ) ;
#4790 = VERTEX_POINT ( 'NONE', #10265 ) ;
#4791 = CARTESIAN_POINT ( 'NONE',  ( -20.20700224038492721, 29.58392382092673500, 0.9908225410479544193 ) ) ;
#4792 =( BOUNDED_SURFACE ( )  B_SPLINE_SURFACE ( 3, 1, ( 
 ( #4941, #2638 ),
 ( #13573, #16308 ),
 ( #13714, #14135 ),
 ( #6980, #22957 ) ),
 .UNSPECIFIED., .F., .F., .F. ) 
 B_SPLINE_SURFACE_WITH_KNOTS ( ( 4, 4 ),
 ( 2, 2 ),
 ( 0.000000000000000000, 1.000000000000000000 ),
 ( 0.000000000000000000, 1.000000000000000000 ),
 .UNSPECIFIED. ) 
 GEOMETRIC_REPRESENTATION_ITEM ( )  RATIONAL_B_SPLINE_SURFACE ( (
 ( 1.000000000000000000, 1.000000000000000000),
 ( 0.9956975270656954757, 0.8568959468854893125),
 ( 0.9956975270656954757, 0.8568959468854893125),
 ( 1.000000000000000000, 1.000000000000000000) ) ) 
 REPRESENTATION_ITEM ( '' )  SURFACE ( )  );
#4793 = CARTESIAN_POINT ( 'NONE',  ( -1.019300379054419725, 38.21680004809200426, 25.26451264419602438 ) ) ;
#4794 = CARTESIAN_POINT ( 'NONE',  ( 109.1586900883932856, -0.004851151255031892033, 0.005236795036868142038 ) ) ;
#4795 = DIRECTION ( 'NONE',  ( 0.000000000000000000, 0.000000000000000000, 1.000000000000000000 ) ) ;
#4797 = B_SPLINE_CURVE_WITH_KNOTS ( 'NONE', 3,
 ( #3366, #3217, #9999, #12284, #25400, #16764 ),
 .UNSPECIFIED., .F., .F.,
 ( 4, 2, 4 ),
 ( 4.906538933386797396E-18, 0.0004335151646191504906, 0.0008670303292382959938 ),
 .UNSPECIFIED. ) ;
#4796 = CARTESIAN_POINT ( 'NONE',  ( 5.340103579038074422, 140.9275371836310455, 43.36842539899422633 ) ) ;
#4798 = CARTESIAN_POINT ( 'NONE',  ( 2.063896406836609909, -118.3103904147675962, -84.29612368209275530 ) ) ;
#4799 = CARTESIAN_POINT ( 'NONE',  ( 26.04756280548354397, -65.62256188141788016, 92.21166514879074327 ) ) ;
#4800 = CARTESIAN_POINT ( 'NONE',  ( 6.224689322667630975, -126.9212313063839588, -76.23997225729401350 ) ) ;
#4801 = CARTESIAN_POINT ( 'NONE',  ( -1.019300379054419947, 25.26451264419699783, 38.21680004809136477 ) ) ;
#4802 = VERTEX_POINT ( 'NONE', #5934 ) ;
#4804 = CARTESIAN_POINT ( 'NONE',  ( 25.64699802086725811, -66.55977212001099019, -91.20712948285722632 ) ) ;
#4803 = CARTESIAN_POINT ( 'NONE',  ( 109.1586900883932856, -0.004277182003220990347, 0.005715190711488705826 ) ) ;
#4805 = CARTESIAN_POINT ( 'NONE',  ( 109.1624594426973260, -0.003771499231549682845, 0.01551217196236918082 ) ) ;
#4806 = CARTESIAN_POINT ( 'NONE',  ( -1.045287976400365970, -36.12803364096568259, 28.14015102489869591 ) ) ;
#4807 = CARTESIAN_POINT ( 'NONE',  ( 10.93730112725978287, -136.0306644680987915, 65.95960219663069779 ) ) ;
#4808 = CARTESIAN_POINT ( 'NONE',  ( -7.711401346138395674, -35.51061203065555816, -38.61705198405353912 ) ) ;
#4809 = ORIENTED_EDGE ( 'NONE', *, *, #1046, .T. ) ;
#4810 = CARTESIAN_POINT ( 'NONE',  ( 1.833721034905646752, -15.52204855105742176, -144.2772269874177198 ) ) ;
#4811 = EDGE_CURVE ( 'NONE', #14553, #12735, #19814, .T. ) ;
#4812 = VERTEX_POINT ( 'NONE', #9066 ) ;
#4813 = CARTESIAN_POINT ( 'NONE',  ( 1.833485406944043827, 117.7091014914961420, -84.86072343962446496 ) ) ;
#4814 = CARTESIAN_POINT ( 'NONE',  ( -20.47566338032530098, -23.19796701701852015, 18.81547714195498244 ) ) ;
#4815 = ORIENTED_EDGE ( 'NONE', *, *, #6490, .F. ) ;
#4816 = EDGE_CURVE ( 'NONE', #1490, #7808, #8168, .T. ) ;
#4817 = CARTESIAN_POINT ( 'NONE',  ( 13.84597867724963294, 129.3717503931862325, -69.17016226638924081 ) ) ;
#4818 = ORIENTED_EDGE ( 'NONE', *, *, #23496, .F. ) ;
#4819 = CARTESIAN_POINT ( 'NONE',  ( 1.833485406944043827, -97.49333871408619245, -107.4794113447419477 ) ) ;
#4820 = ORIENTED_EDGE ( 'NONE', *, *, #4568, .F. ) ;
#4821 = ADVANCED_FACE ( 'NONE', ( #26470 ), #26302, .F. ) ;
#4822 = CARTESIAN_POINT ( 'NONE',  ( 1.893872463202060485, -125.2243573918629096, -73.39855082356775995 ) ) ;
#4823 = ADVANCED_FACE ( 'NONE', ( #6491 ), #20596, .F. ) ;
#4824 = LINE ( 'NONE', #14935, #957 ) ;
#4825 = CARTESIAN_POINT ( 'NONE',  ( 1.893872463202018963, 137.7483215415849713, 45.75900850850049295 ) ) ;
#4826 =( BOUNDED_SURFACE ( )  B_SPLINE_SURFACE ( 3, 1, ( 
 ( #6940, #26492 ),
 ( #2455, #11246 ),
 ( #6509, #444 ),
 ( #22036, #300 ) ),
 .UNSPECIFIED., .F., .F., .F. ) 
 B_SPLINE_SURFACE_WITH_KNOTS ( ( 4, 4 ),
 ( 2, 2 ),
 ( 0.000000000000000000, 1.000000000000000000 ),
 ( 0.000000000000000000, 1.000000000000000000 ),
 .UNSPECIFIED. ) 
 GEOMETRIC_REPRESENTATION_ITEM ( )  RATIONAL_B_SPLINE_SURFACE ( (
 ( 1.000000000000000000, 1.000000000000000000),
 ( 0.7789835883360576307, 0.9689951854195403280),
 ( 0.7789835883360576307, 0.9689951854195403280),
 ( 1.000000000000000000, 1.000000000000000000) ) ) 
 REPRESENTATION_ITEM ( '' )  SURFACE ( )  );
#4827 = CARTESIAN_POINT ( 'NONE',  ( -8.786685647604885574, 6.069026232697080105E-17, 53.53553390275978785 ) ) ;
#4828 = CARTESIAN_POINT ( 'NONE',  ( -55.24300891470648622, 0.0003472257464250210184, -0.009812809446890590967 ) ) ;
#4829 = CARTESIAN_POINT ( 'NONE',  ( -23.79223135445720771, 22.01133905265687929, -24.83942264280410228 ) ) ;
#4830 = CARTESIAN_POINT ( 'NONE',  ( -1.048172774974286847, 26.08722459372787128, -37.64158596421222569 ) ) ;
#4831 = FACE_OUTER_BOUND ( 'NONE', #8783, .T. ) ;
#4832 = ORIENTED_EDGE ( 'NONE', *, *, #23459, .T. ) ;
#4833 = CARTESIAN_POINT ( 'NONE',  ( -4.162674018437136247, 11.82104147411627970, 47.46216648493545165 ) ) ;
#4835 = CARTESIAN_POINT ( 'NONE',  ( -8.259864102781676820, 22.52209142945002895, 47.98931516265572128 ) ) ;
#4834 = CARTESIAN_POINT ( 'NONE',  ( -55.24390624410018802, 0.001451500391953283731, -0.01032895241566680888 ) ) ;
#4836 = CARTESIAN_POINT ( 'NONE',  ( 26.11404676487256893, -110.9778746459748362, 22.43340081644731043 ) ) ;
#4837 = CARTESIAN_POINT ( 'NONE',  ( -8.786685647604890903, 23.24040270374391426, -48.22796981442777309 ) ) ;
#4838 = VERTEX_POINT ( 'NONE', #17823 ) ;
#4839 = CARTESIAN_POINT ( 'NONE',  ( 1.833721034905662295, 45.17977675814314864, 137.8972080590633027 ) ) ;
#4840 = CARTESIAN_POINT ( 'NONE',  ( 24.01988960052062794, -49.36855864442049580, -121.3896480498355714 ) ) ;
#4841 = CARTESIAN_POINT ( 'NONE',  ( 55.79472521941426777, 49.22042574086499656, -53.57698701322163970 ) ) ;
#4842 = ORIENTED_EDGE ( 'NONE', *, *, #24981, .T. ) ;
#4843 = CARTESIAN_POINT ( 'NONE',  ( 25.64704443564078673, 75.65149037849873537, -83.82001435192547945 ) ) ;
#4844 = EDGE_CURVE ( 'NONE', #18428, #11607, #2644, .T. ) ;
#4845 = ORIENTED_EDGE ( 'NONE', *, *, #28444, .F. ) ;
#4846 = CARTESIAN_POINT ( 'NONE',  ( 119.2224693531408803, -6.245004513516543405E-14, 20.00000000000018119 ) ) ;
#4847 = EDGE_CURVE ( 'NONE', #12354, #4901, #17068, .T. ) ;
#4848 = CARTESIAN_POINT ( 'NONE',  ( -20.38016308990358638, -28.74660391518349911, -7.753479680700832155 ) ) ;
#4849 = DIRECTION ( 'NONE',  ( -1.000000000000000000, -0.000000000000000000, -0.000000000000000000 ) ) ;
#4850 = ORIENTED_EDGE ( 'NONE', *, *, #4751, .F. ) ;
#4851 = CARTESIAN_POINT ( 'NONE',  ( 25.81918753295377655, 112.3053965977763511, -12.74259626488037256 ) ) ;
#4852 = ORIENTED_EDGE ( 'NONE', *, *, #10092, .F. ) ;
#4853 = ORIENTED_EDGE ( 'NONE', *, *, #13308, .F. ) ;
#4854 = B_SPLINE_CURVE_WITH_KNOTS ( 'NONE', 3,
 ( #24903, #5162, #13938, #27468, #12083, #7637 ),
 .UNSPECIFIED., .F., .F.,
 ( 4, 2, 4 ),
 ( 1.072867218403649326E-17, 0.003576372551510812684, 0.007152745103021620164 ),
 .UNSPECIFIED. ) ;
#4855 = DIRECTION ( 'NONE',  ( 0.000000000000000000, 5.223019709708233256E-21, -1.000000000000000000 ) ) ;
#4856 = CARTESIAN_POINT ( 'NONE',  ( 30.59138290137870442, 111.3296280985502165, 33.33271994911384439 ) ) ;
#4857 = CARTESIAN_POINT ( 'NONE',  ( -21.81686047589426991, -34.70276904128901663, -16.72402253294301744 ) ) ;
#4858 = CARTESIAN_POINT ( 'NONE',  ( -55.24271866751342941, 0.008488649505346581442, -0.004256484107793381474 ) ) ;
#4859 = FACE_OUTER_BOUND ( 'NONE', #22923, .T. ) ;
#4860 = ORIENTED_EDGE ( 'NONE', *, *, #24344, .T. ) ;
#4861 = CARTESIAN_POINT ( 'NONE',  ( 13.36082413113061307, 53.25066407421994796, -143.3553710183984435 ) ) ;
#4862 = CARTESIAN_POINT ( 'NONE',  ( 2.433796855181205476, 145.5024947199069629, 1.451562450950146133 ) ) ;
#4863 = CARTESIAN_POINT ( 'NONE',  ( -20.47566338032527611, 23.19796701701867647, -18.81547714195482612 ) ) ;
#4864 = VERTEX_POINT ( 'NONE', #2724 ) ;
#4865 = ORIENTED_EDGE ( 'NONE', *, *, #189, .T. ) ;
#4866 = ORIENTED_EDGE ( 'NONE', *, *, #3434, .F. ) ;
#4867 = CARTESIAN_POINT ( 'NONE',  ( -12.82751273423879113, -21.21958768041828947, -44.03362901247000138 ) ) ;
#4868 = CARTESIAN_POINT ( 'NONE',  ( 26.11404676487259024, -47.08215554553450488, -102.9690087468806325 ) ) ;
#4869 = CARTESIAN_POINT ( 'NONE',  ( -1.046935749539996907, 1.275486069320473481, -45.77872888003166452 ) ) ;
#4870 = DIRECTION ( 'NONE',  ( 0.5946245182733608248, 0.4701913299128731016, 0.6521823330503037086 ) ) ;
#4871 = CARTESIAN_POINT ( 'NONE',  ( 10.93730112726024117, 133.3192575531818136, -71.28103789254788580 ) ) ;
#4872 =( BOUNDED_SURFACE ( )  B_SPLINE_SURFACE ( 3, 1, ( 
 ( #7825, #28080 ),
 ( #8385, #6228 ),
 ( #20898, #9983 ),
 ( #16585, #25379 ) ),
 .UNSPECIFIED., .F., .F., .F. ) 
 B_SPLINE_SURFACE_WITH_KNOTS ( ( 4, 4 ),
 ( 2, 2 ),
 ( 0.000000000000000000, 1.000000000000000000 ),
 ( 0.000000000000000000, 1.000000000000000000 ),
 .UNSPECIFIED. ) 
 GEOMETRIC_REPRESENTATION_ITEM ( )  RATIONAL_B_SPLINE_SURFACE ( (
 ( 1.000000000000000000, 1.000000000000000000),
 ( 0.6386103224230316178, 0.9954351624131538845),
 ( 0.6386103224230316178, 0.9954351624131538845),
 ( 1.000000000000000000, 1.000000000000000000) ) ) 
 REPRESENTATION_ITEM ( '' )  SURFACE ( )  );
#4873 = CARTESIAN_POINT ( 'NONE',  ( 1.832998868059858122, 72.09222286251082323, 125.9352106559986311 ) ) ;
#4874 = VERTEX_POINT ( 'NONE', #26333 ) ;
#4875 = CARTESIAN_POINT ( 'NONE',  ( -8.786685647604885574, 6.096987947571466530E-17, -1.524246986892866633E-17 ) ) ;
#4876 = CARTESIAN_POINT ( 'NONE',  ( -4.473127245936431073, -47.80062405537792358, 12.17046501147566318 ) ) ;
#4877 = CARTESIAN_POINT ( 'NONE',  ( 1.833809397773905614, -145.1096615951801141, -0.1779672212515608920 ) ) ;
#4878 = CARTESIAN_POINT ( 'NONE',  ( 25.86096068574581963, 102.8701285401541696, 46.89265070732157881 ) ) ;
#4879 = EDGE_CURVE ( 'NONE', #7066, #2795, #13960, .T. ) ;
#4880 = ORIENTED_EDGE ( 'NONE', *, *, #5427, .F. ) ;
#4881 = FACE_OUTER_BOUND ( 'NONE', #8965, .T. ) ;
#4882 = VERTEX_POINT ( 'NONE', #11497 ) ;
#4883 = DIRECTION ( 'NONE',  ( 0.000000000000000000, 0.000000000000000000, 1.000000000000000000 ) ) ;
#4884 = B_SPLINE_CURVE_WITH_KNOTS ( 'NONE', 3,
 ( #15775, #5269, #20523, #7298, #3115, #24586, #3259, #26854 ),
 .UNSPECIFIED., .F., .F.,
 ( 4, 2, 2, 4 ),
 ( 0.000000000000000000, 0.0002429588503611208340, 0.0004859177007222416681, 0.0009718354014444833362 ),
 .UNSPECIFIED. ) ;
#4885 = ADVANCED_FACE ( 'NONE', ( #21883 ), #3875, .F. ) ;
#4886 = CARTESIAN_POINT ( 'NONE',  ( 25.64700659047694842, -56.25842064176025303, -97.89757946487067386 ) ) ;
#4887 = ORIENTED_EDGE ( 'NONE', *, *, #8850, .T. ) ;
#4888 = EDGE_CURVE ( 'NONE', #5555, #26700, #9936, .T. ) ;
#4889 = ORIENTED_EDGE ( 'NONE', *, *, #4056, .F. ) ;
#4890 = ORIENTED_EDGE ( 'NONE', *, *, #7357, .T. ) ;
#4891 = DIRECTION ( 'NONE',  ( 0.000000000000000000, 0.000000000000000000, 1.000000000000000000 ) ) ;
#4892 = CARTESIAN_POINT ( 'NONE',  ( 109.1721716018069657, -0.009868622090676078262, 0.01392660302850765031 ) ) ;
#4893 = DIRECTION ( 'NONE',  ( 0.000000000000000000, 0.000000000000000000, 1.000000000000000000 ) ) ;
#4894 = CARTESIAN_POINT ( 'NONE',  ( 109.1587776205901577, 0.003592288931009604384, 0.006388631651928904608 ) ) ;
#4895 = DIRECTION ( 'NONE',  ( -5.541455922705464902E-20, 5.223019709708320524E-21, -1.000000000000000000 ) ) ;
#4896 = ORIENTED_EDGE ( 'NONE', *, *, #19775, .F. ) ;
#4897 = CARTESIAN_POINT ( 'NONE',  ( -1.583189561560256253, 29.24830400313217282, 36.01941156322756399 ) ) ;
#4898 = CARTESIAN_POINT ( 'NONE',  ( 1.832998868059858122, -15.69902610990277836, -144.2584710144581948 ) ) ;
#4899 = ADVANCED_FACE ( 'NONE', ( #708 ), #27224, .F. ) ;
#4900 = CARTESIAN_POINT ( 'NONE',  ( 1.833485406944043827, -142.0485807715647297, 29.64752363041495542 ) ) ;
#4901 = VERTEX_POINT ( 'NONE', #25055 ) ;
#4902 = CARTESIAN_POINT ( 'NONE',  ( -1.323439229708146536, -25.17120723334064891, 38.58845475799796532 ) ) ;
#4903 = VERTEX_POINT ( 'NONE', #16397 ) ;
#4904 = CARTESIAN_POINT ( 'NONE',  ( -4.473127245936434626, -37.94261489385694830, 31.51789735524234004 ) ) ;
#4905 = CARTESIAN_POINT ( 'NONE',  ( 25.64681081121879203, -46.30456157731261868, -102.9795863647033229 ) ) ;
#4906 = CARTESIAN_POINT ( 'NONE',  ( 1.832998868059890096, -144.3700883710216090, -14.63705790014157060 ) ) ;
#4907 = CARTESIAN_POINT ( 'NONE',  ( -20.47566262905010603, 27.87687924095562408, 10.72601569609867944 ) ) ;
#4908 = CARTESIAN_POINT ( 'NONE',  ( -22.23342874802667879, 31.55488258420089664, 2.180636882146622657 ) ) ;
#4909 = ADVANCED_FACE ( 'NONE', ( #18250 ), #17145, .T. ) ;
#4910 = CARTESIAN_POINT ( 'NONE',  ( -1.463510566862827655, 44.64091840826493041, -11.94877850058517765 ) ) ;
#4911 = CYLINDRICAL_SURFACE ( 'NONE', #10220, 12.50000000000000178 ) ;
#4912 =( BOUNDED_SURFACE ( )  B_SPLINE_SURFACE ( 3, 1, ( 
 ( #6920, #13230 ),
 ( #6636, #15524 ),
 ( #24483, #2435 ),
 ( #9071, #24200 ) ),
 .UNSPECIFIED., .F., .F., .F. ) 
 B_SPLINE_SURFACE_WITH_KNOTS ( ( 4, 4 ),
 ( 2, 2 ),
 ( 0.000000000000000000, 1.000000000000000000 ),
 ( 0.000000000000000000, 1.000000000000000000 ),
 .UNSPECIFIED. ) 
 GEOMETRIC_REPRESENTATION_ITEM ( )  RATIONAL_B_SPLINE_SURFACE ( (
 ( 1.000000000000000000, 1.000000000000000000),
 ( 0.6386103224230302855, 0.9954351624131538845),
 ( 0.6386103224230302855, 0.9954351624131538845),
 ( 1.000000000000000000, 1.000000000000000000) ) ) 
 REPRESENTATION_ITEM ( '' )  SURFACE ( )  );
#4913 = EDGE_CURVE ( 'NONE', #27654, #8132, #22234, .T. ) ;
#4914 = CARTESIAN_POINT ( 'NONE',  ( -1.045287976400365970, 15.59869763335068171, -43.05558670614252037 ) ) ;
#4915 = CARTESIAN_POINT ( 'NONE',  ( 2.430230287190581429, 107.1617224697464366, 98.44218333480804972 ) ) ;
#4916 = LINE ( 'NONE', #22488, #6177 ) ;
#4917 = CARTESIAN_POINT ( 'NONE',  ( 25.64703792032471341, -107.3388703233124346, 35.03296646432524142 ) ) ;
#4918 = ORIENTED_EDGE ( 'NONE', *, *, #14850, .F. ) ;
#4919 = VERTEX_POINT ( 'NONE', #13945 ) ;
#4920 = CARTESIAN_POINT ( 'NONE',  ( 1.893872463202054046, -126.1771883101041851, 71.74819926215134558 ) ) ;
#4921 = CARTESIAN_POINT ( 'NONE',  ( 1.834118845439484335, -117.5010238212692855, -85.14950727125977892 ) ) ;
#4922 = ORIENTED_EDGE ( 'NONE', *, *, #14661, .F. ) ;
#4923 = VERTEX_POINT ( 'NONE', #16539 ) ;
#4924 = VERTEX_POINT ( 'NONE', #23040 ) ;
#4925 = CARTESIAN_POINT ( 'NONE',  ( 9.884929003653608603, -35.39789245780430349, 146.3148513795965755 ) ) ;
#4926 = CARTESIAN_POINT ( 'NONE',  ( -55.24390624410018802, 0.01027195578988056128, 0.001811362924362418811 ) ) ;
#4927 = CARTESIAN_POINT ( 'NONE',  ( 21.16825799904901473, 51.02216409572741895, -125.4548537968708786 ) ) ;
#4928 = CARTESIAN_POINT ( 'NONE',  ( 119.2224693531407382, -90.00000000000005684, 20.00000000000004263 ) ) ;
#4929 = CARTESIAN_POINT ( 'NONE',  ( -20.57838717382308147, -16.28767523336139078, -25.16001208503099917 ) ) ;
#4930 = FACE_OUTER_BOUND ( 'NONE', #5192, .T. ) ;
#4931 = CARTESIAN_POINT ( 'NONE',  ( -12.82751273423878047, -8.715310691359913875, 48.09651489336692975 ) ) ;
#4932 = CARTESIAN_POINT ( 'NONE',  ( 19.66333377628716406, 4.491394265034155175, -137.6761449113041920 ) ) ;
#4933 = EDGE_CURVE ( 'NONE', #16681, #4784, #3020, .T. ) ;
#4934 = CARTESIAN_POINT ( 'NONE',  ( -6.588769196390761529, -47.06982923582523171, -20.50531526814544847 ) ) ;
#4935 = CARTESIAN_POINT ( 'NONE',  ( 30.58324630866341209, 87.19147450740472038, -83.81536267638863080 ) ) ;
#4936 = ADVANCED_FACE ( 'NONE', ( #850 ), #10526, .F. ) ;
#4937 = VERTEX_POINT ( 'NONE', #3021 ) ;
#4938 = CARTESIAN_POINT ( 'NONE',  ( -28.13707043255157103, -14.07296284901319439, 18.06394523322468615 ) ) ;
#4939 = CARTESIAN_POINT ( 'NONE',  ( 26.11404676487257603, 76.59696442953305962, -83.38016054979703995 ) ) ;
#4940 = CARTESIAN_POINT ( 'NONE',  ( 1.832998868059890096, -125.4013017422225857, -73.01698022778485608 ) ) ;
#4941 = CARTESIAN_POINT ( 'NONE',  ( 109.1592201516379674, -0.007302213399779945366, 0.002913740842108614778 ) ) ;
#4942 = CARTESIAN_POINT ( 'NONE',  ( -1.323439229708132547, 16.42345129173398632, 43.04565903621268319 ) ) ;
#4943 = ORIENTED_EDGE ( 'NONE', *, *, #8331, .F. ) ;
#4944 = CARTESIAN_POINT ( 'NONE',  ( 10.93730112725991432, -71.28103789254845424, -133.3192575531807620 ) ) ;
#4945 = ORIENTED_EDGE ( 'NONE', *, *, #17473, .F. ) ;
#4946 = CARTESIAN_POINT ( 'NONE',  ( -55.24390624410018802, -0.01027195578987734684, 0.001811362924359352471 ) ) ;
#4947 = ORIENTED_EDGE ( 'NONE', *, *, #16320, .T. ) ;
#4948 = CARTESIAN_POINT ( 'NONE',  ( -12.94347594948482794, -6.555928820868979656, 48.30328466416770539 ) ) ;
#4949 = ORIENTED_EDGE ( 'NONE', *, *, #19572, .T. ) ;
#4950 = CARTESIAN_POINT ( 'NONE',  ( 1.833809397773860095, -96.96506043213376813, -107.9565774559021349 ) ) ;
#4951 = VERTEX_POINT ( 'NONE', #22605 ) ;
#4952 = B_SPLINE_CURVE_WITH_KNOTS ( 'NONE', 3,
 ( #25972, #23698, #18933, #25836, #6131, #3949, #19343, #14602, #6262, #23830 ),
 .UNSPECIFIED., .F., .F.,
 ( 4, 3, 3, 4 ),
 ( 8.944667923005411581E-18, 0.0002669560319015738814, 0.0005492286108966413453, 0.0008315040496093442472 ),
 .UNSPECIFIED. ) ;
#4953 = B_SPLINE_CURVE_WITH_KNOTS ( 'NONE', 3,
 ( #17361, #24285, #17648, #2377 ),
 .UNSPECIFIED., .F., .F.,
 ( 4, 4 ),
 ( 5.689046731696576935E-16, 0.008383748772660036541 ),
 .UNSPECIFIED. ) ;
#4954 =( BOUNDED_SURFACE ( )  B_SPLINE_SURFACE ( 3, 1, ( 
 ( #27470, #13940 ),
 ( #3018, #10364 ),
 ( #17094, #25329 ),
 ( #6042, #25620 ) ),
 .UNSPECIFIED., .F., .F., .F. ) 
 B_SPLINE_SURFACE_WITH_KNOTS ( ( 4, 4 ),
 ( 2, 2 ),
 ( 0.000000000000000000, 1.000000000000000000 ),
 ( 0.000000000000000000, 1.000000000000000000 ),
 .UNSPECIFIED. ) 
 GEOMETRIC_REPRESENTATION_ITEM ( )  RATIONAL_B_SPLINE_SURFACE ( (
 ( 1.000000000000000000, 1.000000000000000000),
 ( 0.9934239774497838349, 0.8357310067453913582),
 ( 0.9934239774497838349, 0.8357310067453913582),
 ( 1.000000000000000000, 1.000000000000000000) ) ) 
 REPRESENTATION_ITEM ( '' )  SURFACE ( )  );
#4955 = CARTESIAN_POINT ( 'NONE',  ( 26.11404676487257603, -113.2169081140373947, -1.130420376098323576 ) ) ;
#4956 = CYLINDRICAL_SURFACE ( 'NONE', #22091, 37.50000000000001421 ) ;
#4957 = CARTESIAN_POINT ( 'NONE',  ( -1.045287976400383290, -12.68782741917353185, -44.00138577190637079 ) ) ;
#4958 = ADVANCED_FACE ( 'NONE', ( #3158 ), #27569, .F. ) ;
#4959 = FACE_OUTER_BOUND ( 'NONE', #17435, .T. ) ;
#4960 = CARTESIAN_POINT ( 'NONE',  ( 25.64681081121879203, 110.3564950173084895, -23.88203588907973085 ) ) ;
#4961 = EDGE_CURVE ( 'NONE', #26564, #3869, #245, .T. ) ;
#4962 = CARTESIAN_POINT ( 'NONE',  ( 2.433796855181219243, -125.2830755159749003, -74.00833731765692391 ) ) ;
#4963 = CARTESIAN_POINT ( 'NONE',  ( 32.73300124599732186, 0.000000000000000000, 0.000000000000000000 ) ) ;
#4964 = CARTESIAN_POINT ( 'NONE',  ( 109.1586900883932856, 0.005715190711488721438, 0.004277182003220971265 ) ) ;
#4965 = EDGE_CURVE ( 'NONE', #6633, #7508, #28373, .T. ) ;
#4966 = ORIENTED_EDGE ( 'NONE', *, *, #7172, .T. ) ;
#4967 = CARTESIAN_POINT ( 'NONE',  ( -1.056502255334265339, 43.72121397317224734, -13.66916755949864637 ) ) ;
#4969 = CARTESIAN_POINT ( 'NONE',  ( -4.178947244162533714, -41.47292084251643729, -25.96944194166775333 ) ) ;
#4968 = CARTESIAN_POINT ( 'NONE',  ( 1.833485406944057594, -72.09189602597798796, 125.9346397303433065 ) ) ;
#4970 = CARTESIAN_POINT ( 'NONE',  ( 109.1586900883932856, 0.003481399864218433400, -0.006231977675085001445 ) ) ;
#4971 = CARTESIAN_POINT ( 'NONE',  ( 1.834118845439484335, -44.67218053242488196, 138.0627591860428254 ) ) ;
#4972 = CARTESIAN_POINT ( 'NONE',  ( 26.11404676487259024, -112.4785329405482912, 12.95861723607416671 ) ) ;
#4973 = ADVANCED_FACE ( 'NONE', ( #23460 ), #26472, .F. ) ;
#4974 = CARTESIAN_POINT ( 'NONE',  ( 21.16825799904934158, 135.3612955721062860, -4.416019842158871889 ) ) ;
#4975 = CARTESIAN_POINT ( 'NONE',  ( 1.833485406944043827, 45.34878176254236593, 137.8414413349087511 ) ) ;
#4976 = CARTESIAN_POINT ( 'NONE',  ( 109.1624594426973260, 0.01503296564240497526, 0.005372302061310759227 ) ) ;
#4977 = ORIENTED_EDGE ( 'NONE', *, *, #23231, .T. ) ;
#4978 = CARTESIAN_POINT ( 'NONE',  ( 55.79472521941428198, 23.17337251492763883, 68.96476385670672471 ) ) ;
#4979 = B_SPLINE_CURVE_WITH_KNOTS ( 'NONE', 3,
 ( #5323, #14096, #18714, #5183, #20723, #27485 ),
 .UNSPECIFIED., .F., .F.,
 ( 4, 2, 4 ),
 ( 3.469446951953613804E-18, 0.0006311636237756778267, 0.001262327247551352401 ),
 .UNSPECIFIED. ) ;
#4980 = ORIENTED_EDGE ( 'NONE', *, *, #26121, .T. ) ;
#4981 = AXIS2_PLACEMENT_3D ( 'NONE', #8062, #7481, #16833 ) ;
#4982 = AXIS2_PLACEMENT_3D ( 'NONE', #8847, #6544, #24393 ) ;
#4983 = ORIENTED_EDGE ( 'NONE', *, *, #18568, .F. ) ;
#4984 = CARTESIAN_POINT ( 'NONE',  ( -7.078251931573400491, -34.59014398252887190, 38.93060825814266934 ) ) ;
#4985 =( BOUNDED_SURFACE ( )  B_SPLINE_SURFACE ( 3, 1, ( 
 ( #24052, #26324 ),
 ( #8633, #6765 ),
 ( #15376, #26741 ),
 ( #28467, #6906 ) ),
 .UNSPECIFIED., .F., .F., .F. ) 
 B_SPLINE_SURFACE_WITH_KNOTS ( ( 4, 4 ),
 ( 2, 2 ),
 ( 0.000000000000000000, 1.000000000000000000 ),
 ( 0.000000000000000000, 1.000000000000000000 ),
 .UNSPECIFIED. ) 
 GEOMETRIC_REPRESENTATION_ITEM ( )  RATIONAL_B_SPLINE_SURFACE ( (
 ( 1.000000000000000000, 1.000000000000000000),
 ( 0.7789835883360576307, 0.9689951854195403280),
 ( 0.7789835883360576307, 0.9689951854195403280),
 ( 1.000000000000000000, 1.000000000000000000) ) ) 
 REPRESENTATION_ITEM ( '' )  SURFACE ( )  );
#4986 = EDGE_LOOP ( 'NONE', ( #6716, #22119, #10590, #21995 ) ) ;
#4987 = CARTESIAN_POINT ( 'NONE',  ( -20.57838717382308147, -27.96569011373078339, 10.78122205917029675 ) ) ;
#4988 = ORIENTED_EDGE ( 'NONE', *, *, #22535, .F. ) ;
#4989 = CARTESIAN_POINT ( 'NONE',  ( 10.93730112725990367, -104.7670965581004054, -108.9902118373752842 ) ) ;
#4990 = EDGE_CURVE ( 'NONE', #2580, #13961, #21418, .T. ) ;
#4991 = CARTESIAN_POINT ( 'NONE',  ( 25.64692232868535626, -34.58055111992117503, 107.4854307433085978 ) ) ;
#4992 = CARTESIAN_POINT ( 'NONE',  ( 25.64704443564078318, 110.4160069635933894, 23.60610532596994915 ) ) ;
#4993 = EDGE_CURVE ( 'NONE', #8105, #25030, #19129, .T. ) ;
#4994 = ORIENTED_EDGE ( 'NONE', *, *, #23226, .F. ) ;
#4995 = CARTESIAN_POINT ( 'NONE',  ( 26.11404676487259024, -45.01677474591480888, 103.8885755249567922 ) ) ;
#4996 = DIRECTION ( 'NONE',  ( 0.000000000000000000, 5.223019709707975211E-21, -1.000000000000000000 ) ) ;
#4997 = CARTESIAN_POINT ( 'NONE',  ( -28.13707043255157103, 18.96624908365847162, -12.83104814250460990 ) ) ;
#4998 = ORIENTED_EDGE ( 'NONE', *, *, #7972, .T. ) ;
#4999 = EDGE_CURVE ( 'NONE', #15484, #10441, #21559, .T. ) ;
#5000 = ORIENTED_EDGE ( 'NONE', *, *, #4993, .F. ) ;
#5001 = ORIENTED_EDGE ( 'NONE', *, *, #10476, .T. ) ;
#5002 = CARTESIAN_POINT ( 'NONE',  ( -4.473127245936434626, -47.80062405537809411, -12.17046501147497750 ) ) ;
#5003 = LINE ( 'NONE', #124, #7520 ) ;
#5004 = CARTESIAN_POINT ( 'NONE',  ( -1.113548883309548376, -38.22628252420791739, 25.34012683631596374 ) ) ;
#5005 = CARTESIAN_POINT ( 'NONE',  ( -6.588769196390758864, 51.10255870850473769, 4.956336548259831609 ) ) ;
#5006 = B_SPLINE_CURVE_WITH_KNOTS ( 'NONE', 3,
 ( #9235, #26778, #7091, #15849 ),
 .UNSPECIFIED., .F., .F.,
 ( 4, 4 ),
 ( 0.000000000000000000, 0.01077107196513881274 ),
 .UNSPECIFIED. ) ;
#5007 = CARTESIAN_POINT ( 'NONE',  ( -25.21435515916043713, -25.00736669481004526, 23.92354251275963861 ) ) ;
#5008 = CARTESIAN_POINT ( 'NONE',  ( 25.87036335909430207, 46.88819766600106931, 102.8789780196089936 ) ) ;
#5009 = ORIENTED_EDGE ( 'NONE', *, *, #8118, .F. ) ;
#5010 = CARTESIAN_POINT ( 'NONE',  ( 2.433796855181219243, 118.5671979538068257, -84.34988187690807138 ) ) ;
#5011 = CARTESIAN_POINT ( 'NONE',  ( -20.20700224038492721, 0.9908225410482660589, 29.58392382092671724 ) ) ;
#5012 = CARTESIAN_POINT ( 'NONE',  ( 109.1592201516379674, -0.004194960840990111066, -0.006649399203953448162 ) ) ;
#5013 = CARTESIAN_POINT ( 'NONE',  ( -20.57838717382308147, 10.78122205917039977, 27.96569011373074076 ) ) ;
#5014 = CARTESIAN_POINT ( 'NONE',  ( -1.619063947482197729, -35.99532424477357750, 29.22875152547795707 ) ) ;
#5015 = ORIENTED_EDGE ( 'NONE', *, *, #15033, .T. ) ;
#5016 = CARTESIAN_POINT ( 'NONE',  ( 25.64660436782554598, -12.37913844082964410, -112.2303901742707950 ) ) ;
#5017 = VERTEX_POINT ( 'NONE', #16959 ) ;
#5018 = CARTESIAN_POINT ( 'NONE',  ( 26.04756280548352976, 110.4687147111163199, -24.61655718144232097 ) ) ;
#5019 = CARTESIAN_POINT ( 'NONE',  ( 32.73300124599735739, 51.32617430724909013, 105.8473486001052777 ) ) ;
#5020 = EDGE_LOOP ( 'NONE', ( #22422, #18386, #10870, #19373 ) ) ;
#5021 = VERTEX_POINT ( 'NONE', #6185 ) ;
#5022 = ORIENTED_EDGE ( 'NONE', *, *, #11967, .T. ) ;
#5023 = CARTESIAN_POINT ( 'NONE',  ( 32.73300124599732186, 0.000000000000000000, 0.000000000000000000 ) ) ;
#5024 = CARTESIAN_POINT ( 'NONE',  ( 2.430230287190581429, 96.28466919684099423, 109.1043569252017420 ) ) ;
#5025 = CARTESIAN_POINT ( 'NONE',  ( 32.73300124599732186, 0.000000000000000000, 0.000000000000000000 ) ) ;
#5026 = CARTESIAN_POINT ( 'NONE',  ( 19.66333377628702195, 18.85786579350133607, -136.4524620437342435 ) ) ;
#5027 = VERTEX_POINT ( 'NONE', #1695 ) ;
#5028 = FACE_OUTER_BOUND ( 'NONE', #8473, .T. ) ;
#5029 = ADVANCED_FACE ( 'NONE', ( #28167 ), #6817, .F. ) ;
#5030 = CARTESIAN_POINT ( 'NONE',  ( 1.833603222531970944, 45.26427810763087933, -137.8693250773473267 ) ) ;
#5031 =( BOUNDED_SURFACE ( )  B_SPLINE_SURFACE ( 3, 1, ( 
 ( #28024, #8324 ),
 ( #17230, #19955 ),
 ( #18207, #2671 ),
 ( #664, #2824 ) ),
 .UNSPECIFIED., .F., .F., .F. ) 
 B_SPLINE_SURFACE_WITH_KNOTS ( ( 4, 4 ),
 ( 2, 2 ),
 ( 0.000000000000000000, 1.000000000000000000 ),
 ( 0.000000000000000000, 1.000000000000000000 ),
 .UNSPECIFIED. ) 
 GEOMETRIC_REPRESENTATION_ITEM ( )  RATIONAL_B_SPLINE_SURFACE ( (
 ( 1.000000000000000000, 1.000000000000000000),
 ( 0.9960225298536222738, 0.9999952330161893110),
 ( 0.9960225298536222738, 0.9999952330161893110),
 ( 1.000000000000000000, 1.000000000000000000) ) ) 
 REPRESENTATION_ITEM ( '' )  SURFACE ( )  );
#5032 = CARTESIAN_POINT ( 'NONE',  ( -20.20700224038492721, -27.82980252387826781, -10.08426345511578504 ) ) ;
#5033 = ORIENTED_EDGE ( 'NONE', *, *, #10867, .T. ) ;
#5034 = ADVANCED_FACE ( 'NONE', ( #19259 ), #27401, .F. ) ;
#5035 = B_SPLINE_CURVE_WITH_KNOTS ( 'NONE', 3,
 ( #14687, #23493, #27359, #9970, #1595, #27503, #12254 ),
 .UNSPECIFIED., .F., .F.,
 ( 4, 3, 4 ),
 ( 0.0004157520161266013833, 0.0005492286108966324548, 0.0008315040496093446809 ),
 .UNSPECIFIED. ) ;
#5036 = ORIENTED_EDGE ( 'NONE', *, *, #14570, .T. ) ;
#5037 = LINE ( 'NONE', #9956, #5619 ) ;
#5038 = CARTESIAN_POINT ( 'NONE',  ( 32.73300124599741423, 114.2056417606551406, -28.19767303745493336 ) ) ;
#5039 = CARTESIAN_POINT ( 'NONE',  ( -55.24198130335446422, -0.008252882783648586573, -0.004276389980780055493 ) ) ;
#5040 = ADVANCED_FACE ( 'NONE', ( #10077 ), #8830, .F. ) ;
#5041 = CARTESIAN_POINT ( 'NONE',  ( 109.1778270068192853, 0.004958088776550212406, -0.007885345421907750257 ) ) ;
#5042 = CARTESIAN_POINT ( 'NONE',  ( -1.583189561560252701, -46.33203782964464068, -2.490696082059713046 ) ) ;
#5043 = ORIENTED_EDGE ( 'NONE', *, *, #12995, .T. ) ;
#5044 = AXIS2_PLACEMENT_3D ( 'NONE', #5843, #3663, #25973 ) ;
#5045 = CARTESIAN_POINT ( 'NONE',  ( -55.24271866751342941, -0.006757859501009782881, 0.006671293903667897471 ) ) ;
#5046 = CARTESIAN_POINT ( 'NONE',  ( 109.1586900883932856, 0.007088091345232578125, 0.0008465529156546095163 ) ) ;
#5047 = B_SPLINE_CURVE_WITH_KNOTS ( 'NONE', 3,
 ( #17313, #26102, #6391, #26656, #15722, #16750, #23376 ),
 .UNSPECIFIED., .F., .F.,
 ( 4, 3, 4 ),
 ( 0.000000000000000000, 0.02398743853561295311, 0.04000277880656212537 ),
 .UNSPECIFIED. ) ;
#5048 = B_SPLINE_CURVE_WITH_KNOTS ( 'NONE', 3,
 ( #3861, #25180, #8063, #25480, #14210, #14512, #21413, #18983, #27761, #1686 ),
 .UNSPECIFIED., .F., .F.,
 ( 4, 3, 3, 4 ),
 ( 0.000000000000000000, 0.0002669560319015692193, 0.0005492286108966405863, 0.0008315040496093498851 ),
 .UNSPECIFIED. ) ;
#5049 = CARTESIAN_POINT ( 'NONE',  ( 109.1589550718175161, -0.007270618150635364818, -0.002126635388718505718 ) ) ;
#5050 = CARTESIAN_POINT ( 'NONE',  ( 25.73574536432415982, -76.18908113044813035, 83.41179791497836504 ) ) ;
#5051 = CARTESIAN_POINT ( 'NONE',  ( 9.884929003653626367, 109.0134320167746722, -103.8128997986846827 ) ) ;
#5052 = ORIENTED_EDGE ( 'NONE', *, *, #19812, .T. ) ;
#5053 = CARTESIAN_POINT ( 'NONE',  ( -20.21097721650787093, -8.835581399094968091, 28.26295598655181607 ) ) ;
#5054 = ORIENTED_EDGE ( 'NONE', *, *, #5500, .F. ) ;
#5055 = ORIENTED_EDGE ( 'NONE', *, *, #9735, .F. ) ;
#5056 = VERTEX_POINT ( 'NONE', #27892 ) ;
#5057 = CARTESIAN_POINT ( 'NONE',  ( 55.49584447822657296, -68.91748907713572692, -22.67407039687311610 ) ) ;
#5058 = CIRCLE ( 'NONE', #2760, 117.6351876552689504 ) ;
#5059 = CARTESIAN_POINT ( 'NONE',  ( 10.93730112725932635, 0.000000000000000000, 0.000000000000000000 ) ) ;
#5060 = CARTESIAN_POINT ( 'NONE',  ( -7.078251931573406708, -47.71415099571790108, 20.86696228105274997 ) ) ;
#5061 = UNCERTAINTY_MEASURE_WITH_UNIT (LENGTH_MEASURE( 1.000000000000000082E-05 ), #10377, 'distance_accuracy_value', 'NONE');
#5062 = CARTESIAN_POINT ( 'NONE',  ( -6.588769196390754423, -20.50531526814530636, 47.06982923582530276 ) ) ;
#5063 = EDGE_CURVE ( 'NONE', #23740, #15365, #24055, .T. ) ;
#5064 = CARTESIAN_POINT ( 'NONE',  ( 1.833206308920067196, -97.64934899952775993, 107.3376449983724541 ) ) ;
#5065 = CARTESIAN_POINT ( 'NONE',  ( -20.24399999263414784, -28.55700515887714275, 7.930419334766489747 ) ) ;
#5066 = DIRECTION ( 'NONE',  ( 0.000000000000000000, 0.000000000000000000, 1.000000000000000000 ) ) ;
#5067 = CARTESIAN_POINT ( 'NONE',  ( 25.98107933586745588, 113.1286487641198022, 1.091357942390989155 ) ) ;
#5068 = FACE_OUTER_BOUND ( 'NONE', #25578, .T. ) ;
#5069 = CARTESIAN_POINT ( 'NONE',  ( 25.86096068574578410, 33.98552076022196644, 107.8247115223743435 ) ) ;
#5070 = CARTESIAN_POINT ( 'NONE',  ( -22.34422965417124374, 17.95715691811047776, -33.39267070835825990 ) ) ;
#5071 = CARTESIAN_POINT ( 'NONE',  ( 2.430230287190581429, -98.44218333480841920, 107.1617224697460955 ) ) ;
#5072 = CARTESIAN_POINT ( 'NONE',  ( 55.79472521941428198, 49.22042574086425759, 53.57698701322232893 ) ) ;
#5073 = AXIS2_PLACEMENT_3D ( 'NONE', #10961, #2026, #2449 ) ;
#5074 = VECTOR ( 'NONE', #27927, 999.9999999999998863 ) ;
#5075 = B_SPLINE_CURVE_WITH_KNOTS ( 'NONE', 3,
 ( #27069, #10079, #1280, #18845, #27614, #13839, #7935, #15864, #11540, #25491 ),
 .UNSPECIFIED., .F., .F.,
 ( 4, 2, 2, 2, 4 ),
 ( 2.888718286224068903E-16, 0.0003346187017559086596, 0.0006692374035115283793, 0.001003856105267148099, 0.001338474807022767927 ),
 .UNSPECIFIED. ) ;
#5076 = CARTESIAN_POINT ( 'NONE',  ( 109.1778270068192853, 0.006682187084639316411, 0.006489198140358653361 ) ) ;
#5077 = AXIS2_PLACEMENT_3D ( 'NONE', #1981, #10782, #22388 ) ;
#5078 = CARTESIAN_POINT ( 'NONE',  ( 1.833691583653552115, -144.2771263798445887, -15.52203496789063664 ) ) ;
#5079 = CARTESIAN_POINT ( 'NONE',  ( 55.49584447822657296, -42.86099773636501453, -58.53775398922299900 ) ) ;
#5080 = CARTESIAN_POINT ( 'NONE',  ( -1.031422197589716205, 1.530725436377464499, -45.78027046666444733 ) ) ;
#5081 = CARTESIAN_POINT ( 'NONE',  ( -1.045287976400351981, 36.12803364096590997, -28.14015102489844011 ) ) ;
#5082 = ORIENTED_EDGE ( 'NONE', *, *, #13272, .F. ) ;
#5083 = CARTESIAN_POINT ( 'NONE',  ( 32.73300124599735739, 28.19767303745605602, 114.2056417606549132 ) ) ;
#5084 = CONICAL_SURFACE ( 'NONE', #12876, 117.6351876552689504, 0.9945805576725580410 ) ;
#5085 = ORIENTED_EDGE ( 'NONE', *, *, #8590, .F. ) ;
#5086 = CARTESIAN_POINT ( 'NONE',  ( 25.86096068574583029, 103.6815822123525095, -45.07009591924456515 ) ) ;
#5087 = CARTESIAN_POINT ( 'NONE',  ( -1.031422197589711764, 36.13727897780167808, 28.14735071801703725 ) ) ;
#5088 = ORIENTED_EDGE ( 'NONE', *, *, #10523, .F. ) ;
#5089 = ORIENTED_EDGE ( 'NONE', *, *, #1113, .F. ) ;
#5090 = ORIENTED_EDGE ( 'NONE', *, *, #886, .F. ) ;
#5091 = CARTESIAN_POINT ( 'NONE',  ( 109.1592201516379674, -0.0005146241775983334847, -0.007845213074654432128 ) ) ;
#5092 = EDGE_CURVE ( 'NONE', #27064, #14776, #27373, .T. ) ;
#5093 = ADVANCED_FACE ( 'NONE', ( #15338 ), #9761, .F. ) ;
#5094 = CIRCLE ( 'NONE', #23516, 34.60786435723138510 ) ;
#5095 = CONICAL_SURFACE ( 'NONE', #13367, 34.60786435723138510, 0.8559913436420825139 ) ;
#5096 = ADVANCED_FACE ( 'NONE', ( #3989 ), #10849, .F. ) ;
#5097 = B_SPLINE_CURVE_WITH_KNOTS ( 'NONE', 3,
 ( #5007, #7326, #3432, #26884, #13784, #22592, #14357 ),
 .UNSPECIFIED., .F., .F.,
 ( 4, 3, 4 ),
 ( 0.000000000000000000, 0.006568092053401826565, 0.02506242213020857396 ),
 .UNSPECIFIED. ) ;
#5098 = CARTESIAN_POINT ( 'NONE',  ( 1.832998868059890096, -132.3466930259797891, 59.50898020732464744 ) ) ;
#5099 = FACE_OUTER_BOUND ( 'NONE', #23142, .T. ) ;
#5100 = VECTOR ( 'NONE', #12463, 1000.000000000000114 ) ;
#5101 = CARTESIAN_POINT ( 'NONE',  ( 109.1721716018069515, 0.01629455849719223248, -0.005082060336465326310 ) ) ;
#5102 = CARTESIAN_POINT ( 'NONE',  ( -24.53239521893648245, -33.25736993155760501, 6.738460611583118265 ) ) ;
#5103 = LINE ( 'NONE', #1080, #544 ) ;
#5104 = CARTESIAN_POINT ( 'NONE',  ( -1.239374126674604337, -28.97829083655411964, 35.79060836339844087 ) ) ;
#5105 = DIRECTION ( 'NONE',  ( 0.000000000000000000, 5.223019709707975211E-21, -1.000000000000000000 ) ) ;
#5107 = CARTESIAN_POINT ( 'NONE',  ( 30.59138290137891047, -88.14703743378190381, -75.73279410806814838 ) ) ;
#5106 = DIRECTION ( 'NONE',  ( 0.7563875759206388771, 0.03500244528122559151, -0.6531865459554678788 ) ) ;
#5108 = CARTESIAN_POINT ( 'NONE',  ( 25.70243777736190083, 83.44449745408539343, 76.12033502296544896 ) ) ;
#5109 = EDGE_LOOP ( 'NONE', ( #7373, #24980, #15638, #17759 ) ) ;
#5110 = EDGE_LOOP ( 'NONE', ( #15024, #24395, #18397, #8044 ) ) ;
#5111 = CARTESIAN_POINT ( 'NONE',  ( -1.056502255334264895, 43.40574022158773460, -14.64009593116116292 ) ) ;
#5113 = CARTESIAN_POINT ( 'NONE',  ( -8.786685647604898008, 48.22796981442765940, -23.24040270374399952 ) ) ;
#5112 = DIRECTION ( 'NONE',  ( 0.000000000000000000, 0.000000000000000000, 1.000000000000000000 ) ) ;
#5114 = CARTESIAN_POINT ( 'NONE',  ( 30.58324630866339078, -116.1819705588610816, -33.60235057864094443 ) ) ;
#5115 = B_SPLINE_CURVE_WITH_KNOTS ( 'NONE', 3,
 ( #10959, #17561, #9081, #19869, #19723, #24495, #26768, #26349, #20151, #4611 ),
 .UNSPECIFIED., .F., .F.,
 ( 4, 3, 3, 4 ),
 ( 3.816391647148975608E-17, 0.0002669559177086135637, 0.0005339118354150864786, 0.001067817517169152757 ),
 .UNSPECIFIED. ) ;
#5116 = CARTESIAN_POINT ( 'NONE',  ( -2.911734481061406754, 44.38410240830302911, -17.36785190845994720 ) ) ;
#5117 = EDGE_LOOP ( 'NONE', ( #3998, #2460, #4128, #10975 ) ) ;
#5118 = ORIENTED_EDGE ( 'NONE', *, *, #10105, .F. ) ;
#5119 = CARTESIAN_POINT ( 'NONE',  ( 1.833485406944043827, 45.34878176254236593, 137.8414413349087511 ) ) ;
#5120 = AXIS2_PLACEMENT_3D ( 'NONE', #4185, #24341, #12818 ) ;
#5121 = CARTESIAN_POINT ( 'NONE',  ( -25.21435515916043357, -34.29329011225959079, -4.655591116594231416 ) ) ;
#5122 = CARTESIAN_POINT ( 'NONE',  ( 109.1592201516379674, 0.007302213399779926284, -0.002913740842108661615 ) ) ;
#5123 = VERTEX_POINT ( 'NONE', #26080 ) ;
#5124 = CARTESIAN_POINT ( 'NONE',  ( -55.25719721206881729, -0.002847566758683717138, -0.01079965405819494247 ) ) ;
#5125 = AXIS2_PLACEMENT_3D ( 'NONE', #9733, #7585, #22846 ) ;
#5126 = ORIENTED_EDGE ( 'NONE', *, *, #10304, .T. ) ;
#5127 = DIRECTION ( 'NONE',  ( 0.000000000000000000, 0.000000000000000000, 1.000000000000000000 ) ) ;
#5128 = EDGE_CURVE ( 'NONE', #22381, #22329, #21907, .T. ) ;
#5129 = CARTESIAN_POINT ( 'NONE',  ( -1.155031165708882757, 2.068616213631583545, 45.85732438018710866 ) ) ;
#5130 = CARTESIAN_POINT ( 'NONE',  ( 2.108985857320890389, -132.2056553747750343, 60.26444811757351516 ) ) ;
#5131 = ORIENTED_EDGE ( 'NONE', *, *, #12730, .T. ) ;
#5132 = CARTESIAN_POINT ( 'NONE',  ( -1.019300379054419725, 35.83762006677400791, -28.53917295602911253 ) ) ;
#5133 = ADVANCED_FACE ( 'NONE', ( #17717 ), #6655, .F. ) ;
#5134 = VERTEX_POINT ( 'NONE', #8811 ) ;
#5135 = CARTESIAN_POINT ( 'NONE',  ( -21.41430102051752016, -16.60879216503617073, 25.94791611261633690 ) ) ;
#5136 = B_SPLINE_CURVE_WITH_KNOTS ( 'NONE', 3,
 ( #10119, #25666, #5655, #5945, #21465, #3770, #10407, #1738, #18890, #10537 ),
 .UNSPECIFIED., .F., .F.,
 ( 4, 3, 3, 4 ),
 ( 3.816391647148975608E-17, 0.0002669559177086172500, 0.0005339118354150979712, 0.001067817517169165550 ),
 .UNSPECIFIED. ) ;
#5137 = ORIENTED_EDGE ( 'NONE', *, *, #16551, .T. ) ;
#5138 = CARTESIAN_POINT ( 'NONE',  ( 28.43349137099829349, -94.99961975860206564, -80.08535015164004278 ) ) ;
#5139 = CARTESIAN_POINT ( 'NONE',  ( -1.045287976400386842, 37.92705037016744285, -25.66401692420027203 ) ) ;
#5140 = CARTESIAN_POINT ( 'NONE',  ( 28.37599760073043242, -75.42809173301549208, -86.45296943207098650 ) ) ;
#5141 = CARTESIAN_POINT ( 'NONE',  ( -25.21435515916043002, -4.655591116594591128, -34.29329011225954105 ) ) ;
#5142 = VERTEX_POINT ( 'NONE', #17574 ) ;
#5143 = CARTESIAN_POINT ( 'NONE',  ( -55.24390624410018802, 0.001451500391951047672, 0.01032895241566990016 ) ) ;
#5144 = FACE_OUTER_BOUND ( 'NONE', #23949, .T. ) ;
#5145 = CARTESIAN_POINT ( 'NONE',  ( 25.98552792386799126, 98.51438617140739495, 55.63155129532967891 ) ) ;
#5146 = ORIENTED_EDGE ( 'NONE', *, *, #25133, .F. ) ;
#5147 = VECTOR ( 'NONE', #17005, 1000.000000000000000 ) ;
#5148 = ORIENTED_EDGE ( 'NONE', *, *, #21292, .F. ) ;
#5149 = ORIENTED_EDGE ( 'NONE', *, *, #14886, .T. ) ;
#5150 = CARTESIAN_POINT ( 'NONE',  ( -20.20700224038492010, 8.199606986804733211, 28.44216453106527709 ) ) ;
#5151 = CARTESIAN_POINT ( 'NONE',  ( 1.831572820252008738, -132.9644823688599331, 58.11906524360431803 ) ) ;
#5153 = DIRECTION ( 'NONE',  ( -0.5946245182733608248, -0.4045541647807384122, -0.6948076064830700505 ) ) ;
#5152 = CARTESIAN_POINT ( 'NONE',  ( -22.34422965417125795, -37.57019010019543970, 5.100074259622997097 ) ) ;
#5154 = CARTESIAN_POINT ( 'NONE',  ( -4.780792508754322157, 49.38761389561003767, 3.764354093953751423 ) ) ;
#5155 = CARTESIAN_POINT ( 'NONE',  ( 1.833809397773845662, 107.7184108265663980, 97.22957127128873367 ) ) ;
#5156 = CARTESIAN_POINT ( 'NONE',  ( -1.044557008772710516, -28.22896138707343994, 36.05793264791374497 ) ) ;
#5157 = EDGE_LOOP ( 'NONE', ( #10733, #24610, #5148, #26275 ) ) ;
#5158 = CARTESIAN_POINT ( 'NONE',  ( -25.21435515916043713, 23.92354251275973809, 25.00736669480994934 ) ) ;
#5159 = CARTESIAN_POINT ( 'NONE',  ( -20.20700224038492721, -23.35150625415645820, 18.19058640100249491 ) ) ;
#5160 = CARTESIAN_POINT ( 'NONE',  ( 109.1592201516379674, -0.006174480289199440856, 0.004867031887019522031 ) ) ;
#5161 = CARTESIAN_POINT ( 'NONE',  ( 109.1586059443104944, -0.004935564877218434968, 0.005067816690893726939 ) ) ;
#5162 = CARTESIAN_POINT ( 'NONE',  ( -24.53239521893627995, 33.25736993155740606, -6.738460611583019677 ) ) ;
#5163 = ORIENTED_EDGE ( 'NONE', *, *, #10092, .T. ) ;
#5164 = B_SPLINE_CURVE_WITH_KNOTS ( 'NONE', 3,
 ( #14915, #23735, #10348, #25308, #6023, #21109, #1397, #27451 ),
 .UNSPECIFIED., .F., .F.,
 ( 4, 2, 2, 4 ),
 ( 0.000000000000000000, 0.002761524886576651079, 0.005523049773153302158, 0.01104609954630660432 ),
 .UNSPECIFIED. ) ;
#5165 = EDGE_CURVE ( 'NONE', #19216, #26175, #5792, .T. ) ;
#5166 = CARTESIAN_POINT ( 'NONE',  ( -20.24399999263414784, 16.36687688782894412, 24.70869149526185282 ) ) ;
#5167 = CARTESIAN_POINT ( 'NONE',  ( 109.1586900883932856, 0.002995460350180810267, -0.006479576224403795805 ) ) ;
#5168 = ORIENTED_EDGE ( 'NONE', *, *, #25133, .T. ) ;
#5169 = EDGE_CURVE ( 'NONE', #21319, #15966, #13252, .T. ) ;
#5170 = CIRCLE ( 'NONE', #10688, 117.6351876552689504 ) ;
#5171 = ORIENTED_EDGE ( 'NONE', *, *, #21445, .F. ) ;
#5172 = ORIENTED_EDGE ( 'NONE', *, *, #3303, .F. ) ;
#5173 = VECTOR ( 'NONE', #6362, 1000.000000000000227 ) ;
#5174 = EDGE_CURVE ( 'NONE', #15441, #17576, #9167, .T. ) ;
#5175 = CARTESIAN_POINT ( 'NONE',  ( 26.11404676487257603, 84.89295829319495112, 74.91683232331003239 ) ) ;
#5176 = EDGE_CURVE ( 'NONE', #10776, #2577, #4032, .T. ) ;
#5177 = CARTESIAN_POINT ( 'NONE',  ( 24.22246935314087324, -69.99999999999998579, -40.00000000000002132 ) ) ;
#5178 = CARTESIAN_POINT ( 'NONE',  ( 2.433796855181233454, 144.8571464219889151, 13.76554153471742481 ) ) ;
#5179 = CARTESIAN_POINT ( 'NONE',  ( 5.340103556456345046, 108.0219267027630252, 100.3626145793565172 ) ) ;
#5180 = EDGE_LOOP ( 'NONE', ( #802, #3561, #25283, #12153 ) ) ;
#5181 = CARTESIAN_POINT ( 'NONE',  ( -10.86508079875781974, 22.20099862734820562, -46.07061504567093380 ) ) ;
#5182 = CARTESIAN_POINT ( 'NONE',  ( 25.64703792032473118, 35.03296646432561090, 107.3388703233122783 ) ) ;
#5183 = CARTESIAN_POINT ( 'NONE',  ( 1.893872463202041612, -116.8661275359691700, -86.08597552418997623 ) ) ;
#5184 = VERTEX_POINT ( 'NONE', #6947 ) ;
#5185 = VERTEX_POINT ( 'NONE', #9668 ) ;
#5186 = CARTESIAN_POINT ( 'NONE',  ( -1.583189561560253589, -36.01941156322766346, 29.24830400313204848 ) ) ;
#5187 = CARTESIAN_POINT ( 'NONE',  ( -1.048172774974294619, -36.44231470008696760, 27.73787987941047817 ) ) ;
#5188 = CARTESIAN_POINT ( 'NONE',  ( 109.1592201516379674, 0.007376275279030877242, 0.002720803050361335265 ) ) ;
#5189 = DIRECTION ( 'NONE',  ( 0.000000000000000000, 0.000000000000000000, 1.000000000000000000 ) ) ;
#5190 = CARTESIAN_POINT ( 'NONE',  ( 1.831572820252008738, 137.7011124121617058, 45.77972211429861460 ) ) ;
#5191 = CARTESIAN_POINT ( 'NONE',  ( -1.155001620486251213, 2.068551059060327546, -45.85729774065935516 ) ) ;
#5192 = EDGE_LOOP ( 'NONE', ( #4574, #13786, #23413, #13637 ) ) ;
#5193 = CARTESIAN_POINT ( 'NONE',  ( -55.24300891470650754, -0.009439835024158502175, -0.002702093572893477045 ) ) ;
#5194 = DIRECTION ( 'NONE',  ( 0.000000000000000000, 5.223019709707975211E-21, -1.000000000000000000 ) ) ;
#5195 = B_SPLINE_CURVE_WITH_KNOTS ( 'NONE', 3,
 ( #358, #650, #4829, #9145, #17900, #9439 ),
 .UNSPECIFIED., .F., .F.,
 ( 4, 2, 4 ),
 ( 3.208066105977133993E-16, 0.003576372551511132307, 0.007152745103021943690 ),
 .UNSPECIFIED. ) ;
#5196 = CARTESIAN_POINT ( 'NONE',  ( -1.463510566862827655, 44.64091840826493041, -11.94877850058517765 ) ) ;
#5197 = CARTESIAN_POINT ( 'NONE',  ( 25.70243777736191859, -76.12033502296576160, 83.44449745408508079 ) ) ;
#5198 = FACE_OUTER_BOUND ( 'NONE', #1036, .T. ) ;
#5199 = VERTEX_POINT ( 'NONE', #18145 ) ;
#5200 = B_SPLINE_CURVE_WITH_KNOTS ( 'NONE', 3,
 ( #20264, #11642, #16240, #22446, #699, #9781, #2714, #11792, #9354, #7196 ),
 .UNSPECIFIED., .F., .F.,
 ( 4, 2, 2, 2, 4 ),
 ( 4.210279659405072890E-18, 0.0003346267210630970664, 0.0006692534421261899045, 0.001003880163189282580, 0.001338506884252375472 ),
 .UNSPECIFIED. ) ;
#5201 = EDGE_LOOP ( 'NONE', ( #16212, #25599, #17051, #27369 ) ) ;
#5202 = CARTESIAN_POINT ( 'NONE',  ( 1.833838850855489255, 145.1097630809417467, 0.08898185259624630250 ) ) ;
#5203 = ORIENTED_EDGE ( 'NONE', *, *, #7633, .T. ) ;
#5204 = EDGE_CURVE ( 'NONE', #17827, #2087, #15319, .T. ) ;
#5205 = VERTEX_POINT ( 'NONE', #13683 ) ;
#5206 = ORIENTED_EDGE ( 'NONE', *, *, #21632, .F. ) ;
#5207 = EDGE_CURVE ( 'NONE', #12120, #4838, #12946, .T. ) ;
#5209 =( BOUNDED_SURFACE ( )  B_SPLINE_SURFACE ( 3, 1, ( 
 ( #21847, #11325 ),
 ( #11046, #379 ),
 ( #2386, #2683 ),
 ( #24294, #15619 ) ),
 .UNSPECIFIED., .F., .F., .F. ) 
 B_SPLINE_SURFACE_WITH_KNOTS ( ( 4, 4 ),
 ( 2, 2 ),
 ( 0.000000000000000000, 1.000000000000000000 ),
 ( 0.000000000000000000, 1.000000000000000000 ),
 .UNSPECIFIED. ) 
 GEOMETRIC_REPRESENTATION_ITEM ( )  RATIONAL_B_SPLINE_SURFACE ( (
 ( 1.000000000000000000, 1.000000000000000000),
 ( 0.6386103224230302855, 0.9954351624131538845),
 ( 0.6386103224230302855, 0.9954351624131538845),
 ( 1.000000000000000000, 1.000000000000000000) ) ) 
 REPRESENTATION_ITEM ( '' )  SURFACE ( )  );
#5208 = VECTOR ( 'NONE', #17213, 1000.000000000000114 ) ;
#5210 = CARTESIAN_POINT ( 'NONE',  ( -55.24390624410018802, 0.009209468562452933355, 0.004896917417131438528 ) ) ;
#5211 = AXIS2_PLACEMENT_3D ( 'NONE', #6830, #12145, #23242 ) ;
#5212 = CARTESIAN_POINT ( 'NONE',  ( 109.1592201516379674, 0.006174480289199407029, -0.004867031887019566266 ) ) ;
#5213 = CARTESIAN_POINT ( 'NONE',  ( -21.41430102051751305, -23.81424706376350287, 19.54553566814611898 ) ) ;
#5214 = B_SPLINE_CURVE_WITH_KNOTS ( 'NONE', 3,
 ( #666, #6589, #13469, #17915, #24148, #20224, #4410, #520, #22266, #13614 ),
 .UNSPECIFIED., .F., .F.,
 ( 4, 3, 3, 4 ),
 ( 3.469446951953614189E-18, 0.0002669560319015759414, 0.0005492286108966491515, 0.0008315040496093429462 ),
 .UNSPECIFIED. ) ;
#5215 = CARTESIAN_POINT ( 'NONE',  ( -12.94347594948494340, 6.555928820869281637, -48.30328466416744249 ) ) ;
#5216 = CARTESIAN_POINT ( 'NONE',  ( 119.2224693531408803, 90.00000000000005684, 39.99999999999999289 ) ) ;
#5217 = ADVANCED_FACE ( 'NONE', ( #5198 ), #14551, .F. ) ;
#5218 = CARTESIAN_POINT ( 'NONE',  ( 10.93730112725995873, 4.928439153522441885, -151.0983828010091656 ) ) ;
#5219 = CARTESIAN_POINT ( 'NONE',  ( 109.1592201516379674, -0.007620268632968129653, -0.001934867487012907703 ) ) ;
#5220 = CARTESIAN_POINT ( 'NONE',  ( -20.21097721650786738, -9.464413208035280078, -28.05863614620935209 ) ) ;
#5221 = CARTESIAN_POINT ( 'NONE',  ( -10.86508079875782329, 24.22249093393363850, 45.04061326950845512 ) ) ;
#5222 = CARTESIAN_POINT ( 'NONE',  ( -8.786685647604885574, 6.096987947571466530E-17, -1.524246986892866633E-17 ) ) ;
#5224 = CARTESIAN_POINT ( 'NONE',  ( 16.05277956358209579, -25.20902801311468266, 141.0713346807233393 ) ) ;
#5223 = CARTESIAN_POINT ( 'NONE',  ( -21.81686047589426991, 6.867757412721210208, 37.90526371014249918 ) ) ;
#5225 = CARTESIAN_POINT ( 'NONE',  ( 25.64660436782543940, 75.98230157781860328, 83.52001792470919384 ) ) ;
#5226 = CARTESIAN_POINT ( 'NONE',  ( 25.64704443564077252, 45.80316013050833135, 103.2037466592375807 ) ) ;
#5227 = CARTESIAN_POINT ( 'NONE',  ( 13.36082413113061307, -152.6206443696329416, 9.660980093454195838 ) ) ;
#5228 = CARTESIAN_POINT ( 'NONE',  ( 13.36082413113063083, 117.7941133658638790, 97.52406103376794988 ) ) ;
#5229 = ORIENTED_EDGE ( 'NONE', *, *, #4041, .T. ) ;
#5230 = DIRECTION ( 'NONE',  ( -0.5946245182733607137, 0.7332888028688970827, -0.3297108033645145819 ) ) ;
#5231 = ORIENTED_EDGE ( 'NONE', *, *, #21295, .T. ) ;
#5232 = CARTESIAN_POINT ( 'NONE',  ( -20.20700224038492365, 23.35150625415685255, 18.19058640100197977 ) ) ;
#5233 = CARTESIAN_POINT ( 'NONE',  ( 1.893872463202043832, 0.9528309182417881162, -145.1467500857187929 ) ) ;
#5234 = VERTEX_POINT ( 'NONE', #3187 ) ;
#5235 = EDGE_CURVE ( 'NONE', #28150, #7707, #3659, .T. ) ;
#5236 = ORIENTED_EDGE ( 'NONE', *, *, #1183, .T. ) ;
#5237 = ORIENTED_EDGE ( 'NONE', *, *, #8172, .F. ) ;
#5238 = B_SPLINE_CURVE_WITH_KNOTS ( 'NONE', 3,
 ( #12258, #7967, #16574, #2647, #7133, #4817, #2792 ),
 .UNSPECIFIED., .F., .F.,
 ( 4, 3, 4 ),
 ( 0.000000000000000000, 0.02398743853561391762, 0.04000277880656258334 ),
 .UNSPECIFIED. ) ;
#5239 = ADVANCED_FACE ( 'NONE', ( #7234 ), #25890, .T. ) ;
#5240 = ADVANCED_FACE ( 'NONE', ( #24662 ), #12688, .F. ) ;
#5241 = CARTESIAN_POINT ( 'NONE',  ( -1.019300379054419725, 12.21833869579464604, -44.15350047934403221 ) ) ;
#5242 =( BOUNDED_SURFACE ( )  B_SPLINE_SURFACE ( 3, 1, ( 
 ( #13901, #10177 ),
 ( #14470, #1371 ),
 ( #7443, #3400 ),
 ( #5715, #22710 ) ),
 .UNSPECIFIED., .F., .F., .F. ) 
 B_SPLINE_SURFACE_WITH_KNOTS ( ( 4, 4 ),
 ( 2, 2 ),
 ( 0.000000000000000000, 1.000000000000000000 ),
 ( 0.000000000000000000, 1.000000000000000000 ),
 .UNSPECIFIED. ) 
 GEOMETRIC_REPRESENTATION_ITEM ( )  RATIONAL_B_SPLINE_SURFACE ( (
 ( 1.000000000000000000, 1.000000000000000000),
 ( 0.7789835883360576307, 0.9689951854195403280),
 ( 0.7789835883360576307, 0.9689951854195403280),
 ( 1.000000000000000000, 1.000000000000000000) ) ) 
 REPRESENTATION_ITEM ( '' )  SURFACE ( )  );
#5243 = EDGE_CURVE ( 'NONE', #19356, #12270, #5035, .T. ) ;
#5244 = FACE_OUTER_BOUND ( 'NONE', #22142, .T. ) ;
#5245 = CARTESIAN_POINT ( 'NONE',  ( 1.833721034905634317, 144.2772269874178050, -15.52204855105691905 ) ) ;
#5246 = FACE_OUTER_BOUND ( 'NONE', #5937, .T. ) ;
#5247 = CARTESIAN_POINT ( 'NONE',  ( 10.93730112725970294, 65.95960219663110990, 136.0306644680985642 ) ) ;
#5248 = CARTESIAN_POINT ( 'NONE',  ( 32.73300124599735028, 84.80615050150375112, 81.52272205837232377 ) ) ;
#5249 = CARTESIAN_POINT ( 'NONE',  ( 1.833838848569416147, -59.18404309081275017, -132.4919773286275415 ) ) ;
#5250 = CARTESIAN_POINT ( 'NONE',  ( -1.619063947482194177, 29.22875152547808852, 35.99532424477347092 ) ) ;
#5251 = LINE ( 'NONE', #3240, #20810 ) ;
#5252 = CARTESIAN_POINT ( 'NONE',  ( 26.11404676487257603, 83.38016054979783576, 76.59696442953219275 ) ) ;
#5253 = ORIENTED_EDGE ( 'NONE', *, *, #17089, .F. ) ;
#5254 = DIRECTION ( 'NONE',  ( 0.7563875759206388771, -0.2351350468682826267, 0.6104009704506950795 ) ) ;
#5256 = CARTESIAN_POINT ( 'NONE',  ( -1.323830074806759960, 25.17121255494532406, 38.58891736138504314 ) ) ;
#5255 = CARTESIAN_POINT ( 'NONE',  ( -21.41427618760458884, 11.22988868156184772, -28.68857606049970244 ) ) ;
#5257 = CARTESIAN_POINT ( 'NONE',  ( -15.02187109954786060, -8.264310930412701595, -45.60876405941874623 ) ) ;
#5258 = FACE_OUTER_BOUND ( 'NONE', #24, .T. ) ;
#5259 = CARTESIAN_POINT ( 'NONE',  ( 1.833206310202336153, 144.3905118062894530, 14.42724831649402617 ) ) ;
#5260 = EDGE_CURVE ( 'NONE', #5291, #25128, #12289, .T. ) ;
#5261 = ORIENTED_EDGE ( 'NONE', *, *, #27085, .T. ) ;
#5262 = CARTESIAN_POINT ( 'NONE',  ( -22.23342874802667879, -30.68433055777675733, 7.677086057585283285 ) ) ;
#5263 = CARTESIAN_POINT ( 'NONE',  ( -1.155001620486253877, 45.85729774065937647, 2.068551059060488750 ) ) ;
#5264 = CARTESIAN_POINT ( 'NONE',  ( -1.155001620486248548, -38.31519699443482097, 25.28075036143263077 ) ) ;
#5265 = ORIENTED_EDGE ( 'NONE', *, *, #18518, .T. ) ;
#5266 = CARTESIAN_POINT ( 'NONE',  ( -25.21435515916025594, 1.749597353048488237E-16, -4.373993382621220594E-17 ) ) ;
#5268 = ORIENTED_EDGE ( 'NONE', *, *, #6000, .T. ) ;
#5267 = EDGE_CURVE ( 'NONE', #26744, #27903, #6419, .T. ) ;
#5269 = CARTESIAN_POINT ( 'NONE',  ( 25.64670758986456889, -112.3434365398309041, 11.30712635241953024 ) ) ;
#5270 = EDGE_CURVE ( 'NONE', #4384, #21682, #8227, .T. ) ;
#5271 = CARTESIAN_POINT ( 'NONE',  ( -24.53239521893647179, -33.71193723315173685, -3.868435622621356096 ) ) ;
#5272 = CARTESIAN_POINT ( 'NONE',  ( -20.20700224038492721, 0.9908225410478516126, -29.58392382092673145 ) ) ;
#5273 = VERTEX_POINT ( 'NONE', #9823 ) ;
#5274 = CARTESIAN_POINT ( 'NONE',  ( 109.1624594426973260, 0.001206615835671176864, 0.01591840958352308891 ) ) ;
#5275 = ORIENTED_EDGE ( 'NONE', *, *, #9945, .T. ) ;
#5276 = CARTESIAN_POINT ( 'NONE',  ( -24.53237795827032031, -16.68575684089471878, 29.54731592868582979 ) ) ;
#5277 = B_SPLINE_CURVE_WITH_KNOTS ( 'NONE', 3,
 ( #25861, #19642, #2216, #1945, #17070, #80, #3840, #4394 ),
 .UNSPECIFIED., .F., .F.,
 ( 4, 2, 2, 4 ),
 ( 6.938893903907228378E-18, 0.0002429588503611338987, 0.0004859177007222608585, 0.0009718354014444862635 ),
 .UNSPECIFIED. ) ;
#5278 = ORIENTED_EDGE ( 'NONE', *, *, #15826, .T. ) ;
#5279 = B_SPLINE_CURVE_WITH_KNOTS ( 'NONE', 3,
 ( #9578, #22985, #3104, #27272 ),
 .UNSPECIFIED., .F., .F.,
 ( 4, 4 ),
 ( 0.000000000000000000, 0.01077107196513891682 ),
 .UNSPECIFIED. ) ;
#5280 = APPLICATION_PROTOCOL_DEFINITION ( 'draft international standard', 'automotive_design', 1998, #21866 ) ;
#5281 = CARTESIAN_POINT ( 'NONE',  ( 32.73300124599733607, 103.7392577722176270, 55.46353551262048853 ) ) ;
#5282 = CARTESIAN_POINT ( 'NONE',  ( 25.64681081121879203, 107.5125461021407318, -34.49579773461672971 ) ) ;
#5283 = CARTESIAN_POINT ( 'NONE',  ( -55.24340739397742084, 0.009842732675352565408, -0.002421372372454350108 ) ) ;
#5284 = B_SPLINE_CURVE_WITH_KNOTS ( 'NONE', 3,
 ( #7723, #16478, #17037, #23123 ),
 .UNSPECIFIED., .F., .F.,
 ( 4, 4 ),
 ( 2.005388357681274105E-16, 0.001982023823822939412 ),
 .UNSPECIFIED. ) ;
#5285 = EDGE_LOOP ( 'NONE', ( #781, #27994, #23543, #23280 ) ) ;
#5286 = CARTESIAN_POINT ( 'NONE',  ( -20.57838717382308147, 29.92853265176831812, -1.611677988432464126 ) ) ;
#5287 = CARTESIAN_POINT ( 'NONE',  ( -1.048996300304511298, 43.31387123529979277, -14.87787369922182990 ) ) ;
#5288 = CARTESIAN_POINT ( 'NONE',  ( -22.23342874802668589, 26.81018246605539446, -16.78332232459650797 ) ) ;
#5289 = EDGE_LOOP ( 'NONE', ( #9575, #7580, #17038, #17449 ) ) ;
#5290 = B_SPLINE_CURVE_WITH_KNOTS ( 'NONE', 3,
 ( #13391, #15695, #22190, #2457, #4476, #15 ),
 .UNSPECIFIED., .F., .F.,
 ( 4, 2, 4 ),
 ( 6.952433221959954168E-18, 0.0006311571484585832377, 0.001262314296917159536 ),
 .UNSPECIFIED. ) ;
#5291 = VERTEX_POINT ( 'NONE', #25653 ) ;
#5292 = ORIENTED_EDGE ( 'NONE', *, *, #7679, .F. ) ;
#5293 = CARTESIAN_POINT ( 'NONE',  ( -1.050229599974481065, 36.90196321294333615, 27.12684363859215608 ) ) ;
#5294 = FACE_OUTER_BOUND ( 'NONE', #25868, .T. ) ;
#5296 = CARTESIAN_POINT ( 'NONE',  ( 25.64681081121879203, 11.38886654529823694, -112.3352186517029594 ) ) ;
#5295 = CARTESIAN_POINT ( 'NONE',  ( 1.833691583653511925, 108.0753610255266466, -96.83253123394105444 ) ) ;
#5297 = CARTESIAN_POINT ( 'NONE',  ( -7.711401346138264223, -38.61705198405337569, 35.51061203065550131 ) ) ;
#5298 = CARTESIAN_POINT ( 'NONE',  ( -20.38016308990357928, -18.69911008768351479, -23.16952666206578826 ) ) ;
#5299 = CARTESIAN_POINT ( 'NONE',  ( 26.28373643307403995, -127.4927519498667010, 4.159810388345953847 ) ) ;
#5300 = EDGE_CURVE ( 'NONE', #25430, #3869, #14407, .T. ) ;
#5301 = VERTEX_POINT ( 'NONE', #16431 ) ;
#5302 = CARTESIAN_POINT ( 'NONE',  ( -1.619063947482197729, -29.22875152547730337, 35.99532424477411041 ) ) ;
#5303 = CARTESIAN_POINT ( 'NONE',  ( -1.113427685307007975, 44.18561238466754304, 12.28784199929889098 ) ) ;
#5304 = CARTESIAN_POINT ( 'NONE',  ( 109.1589550718174877, -0.007453082872776649326, 0.001354998915261305167 ) ) ;
#5305 = ADVANCED_FACE ( 'NONE', ( #19021 ), #13770, .F. ) ;
#5306 = DIRECTION ( 'NONE',  ( 0.000000000000000000, 5.223019709707975211E-21, -1.000000000000000000 ) ) ;
#5307 = FACE_OUTER_BOUND ( 'NONE', #18548, .T. ) ;
#5308 = ORIENTED_EDGE ( 'NONE', *, *, #21224, .T. ) ;
#5309 = DIRECTION ( 'NONE',  ( 0.000000000000000000, 0.000000000000000000, 1.000000000000000000 ) ) ;
#5310 = CARTESIAN_POINT ( 'NONE',  ( 1.833809397773803918, -29.99591688576986570, -141.9756687985007204 ) ) ;
#5311 = CARTESIAN_POINT ( 'NONE',  ( -1.045287976400383290, 12.68782741917383738, 44.00138577190627842 ) ) ;
#5312 = ORIENTED_EDGE ( 'NONE', *, *, #23726, .F. ) ;
#5313 = EDGE_LOOP ( 'NONE', ( #3446, #3300, #11572, #1170 ) ) ;
#5314 = CARTESIAN_POINT ( 'NONE',  ( -6.588769196390754423, -20.50531526814530636, 47.06982923582530276 ) ) ;
#5315 = EDGE_CURVE ( 'NONE', #16951, #27330, #4378, .T. ) ;
#5316 = CARTESIAN_POINT ( 'NONE',  ( 28.37603512858449406, -111.8384105897143570, 25.60641750873868361 ) ) ;
#5317 = CARTESIAN_POINT ( 'NONE',  ( 25.64681081121879203, 56.81519825470756047, 97.57530875170624540 ) ) ;
#5318 = CARTESIAN_POINT ( 'NONE',  ( -20.47566338032530808, 25.06314818626709240, 16.24827550219793437 ) ) ;
#5319 = CARTESIAN_POINT ( 'NONE',  ( 32.73300124599738581, 16.10546300444979195, -116.5274707358853163 ) ) ;
#5320 = ORIENTED_EDGE ( 'NONE', *, *, #11233, .F. ) ;
#5321 = CARTESIAN_POINT ( 'NONE',  ( 26.11404676487257603, 67.46175819463486789, -90.92995828888132337 ) ) ;
#5322 = CARTESIAN_POINT ( 'NONE',  ( 25.64708228042121618, -103.1656011680036045, 45.88917180166242815 ) ) ;
#5323 = CARTESIAN_POINT ( 'NONE',  ( 2.433796855181205476, -116.8607839509050734, -86.69855925934092511 ) ) ;
#5324 = ORIENTED_EDGE ( 'NONE', *, *, #13308, .T. ) ;
#5325 = EDGE_CURVE ( 'NONE', #24050, #14114, #18727, .T. ) ;
#5326 = ORIENTED_EDGE ( 'NONE', *, *, #8529, .T. ) ;
#5327 = FACE_OUTER_BOUND ( 'NONE', #24869, .T. ) ;
#5328 = EDGE_CURVE ( 'NONE', #8855, #17826, #9821, .T. ) ;
#5329 = CARTESIAN_POINT ( 'NONE',  ( -55.25719721206881729, 0.004044147484875269816, -0.01041086141212288138 ) ) ;
#5330 = DIRECTION ( 'NONE',  ( 1.000000000000000000, 0.000000000000000000, 0.000000000000000000 ) ) ;
#5331 = CARTESIAN_POINT ( 'NONE',  ( -8.786685647604889127, 9.545808661480615243, -52.67761315067287597 ) ) ;
#5332 = CARTESIAN_POINT ( 'NONE',  ( -8.259864102781676820, 6.590267880897663133, 52.60025989855196116 ) ) ;
#5333 = CARTESIAN_POINT ( 'NONE',  ( -1.049819825607609225, -45.79654196517396514, 0.5097917909113501844 ) ) ;
#5334 = ORIENTED_EDGE ( 'NONE', *, *, #16210, .T. ) ;
#5335 = DIRECTION ( 'NONE',  ( 0.5914120900931444380, 0.5455001977188090878, -0.5938529060132641257 ) ) ;
#5336 = CARTESIAN_POINT ( 'NONE',  ( 1.833485406944057594, 138.1714136985308699, 44.33323125129973619 ) ) ;
#5337 = CARTESIAN_POINT ( 'NONE',  ( 2.063896406836609909, -96.20114399516467074, 108.8509294491461787 ) ) ;
#5338 = EDGE_CURVE ( 'NONE', #24458, #13365, #8825, .T. ) ;
#5339 = B_SPLINE_CURVE_WITH_KNOTS ( 'NONE', 3,
 ( #14486, #16509, #6013, #16809, #12465, #10044, #3691, #27441 ),
 .UNSPECIFIED., .F., .F.,
 ( 4, 2, 2, 4 ),
 ( 6.938893903907228378E-18, 0.0002429588503611250624, 0.0004859177007222431860, 0.0009718354014444615437 ),
 .UNSPECIFIED. ) ;
#5340 = B_SPLINE_CURVE_WITH_KNOTS ( 'NONE', 3,
 ( #24711, #13735, #2508, #7420, #7146, #16037, #2360, #24841 ),
 .UNSPECIFIED., .F., .F.,
 ( 4, 2, 2, 4 ),
 ( 0.000000000000000000, 0.002761524886576648477, 0.005523049773153296954, 0.01104609954630659391 ),
 .UNSPECIFIED. ) ;
#5341 = CARTESIAN_POINT ( 'NONE',  ( 2.063896406836609909, -60.31174178979723166, -132.1577797566312142 ) ) ;
#5342 = CARTESIAN_POINT ( 'NONE',  ( 109.1592201516379674, -0.007051465909552739365, 0.003476928926134781935 ) ) ;
#5343 = CARTESIAN_POINT ( 'NONE',  ( -21.41430102051744555, 1.815007301162403497, 30.75470819672109002 ) ) ;
#5344 = ADVANCED_FACE ( 'NONE', ( #5790 ), #14703, .F. ) ;
#5345 = ORIENTED_EDGE ( 'NONE', *, *, #15749, .F. ) ;
#5346 = CARTESIAN_POINT ( 'NONE',  ( -55.24728320129491266, 0.01453410071985698077, 0.0006547948648746833647 ) ) ;
#5347 = ORIENTED_EDGE ( 'NONE', *, *, #17831, .T. ) ;
#5348 = B_SPLINE_CURVE_WITH_KNOTS ( 'NONE', 3,
 ( #4300, #17670, #4721, #4430, #13077, #2258, #13203 ),
 .UNSPECIFIED., .F., .F.,
 ( 4, 3, 4 ),
 ( 0.000000000000000000, 0.009512539173626427882, 0.02506242213020844906 ),
 .UNSPECIFIED. ) ;
#5349 = ORIENTED_EDGE ( 'NONE', *, *, #12105, .F. ) ;
#5350 = EDGE_LOOP ( 'NONE', ( #5684, #27566, #15298, #10978 ) ) ;
#5351 = DIRECTION ( 'NONE',  ( 1.000000000000000000, -6.938893903907226837E-18, 1.734723475976806709E-18 ) ) ;
#5352 = B_SPLINE_CURVE_WITH_KNOTS ( 'NONE', 3,
 ( #1614, #25948, #12275, #26077, #21191, #12405, #19180, #12826, #5815, #19042 ),
 .UNSPECIFIED., .F., .F.,
 ( 4, 3, 3, 4 ),
 ( 3.122502256758252770E-17, 0.0002669559177086221831, 0.0005339118354151072953, 0.001067817517169176392 ),
 .UNSPECIFIED. ) ;
#5353 = EDGE_CURVE ( 'NONE', #22045, #12390, #20737, .T. ) ;
#5354 = CARTESIAN_POINT ( 'NONE',  ( -1.048996300304498419, 43.78665266739856321, 13.42280206896931638 ) ) ;
#5355 = DIRECTION ( 'NONE',  ( 1.000000000000000000, -6.938893903907226837E-18, 1.734723475976806709E-18 ) ) ;
#5356 = FACE_OUTER_BOUND ( 'NONE', #17512, .T. ) ;
#5357 = CARTESIAN_POINT ( 'NONE',  ( 2.263178607246642660, -13.80342482180185115, 144.7392885066942654 ) ) ;
#5358 = CARTESIAN_POINT ( 'NONE',  ( -25.21435515916043713, 25.00736669481056751, 23.92354251275909505 ) ) ;
#5359 = ORIENTED_EDGE ( 'NONE', *, *, #19131, .F. ) ;
#5360 = CARTESIAN_POINT ( 'NONE',  ( 1.833691583653512369, 132.4191286035306518, 59.34641645332686011 ) ) ;
#5361 = EDGE_CURVE ( 'NONE', #1807, #27476, #9538, .T. ) ;
#5362 = CARTESIAN_POINT ( 'NONE',  ( 32.73300124599732186, 0.000000000000000000, 0.000000000000000000 ) ) ;
#5363 = CARTESIAN_POINT ( 'NONE',  ( -20.47566262905010248, 25.06314747784837138, -16.24827521404660047 ) ) ;
#5364 = CARTESIAN_POINT ( 'NONE',  ( 30.58324630866342275, -106.6567942264192368, -57.02364853894589203 ) ) ;
#5365 = ADVANCED_FACE ( 'NONE', ( #18589 ), #11063, .T. ) ;
#5366 = CARTESIAN_POINT ( 'NONE',  ( 13.36082413113063083, -9.660980093455732387, 152.6206443696328563 ) ) ;
#5367 = CARTESIAN_POINT ( 'NONE',  ( 109.1721716018069515, -0.01550977894511840725, -0.007126480965768139213 ) ) ;
#5368 = CARTESIAN_POINT ( 'NONE',  ( 32.73300124599737160, -89.94078864464117373, 75.82012867748450446 ) ) ;
#5369 = B_SPLINE_CURVE_WITH_KNOTS ( 'NONE', 3,
 ( #14910, #13169, #19233, #1804, #10604, #26001 ),
 .UNSPECIFIED., .F., .F.,
 ( 4, 2, 4 ),
 ( 0.000000000000000000, 0.0004335151646191511953, 0.0008670303292383023906 ),
 .UNSPECIFIED. ) ;
#5370 = CARTESIAN_POINT ( 'NONE',  ( 32.73300124599740002, 103.7392577722183660, -55.46353551261898218 ) ) ;
#5371 = CARTESIAN_POINT ( 'NONE',  ( 25.64699802086726521, 83.75009658924095390, -75.72889180797035635 ) ) ;
#5372 = ORIENTED_EDGE ( 'NONE', *, *, #17569, .F. ) ;
#5373 = DIRECTION ( 'NONE',  ( 0.5946245182733607137, 0.7999021332774030046, -0.08110646981858811444 ) ) ;
#5374 = ORIENTED_EDGE ( 'NONE', *, *, #10638, .F. ) ;
#5375 = CARTESIAN_POINT ( 'NONE',  ( -55.24340739397742794, -0.003826481709799693914, -0.009386184976285299672 ) ) ;
#5376 = CARTESIAN_POINT ( 'NONE',  ( 10.93730112725971715, 20.69552240458328995, 149.7554878793148703 ) ) ;
#5377 = ORIENTED_EDGE ( 'NONE', *, *, #15924, .T. ) ;
#5378 =( BOUNDED_SURFACE ( )  B_SPLINE_SURFACE ( 3, 1, ( 
 ( #4161, #12518 ),
 ( #1855, #8364 ),
 ( #25644, #28331 ),
 ( #15088, #23907 ) ),
 .UNSPECIFIED., .F., .F., .F. ) 
 B_SPLINE_SURFACE_WITH_KNOTS ( ( 4, 4 ),
 ( 2, 2 ),
 ( 0.000000000000000000, 1.000000000000000000 ),
 ( 0.000000000000000000, 1.000000000000000000 ),
 .UNSPECIFIED. ) 
 GEOMETRIC_REPRESENTATION_ITEM ( )  RATIONAL_B_SPLINE_SURFACE ( (
 ( 1.000000000000000000, 1.000000000000000000),
 ( 0.9934239774497837239, 0.8357310067453919133),
 ( 0.9934239774497837239, 0.8357310067453919133),
 ( 1.000000000000000000, 1.000000000000000000) ) ) 
 REPRESENTATION_ITEM ( '' )  SURFACE ( )  );
#5379 = VERTEX_POINT ( 'NONE', #16428 ) ;
#5380 = VERTEX_POINT ( 'NONE', #1304 ) ;
#5381 = VERTEX_POINT ( 'NONE', #3754 ) ;
#5382 = FACE_OUTER_BOUND ( 'NONE', #19250, .T. ) ;
#5383 = CARTESIAN_POINT ( 'NONE',  ( 1.833485406944043827, 85.72460230293849293, -117.0814567582535659 ) ) ;
#5384 = B_SPLINE_CURVE_WITH_KNOTS ( 'NONE', 3,
 ( #13693, #14117, #462, #18006 ),
 .UNSPECIFIED., .F., .F.,
 ( 4, 4 ),
 ( 9.837579971998123693E-17, 0.008383748772659571635 ),
 .UNSPECIFIED. ) ;
#5385 = CARTESIAN_POINT ( 'NONE',  ( -55.24728320129491266, -0.01362040845703012606, 0.005114031043466422087 ) ) ;
#5386 = B_SPLINE_CURVE_WITH_KNOTS ( 'NONE', 3,
 ( #2410, #18101, #13348, #8920, #11346, #2855, #125, #11481, #17677, #26456 ),
 .UNSPECIFIED., .F., .F.,
 ( 4, 3, 3, 4 ),
 ( 0.000000000000000000, 0.0002669560319015801698, 0.0005492286108966397190, 0.0008315040496093522703 ),
 .UNSPECIFIED. ) ;
#5387 = CARTESIAN_POINT ( 'NONE',  ( -5.986830583229487246, 49.46736940480273859, 11.27873876172089851 ) ) ;
#5388 = CARTESIAN_POINT ( 'NONE',  ( 19.66333377628710366, -137.6761449113042772, -4.491394265033680000 ) ) ;
#5389 = CARTESIAN_POINT ( 'NONE',  ( 2.433796855181205476, -137.9325382748282038, -46.34326152018883249 ) ) ;
#5390 = CARTESIAN_POINT ( 'NONE',  ( 109.1589550718175161, -0.001354998915253822220, 0.007453082872782193502 ) ) ;
#5391 = CARTESIAN_POINT ( 'NONE',  ( 1.831572820252008738, -43.90210991190526357, -138.3111855986065564 ) ) ;
#5392 = EDGE_CURVE ( 'NONE', #10557, #26958, #11936, .T. ) ;
#5393 = CARTESIAN_POINT ( 'NONE',  ( -20.20700224038492721, 18.19058640100257662, 23.35150625415638714 ) ) ;
#5395 = CARTESIAN_POINT ( 'NONE',  ( -1.046936909428682894, -15.35929614323696413, -43.14407378092988665 ) ) ;
#5394 = CARTESIAN_POINT ( 'NONE',  ( -1.058473599757822292, -44.07591602137166831, -12.47539220917846237 ) ) ;
#5396 = LINE ( 'NONE', #10313, #12456 ) ;
#5398 = EDGE_LOOP ( 'NONE', ( #4048, #7638, #27241, #563 ) ) ;
#5397 = EDGE_CURVE ( 'NONE', #9920, #1176, #16111, .T. ) ;
#5399 = ORIENTED_EDGE ( 'NONE', *, *, #2654, .F. ) ;
#5400 = CARTESIAN_POINT ( 'NONE',  ( 32.73300124599739291, -99.90245962373785460, -62.10906484417343165 ) ) ;
#5402 = CARTESIAN_POINT ( 'NONE',  ( 1.831572820252009626, 126.1609924456730170, 71.69925593429853450 ) ) ;
#5401 = CARTESIAN_POINT ( 'NONE',  ( 2.433796855181205476, -16.65276281464661423, 144.5536872373191102 ) ) ;
#5403 = EDGE_CURVE ( 'NONE', #19868, #20968, #1802, .T. ) ;
#5404 = CARTESIAN_POINT ( 'NONE',  ( 32.73300124599738581, -32.68291970228155918, -113.0038235389605461 ) ) ;
#5405 = CYLINDRICAL_SURFACE ( 'NONE', #5125, 12.50000000000000178 ) ;
#5406 = ORIENTED_EDGE ( 'NONE', *, *, #7093, .T. ) ;
#5407 = EDGE_LOOP ( 'NONE', ( #19419, #8984, #23779, #16565 ) ) ;
#5408 = CARTESIAN_POINT ( 'NONE',  ( -12.82751273423880711, 35.32125660155448088, -33.78816682541299343 ) ) ;
#5409 = CARTESIAN_POINT ( 'NONE',  ( 9.884929003653608603, 42.50195158091032965, 144.4113244745773272 ) ) ;
#5410 = CARTESIAN_POINT ( 'NONE',  ( 16.75465622695650936, -138.0797984721905323, -34.09043808962561428 ) ) ;
#5411 = ORIENTED_EDGE ( 'NONE', *, *, #11379, .F. ) ;
#5412 = CARTESIAN_POINT ( 'NONE',  ( 25.64708010899964208, -97.75667227735131348, 56.50300922386559677 ) ) ;
#5413 = DIRECTION ( 'NONE',  ( -1.000000000000000000, -0.000000000000000000, -0.000000000000000000 ) ) ;
#5414 =( BOUNDED_SURFACE ( )  B_SPLINE_SURFACE ( 3, 1, ( 
 ( #12555, #17160 ),
 ( #10695, #23806 ),
 ( #12829, #19461 ),
 ( #19047, #6799 ) ),
 .UNSPECIFIED., .F., .F., .F. ) 
 B_SPLINE_SURFACE_WITH_KNOTS ( ( 4, 4 ),
 ( 2, 2 ),
 ( 0.000000000000000000, 1.000000000000000000 ),
 ( 0.000000000000000000, 1.000000000000000000 ),
 .UNSPECIFIED. ) 
 GEOMETRIC_REPRESENTATION_ITEM ( )  RATIONAL_B_SPLINE_SURFACE ( (
 ( 1.000000000000000000, 1.000000000000000000),
 ( 0.6386103224230316178, 0.9954351624131538845),
 ( 0.6386103224230316178, 0.9954351624131538845),
 ( 1.000000000000000000, 1.000000000000000000) ) ) 
 REPRESENTATION_ITEM ( '' )  SURFACE ( )  );
#5415 = ORIENTED_EDGE ( 'NONE', *, *, #13652, .T. ) ;
#5416 = CARTESIAN_POINT ( 'NONE',  ( 1.832998868059890096, -44.33343224355141388, -138.1720401012271395 ) ) ;
#5417 = EDGE_LOOP ( 'NONE', ( #24930, #14170, #8406, #17374 ) ) ;
#5418 = CARTESIAN_POINT ( 'NONE',  ( 25.73574536432414916, -45.21157800100239399, -103.5288236655400027 ) ) ;
#5419 = DIRECTION ( 'NONE',  ( 0.5946245182733607137, -0.1642747008466192427, -0.7870422510449660569 ) ) ;
#5420 = ORIENTED_EDGE ( 'NONE', *, *, #14588, .F. ) ;
#5421 = APPLICATION_PROTOCOL_DEFINITION ( 'draft international standard', 'automotive_design', 1998, #4206 ) ;
#5422 = EDGE_CURVE ( 'NONE', #6247, #25314, #2838, .T. ) ;
#5423 = CARTESIAN_POINT ( 'NONE',  ( -28.13707043255157103, -18.96624908365836859, 12.83104814250474668 ) ) ;
#5424 = CARTESIAN_POINT ( 'NONE',  ( -1.049819825607590351, 14.63675055554442395, 43.39756533277866879 ) ) ;
#5425 = CARTESIAN_POINT ( 'NONE',  ( 109.1592201516379674, -0.007376275279032879113, 0.002720803050370542309 ) ) ;
#5426 = CARTESIAN_POINT ( 'NONE',  ( 1.833838850855475044, -107.7780290788690536, -97.16351016226002457 ) ) ;
#5427 = EDGE_CURVE ( 'NONE', #20744, #25928, #8369, .T. ) ;
#5428 = ORIENTED_EDGE ( 'NONE', *, *, #4354, .T. ) ;
#5429 = FACE_OUTER_BOUND ( 'NONE', #17472, .T. ) ;
#5431 = CARTESIAN_POINT ( 'NONE',  ( -1.045287976400365970, -45.76855895860942525, 1.530335034934587002 ) ) ;
#5430 = CARTESIAN_POINT ( 'NONE',  ( -55.24300891470648622, -0.003362556190414485880, 0.009225237711097986765 ) ) ;
#5432 = CARTESIAN_POINT ( 'NONE',  ( 28.37644542392845892, -17.02293047611445687, 123.1691345231581352 ) ) ;
#5433 = ORIENTED_EDGE ( 'NONE', *, *, #25952, .T. ) ;
#5434 = ORIENTED_EDGE ( 'NONE', *, *, #23124, .T. ) ;
#5435 = EDGE_LOOP ( 'NONE', ( #27746, #3405, #4411, #4175 ) ) ;
#5436 = CARTESIAN_POINT ( 'NONE',  ( 10.93730112725996406, 10.89264110825190457, -150.7858122213661716 ) ) ;
#5437 = CARTESIAN_POINT ( 'NONE',  ( -1.619063947482201282, 11.94059994246159384, -44.80407745103787676 ) ) ;
#5439 = LINE ( 'NONE', #8727, #4055 ) ;
#5438 = DIRECTION ( 'NONE',  ( -1.000000000000000000, -0.000000000000000000, -0.000000000000000000 ) ) ;
#5440 = CARTESIAN_POINT ( 'NONE',  ( 26.11404676487257603, -110.9778746459745520, -22.43340081644882389 ) ) ;
#5441 = CARTESIAN_POINT ( 'NONE',  ( -8.786685647604890903, 37.00619870957935120, -38.68584556812312059 ) ) ;
#5442 = CARTESIAN_POINT ( 'NONE',  ( -28.41354790283022069, -18.00456980371910376, -14.62505768302794529 ) ) ;
#5443 = CARTESIAN_POINT ( 'NONE',  ( -1.239374126674604337, -35.79060836339793639, 28.97829083655478399 ) ) ;
#5444 = ORIENTED_EDGE ( 'NONE', *, *, #9030, .F. ) ;
#5445 = CARTESIAN_POINT ( 'NONE',  ( 19.66333377628716406, -129.5498775999581085, -46.81583828063196506 ) ) ;
#5446 = CARTESIAN_POINT ( 'NONE',  ( 109.1592201516379674, -0.006044422199831509662, -0.005027640251764362717 ) ) ;
#5447 = CARTESIAN_POINT ( 'NONE',  ( 25.64681081121879203, 110.3564950173081769, 23.88203588908119457 ) ) ;
#5448 = CARTESIAN_POINT ( 'NONE',  ( 109.1586059443104944, -0.003774052605959072812, 0.005983234375919664789 ) ) ;
#5449 = CARTESIAN_POINT ( 'NONE',  ( -55.24728320129491266, -0.01137345571546789259, 0.009072670231975133240 ) ) ;
#5450 = FACE_BOUND ( 'NONE', #15960, .T. ) ;
#5451 = B_SPLINE_CURVE_WITH_KNOTS ( 'NONE', 3,
 ( #22097, #11165, #11732, #17772 ),
 .UNSPECIFIED., .F., .F.,
 ( 4, 4 ),
 ( 0.000000000000000000, 0.01077107196513816395 ),
 .UNSPECIFIED. ) ;
#5452 = CARTESIAN_POINT ( 'NONE',  ( -1.045287976400365970, -25.66401692419961833, 37.92705037016786918 ) ) ;
#5453 = ORIENTED_EDGE ( 'NONE', *, *, #1726, .T. ) ;
#5454 = B_SPLINE_CURVE_WITH_KNOTS ( 'NONE', 3,
 ( #12074, #27596, #986, #27014, #7327, #12212, #14358, #3009, #1263, #22888 ),
 .UNSPECIFIED., .F., .F.,
 ( 4, 3, 3, 4 ),
 ( 0.000000000000000000, 0.0002669560319015888434, 0.0005492286108966463326, 0.0008315040496093561734 ),
 .UNSPECIFIED. ) ;
#5455 = CARTESIAN_POINT ( 'NONE',  ( 2.108985857320942348, 28.95357181521022127, -142.3791757917249186 ) ) ;
#5456 = CARTESIAN_POINT ( 'NONE',  ( -18.41936578851711204, 41.75701384111740566, -7.566034416290932541 ) ) ;
#5457 = CARTESIAN_POINT ( 'NONE',  ( -1.044557008772713624, 12.57891310333411106, 44.03203053429556491 ) ) ;
#5458 = VERTEX_POINT ( 'NONE', #12666 ) ;
#5459 = ORIENTED_EDGE ( 'NONE', *, *, #8113, .T. ) ;
#5460 = CARTESIAN_POINT ( 'NONE',  ( -55.24198130335446422, -0.006617369590171728877, 0.006527480770973505091 ) ) ;
#5461 = CONICAL_SURFACE ( 'NONE', #12812, 34.60786435723138510, 0.8559913436420825139 ) ;
#5462 = EDGE_CURVE ( 'NONE', #24670, #15546, #11991, .T. ) ;
#5463 = CARTESIAN_POINT ( 'NONE',  ( -1.048171036023512803, -15.11933492062798656, 43.23005599774316465 ) ) ;
#5464 = ADVANCED_FACE ( 'NONE', ( #13090 ), #11597, .F. ) ;
#5465 = CARTESIAN_POINT ( 'NONE',  ( 25.64681081121880624, -23.88203588908156760, 110.3564950173080916 ) ) ;
#5466 = CARTESIAN_POINT ( 'NONE',  ( 25.69398547355840989, 97.43788956976230509, -57.11291030433552152 ) ) ;
#5467 = ORIENTED_EDGE ( 'NONE', *, *, #11247, .T. ) ;
#5468 = CARTESIAN_POINT ( 'NONE',  ( 1.893872463202055600, -144.4512189534318622, 14.22435552397961978 ) ) ;
#5469 = EDGE_CURVE ( 'NONE', #25788, #1690, #25325, .T. ) ;
#5470 = B_SPLINE_CURVE_WITH_KNOTS ( 'NONE', 3,
 ( #5150, #12475, #5740, #3979 ),
 .UNSPECIFIED., .F., .F.,
 ( 4, 4 ),
 ( 1.877672896018868361E-16, 0.001982023823822947652 ),
 .UNSPECIFIED. ) ;
#5471 = CARTESIAN_POINT ( 'NONE',  ( 25.64704443564076541, 34.76451658509533615, 107.4261196778963949 ) ) ;
#5472 = CARTESIAN_POINT ( 'NONE',  ( 1.833485406944057594, -45.34878176254139248, -137.8414413349090637 ) ) ;
#5473 = ORIENTED_EDGE ( 'NONE', *, *, #8645, .F. ) ;
#5474 = ORIENTED_EDGE ( 'NONE', *, *, #13305, .T. ) ;
#5475 = ORIENTED_EDGE ( 'NONE', *, *, #12024, .F. ) ;
#5476 = CARTESIAN_POINT ( 'NONE',  ( -55.24728320129491266, -0.01214321324516726489, -0.008013189884950557701 ) ) ;
#5477 = CARTESIAN_POINT ( 'NONE',  ( 1.833206308920100724, 107.3376449983727809, 97.64934899952737624 ) ) ;
#5478 = CARTESIAN_POINT ( 'NONE',  ( 25.64681081121879203, 56.09509703373481670, -97.99105938547863559 ) ) ;
#5479 = CARTESIAN_POINT ( 'NONE',  ( -1.539760825549692180, 11.93465943778514315, -44.72358953107736568 ) ) ;
#5480 = CARTESIAN_POINT ( 'NONE',  ( -5.986830583229484581, 4.559539818181838733, 50.53158596890435916 ) ) ;
#5481 = CARTESIAN_POINT ( 'NONE',  ( 24.22246935314087324, -90.00000000000005684, 39.99999999999997158 ) ) ;
#5482 = EDGE_LOOP ( 'NONE', ( #2793, #22821 ) ) ;
#5483 = CARTESIAN_POINT ( 'NONE',  ( 2.433796855181233454, 43.58222566461826375, -138.8296532063083646 ) ) ;
#5484 = CARTESIAN_POINT ( 'NONE',  ( -25.21435515916025594, 1.749597353048488237E-16, -4.373993382621220594E-17 ) ) ;
#5485 = DIRECTION ( 'NONE',  ( -1.000000000000000000, -0.000000000000000000, -0.000000000000000000 ) ) ;
#5486 = CARTESIAN_POINT ( 'NONE',  ( 26.11404676487259024, -45.01677474591480888, 103.8885755249567922 ) ) ;
#5487 = CARTESIAN_POINT ( 'NONE',  ( 109.1592201516379674, 0.004194960840980690650, -0.006649399203953405661 ) ) ;
#5488 = CARTESIAN_POINT ( 'NONE',  ( 25.64708010899963853, -75.51173009720581319, 83.94602815988648103 ) ) ;
#5489 = CARTESIAN_POINT ( 'NONE',  ( -8.786685647604890903, 47.14957014837354876, -25.35688121747519119 ) ) ;
#5490 = VERTEX_POINT ( 'NONE', #4031 ) ;
#5491 = ORIENTED_EDGE ( 'NONE', *, *, #6775, .T. ) ;
#5492 = ORIENTED_EDGE ( 'NONE', *, *, #23041, .T. ) ;
#5493 = EDGE_CURVE ( 'NONE', #7441, #1461, #23461, .T. ) ;
#5494 = CARTESIAN_POINT ( 'NONE',  ( -4.473127245936434626, 18.25038884639934977, 45.82513704981523972 ) ) ;
#5495 = CARTESIAN_POINT ( 'NONE',  ( 19.66333377628679813, -108.7423656420555460, -84.55762186019691740 ) ) ;
#5496 = EDGE_CURVE ( 'NONE', #17315, #8356, #15668, .T. ) ;
#5497 = B_SPLINE_CURVE_WITH_KNOTS ( 'NONE', 3,
 ( #8483, #17245, #24167, #28181, #4426, #13073, #11056, #2399, #19549, #14942 ),
 .UNSPECIFIED., .F., .F.,
 ( 4, 3, 3, 4 ),
 ( 2.775557561562891351E-17, 0.0002669559177086104737, 0.0005339118354150823587, 0.001067817517169155576 ),
 .UNSPECIFIED. ) ;
#5498 = FACE_OUTER_BOUND ( 'NONE', #1629, .T. ) ;
#5499 = CARTESIAN_POINT ( 'NONE',  ( 8.186469777910884815, -143.0750864738775192, -42.84118569629491446 ) ) ;
#5500 = EDGE_CURVE ( 'NONE', #22518, #21826, #2270, .T. ) ;
#5501 = B_SPLINE_CURVE_WITH_KNOTS ( 'NONE', 3,
 ( #18069, #20220, #27129, #5262, #24724, #7014 ),
 .UNSPECIFIED., .F., .F.,
 ( 4, 2, 4 ),
 ( 3.689388176052398149E-16, 0.003576372551511164399, 0.007152745103021965374 ),
 .UNSPECIFIED. ) ;
#5502 = CARTESIAN_POINT ( 'NONE',  ( -20.37983603106074426, -28.74620395171555742, 7.753708011498863684 ) ) ;
#5503 = CARTESIAN_POINT ( 'NONE',  ( -20.20700224038492721, 23.35150625415659320, -18.19058640100232438 ) ) ;
#5504 = CARTESIAN_POINT ( 'NONE',  ( -20.21097721650785672, 17.13687097598137399, -24.14932365326959030 ) ) ;
#5505 = CARTESIAN_POINT ( 'NONE',  ( 60.46576798286869803, -12.50000000000000000, 1.048913872128491071E-16 ) ) ;
#5506 = CARTESIAN_POINT ( 'NONE',  ( 1.833485406944043827, -59.50871042846314651, 132.3460930279889567 ) ) ;
#5507 = CARTESIAN_POINT ( 'NONE',  ( 109.1586900883932856, -0.004701023939945749193, 0.005371970278528625728 ) ) ;
#5508 = CARTESIAN_POINT ( 'NONE',  ( -20.20997486282892552, 0.3303599360442536770, 29.60348406988233450 ) ) ;
#5509 = CARTESIAN_POINT ( 'NONE',  ( -1.464342487929864323, -25.15873223207664466, 38.76467504336611114 ) ) ;
#5510 = B_SPLINE_CURVE_WITH_KNOTS ( 'NONE', 3,
 ( #24252, #24830, #6985, #11146, #9556, #5086, #11425, #22521 ),
 .UNSPECIFIED., .F., .F.,
 ( 4, 2, 2, 4 ),
 ( 1.430489624538199204E-17, 0.0002429588503611245745, 0.0004859177007222348376, 0.0009718354014444673984 ),
 .UNSPECIFIED. ) ;
#5511 = CARTESIAN_POINT ( 'NONE',  ( 9.884929003653608603, 148.0628878137283948, -27.17402761732198613 ) ) ;
#5512 = CARTESIAN_POINT ( 'NONE',  ( -1.539763995773681504, 35.94321074656937753, 29.16712963492422617 ) ) ;
#5513 = CARTESIAN_POINT ( 'NONE',  ( -28.41354790283022069, -19.47297445639540214, 12.60397206714853624 ) ) ;
#5514 = CARTESIAN_POINT ( 'NONE',  ( -1.031422197589716205, -45.78027046666443312, 1.530725436377931237 ) ) ;
#5515 = CARTESIAN_POINT ( 'NONE',  ( -6.588769196390764193, -11.07780292579730208, -50.13301368233293687 ) ) ;
#5516 = ORIENTED_EDGE ( 'NONE', *, *, #6111, .F. ) ;
#5517 = CARTESIAN_POINT ( 'NONE',  ( -1.155031165708886087, 25.28071330859886245, -38.31525684316149949 ) ) ;
#5518 = VERTEX_POINT ( 'NONE', #8634 ) ;
#5519 = CARTESIAN_POINT ( 'NONE',  ( -1.019300379054419947, -16.06793277091962935, 42.90269154183443590 ) ) ;
#5520 = ORIENTED_EDGE ( 'NONE', *, *, #14428, .T. ) ;
#5521 = VECTOR ( 'NONE', #13446, 1000.000000000000114 ) ;
#5522 = ORIENTED_EDGE ( 'NONE', *, *, #9562, .F. ) ;
#5523 = VERTEX_POINT ( 'NONE', #17264 ) ;
#5524 = ADVANCED_FACE ( 'NONE', ( #21736 ), #21354, .F. ) ;
#5525 = EDGE_CURVE ( 'NONE', #19015, #5056, #2156, .T. ) ;
#5526 = CARTESIAN_POINT ( 'NONE',  ( 1.831572820252008738, 59.92262167723615107, -132.1614873090342712 ) ) ;
#5527 = CIRCLE ( 'NONE', #6001, 151.1787379149930359 ) ;
#5528 = EDGE_CURVE ( 'NONE', #15977, #13981, #22155, .T. ) ;
#5529 = CARTESIAN_POINT ( 'NONE',  ( -18.41936578851711204, 41.75701384111740566, -7.566034416290932541 ) ) ;
#5530 = ADVANCED_FACE ( 'NONE', ( #11214, #2419 ), #11793, .T. ) ;
#5531 = FACE_OUTER_BOUND ( 'NONE', #11258, .T. ) ;
#5532 = CARTESIAN_POINT ( 'NONE',  ( -12.94347594948481195, -43.91326021875530472, -21.16159467081338263 ) ) ;
#5533 = AXIS2_PLACEMENT_3D ( 'NONE', #13930, #13642, #20259 ) ;
#5534 =( BOUNDED_SURFACE ( )  B_SPLINE_SURFACE ( 3, 1, ( 
 ( #10981, #4209 ),
 ( #13128, #4486 ),
 ( #8823, #17860 ),
 ( #4785, #21779 ) ),
 .UNSPECIFIED., .F., .F., .F. ) 
 B_SPLINE_SURFACE_WITH_KNOTS ( ( 4, 4 ),
 ( 2, 2 ),
 ( 0.000000000000000000, 1.000000000000000000 ),
 ( 0.000000000000000000, 1.000000000000000000 ),
 .UNSPECIFIED. ) 
 GEOMETRIC_REPRESENTATION_ITEM ( )  RATIONAL_B_SPLINE_SURFACE ( (
 ( 1.000000000000000000, 1.000000000000000000),
 ( 0.9960225298536222738, 0.9999952330161893110),
 ( 0.9960225298536222738, 0.9999952330161893110),
 ( 1.000000000000000000, 1.000000000000000000) ) ) 
 REPRESENTATION_ITEM ( '' )  SURFACE ( )  );
#5535 = CARTESIAN_POINT ( 'NONE',  ( 25.86096068574580542, 35.88291140784058797, -107.2082119295148459 ) ) ;
#5536 = CARTESIAN_POINT ( 'NONE',  ( 109.1586900883932856, -0.002109621908824192878, -0.006819617742892434241 ) ) ;
#5537 = CARTESIAN_POINT ( 'NONE',  ( 1.833485406944043827, -58.53321471326791681, -132.7804117027893938 ) ) ;
#5538 = CONICAL_SURFACE ( 'NONE', #1415, 34.60786435723138510, 0.8559913436420825139 ) ;
#5539 = CARTESIAN_POINT ( 'NONE',  ( 10.93730112725945602, 104.7670965581007607, 108.9902118373744742 ) ) ;
#5540 = CARTESIAN_POINT ( 'NONE',  ( 8.186469829614269500, -131.0413692472658340, 71.65198613712934161 ) ) ;
#5541 = AXIS2_PLACEMENT_3D ( 'NONE', #10677, #19446, #28215 ) ;
#5542 = ORIENTED_EDGE ( 'NONE', *, *, #8750, .F. ) ;
#5543 = VERTEX_POINT ( 'NONE', #6907 ) ;
#5544 = CARTESIAN_POINT ( 'NONE',  ( 55.49584447822657296, 42.42793568433036455, -58.85239198729144761 ) ) ;
#5546 = CARTESIAN_POINT ( 'NONE',  ( 26.11404676487257603, 57.58742681967585497, -97.48350837663548418 ) ) ;
#5545 = CARTESIAN_POINT ( 'NONE',  ( -55.24390624410018802, 0.01027195578987812573, -0.001811362924359468263 ) ) ;
#5547 = CARTESIAN_POINT ( 'NONE',  ( 8.186469829614233973, 12.15801983495625116, 148.8557359502361805 ) ) ;
#5548 = CARTESIAN_POINT ( 'NONE',  ( -20.20700224038492365, 8.199606986804329978, -28.44216453106539078 ) ) ;
#5549 = CARTESIAN_POINT ( 'NONE',  ( -1.045287976400383290, -36.12803364096628655, -28.14015102489793918 ) ) ;
#5550 =( BOUNDED_SURFACE ( )  B_SPLINE_SURFACE ( 3, 1, ( 
 ( #18585, #11823 ),
 ( #18723, #27641 ),
 ( #7665, #872 ),
 ( #16424, #7516 ) ),
 .UNSPECIFIED., .F., .F., .F. ) 
 B_SPLINE_SURFACE_WITH_KNOTS ( ( 4, 4 ),
 ( 2, 2 ),
 ( 0.000000000000000000, 1.000000000000000000 ),
 ( 0.000000000000000000, 1.000000000000000000 ),
 .UNSPECIFIED. ) 
 GEOMETRIC_REPRESENTATION_ITEM ( )  RATIONAL_B_SPLINE_SURFACE ( (
 ( 1.000000000000000000, 1.000000000000000000),
 ( 0.9956975270656954757, 0.8568959468854893125),
 ( 0.9956975270656954757, 0.8568959468854893125),
 ( 1.000000000000000000, 1.000000000000000000) ) ) 
 REPRESENTATION_ITEM ( '' )  SURFACE ( )  );
#5551 = ORIENTED_EDGE ( 'NONE', *, *, #3227, .F. ) ;
#5552 = CARTESIAN_POINT ( 'NONE',  ( 1.833206310202339262, 137.7753867363983886, -45.54896489827011408 ) ) ;
#5553 = CARTESIAN_POINT ( 'NONE',  ( 109.1586900883932856, -0.007109207791181747921, 0.0006456433529163188882 ) ) ;
#5554 = CARTESIAN_POINT ( 'NONE',  ( 32.73300124599738581, -114.2056417606545864, -28.19767303745721065 ) ) ;
#5555 = VERTEX_POINT ( 'NONE', #2566 ) ;
#5556 = CARTESIAN_POINT ( 'NONE',  ( 25.64703792032469920, -97.70949518026544922, 56.58441811305572600 ) ) ;
#5557 = CARTESIAN_POINT ( 'NONE',  ( -1.323439229708138987, -28.92147054731866263, -35.86372896917463038 ) ) ;
#5558 = ORIENTED_EDGE ( 'NONE', *, *, #3935, .T. ) ;
#5559 = AXIS2_PLACEMENT_3D ( 'NONE', #5985, #4372, #19622 ) ;
#5560 = AXIS2_PLACEMENT_3D ( 'NONE', #13218, #6341, #19567 ) ;
#5561 = AXIS2_PLACEMENT_3D ( 'NONE', #5579, #3420, #12201 ) ;
#5562 = EDGE_CURVE ( 'NONE', #9016, #4553, #23159, .T. ) ;
#5563 = CONICAL_SURFACE ( 'NONE', #16155, 117.6351876552689504, 0.9945805576725580410 ) ;
#5564 = ORIENTED_EDGE ( 'NONE', *, *, #15708, .T. ) ;
#5565 = CARTESIAN_POINT ( 'NONE',  ( -55.24300891470650754, -0.009812809446892518245, 0.0003472257464213444889 ) ) ;
#5566 = AXIS2_PLACEMENT_3D ( 'NONE', #21566, #24299, #4143 ) ;
#5567 = VERTEX_POINT ( 'NONE', #22748 ) ;
#5568 = ADVANCED_FACE ( 'NONE', ( #24469 ), #22636, .F. ) ;
#5569 = CARTESIAN_POINT ( 'NONE',  ( 109.1592201516379674, -0.005485778713193788063, 0.005631912476305676526 ) ) ;
#5570 = EDGE_CURVE ( 'NONE', #2039, #5567, #20371, .T. ) ;
#5571 = CARTESIAN_POINT ( 'NONE',  ( -1.019300379054419725, 38.21680004809200426, 25.26451264419602438 ) ) ;
#5572 = B_SPLINE_CURVE_WITH_KNOTS ( 'NONE', 3,
 ( #4047, #10683, #28353, #19035 ),
 .UNSPECIFIED., .F., .F.,
 ( 4, 4 ),
 ( 2.081668171172168513E-17, 0.008383748772659471021 ),
 .UNSPECIFIED. ) ;
#5573 = CARTESIAN_POINT ( 'NONE',  ( 2.108985857320932578, -118.2933707022552454, -84.36123201973929042 ) ) ;
#5574 = CARTESIAN_POINT ( 'NONE',  ( 16.75465622695635659, 133.7599617830029217, 48.33695624543378244 ) ) ;
#5575 = ORIENTED_EDGE ( 'NONE', *, *, #19307, .F. ) ;
#5576 = CARTESIAN_POINT ( 'NONE',  ( -1.050231094221201644, -13.91061116148162391, 43.63617436699752261 ) ) ;
#5578 = CARTESIAN_POINT ( 'NONE',  ( -1.050230346682676785, 43.55772679531850855, -14.15203301556446647 ) ) ;
#5577 = CARTESIAN_POINT ( 'NONE',  ( 10.93730112725945425, 115.5857507957700818, 97.44200844886312041 ) ) ;
#5579 = CARTESIAN_POINT ( 'NONE',  ( 24.22246935314087324, 0.000000000000000000, 0.000000000000000000 ) ) ;
#5580 = ORIENTED_EDGE ( 'NONE', *, *, #21590, .F. ) ;
#5581 = VECTOR ( 'NONE', #2765, 1000.000000000000000 ) ;
#5582 = VERTEX_POINT ( 'NONE', #20126 ) ;
#5583 = EDGE_LOOP ( 'NONE', ( #2105, #17997, #7562, #2166 ) ) ;
#5584 = AXIS2_PLACEMENT_3D ( 'NONE', #16241, #25047, #20696 ) ;
#5585 = CARTESIAN_POINT ( 'NONE',  ( -55.24390624410018802, -0.007503127514281482044, 0.007245494385991411469 ) ) ;
#5586 = DIRECTION ( 'NONE',  ( 0.5914120900931444380, 0.8027508043202539190, -0.07630783613000559351 ) ) ;
#5588 = CARTESIAN_POINT ( 'NONE',  ( 10.93730112726006176, 142.1801301103792809, -51.37919228020152929 ) ) ;
#5587 = CARTESIAN_POINT ( 'NONE',  ( -20.20700224038492721, -24.51628800869035274, 16.58740185276737122 ) ) ;
#5589 = VECTOR ( 'NONE', #15372, 1000.000000000000000 ) ;
#5590 = CARTESIAN_POINT ( 'NONE',  ( -55.24340739397742084, 0.005344433640973447058, 0.008612749836246493332 ) ) ;
#5591 = DIRECTION ( 'NONE',  ( -1.000000000000000000, 0.000000000000000000, 0.000000000000000000 ) ) ;
#5592 = VERTEX_POINT ( 'NONE', #559 ) ;
#5593 = CARTESIAN_POINT ( 'NONE',  ( 1.833750490713684123, 107.6587173638747146, 97.29556423840173807 ) ) ;
#5594 = DIRECTION ( 'NONE',  ( 0.000000000000000000, 0.000000000000000000, -1.000000000000000000 ) ) ;
#5595 = ORIENTED_EDGE ( 'NONE', *, *, #13654, .T. ) ;
#5596 = CARTESIAN_POINT ( 'NONE',  ( 8.186469777910868828, -137.8131828745823668, -57.56191611950443843 ) ) ;
#5597 = CARTESIAN_POINT ( 'NONE',  ( -20.57838717382308147, -23.26537097894090778, 18.89542499756525729 ) ) ;
#5599 = CONICAL_SURFACE ( 'NONE', #1462, 117.6351876552689504, 0.9945805576725580410 ) ;
#5598 =( BOUNDED_SURFACE ( )  B_SPLINE_SURFACE ( 3, 1, ( 
 ( #24958, #9113 ),
 ( #22060, #4800 ),
 ( #22219, #24820 ),
 ( #6971, #19905 ) ),
 .UNSPECIFIED., .F., .F., .F. ) 
 B_SPLINE_SURFACE_WITH_KNOTS ( ( 4, 4 ),
 ( 2, 2 ),
 ( 0.000000000000000000, 1.000000000000000000 ),
 ( 0.000000000000000000, 1.000000000000000000 ),
 .UNSPECIFIED. ) 
 GEOMETRIC_REPRESENTATION_ITEM ( )  RATIONAL_B_SPLINE_SURFACE ( (
 ( 1.000000000000000000, 1.000000000000000000),
 ( 0.6386103224230302855, 0.9954351624131538845),
 ( 0.6386103224230302855, 0.9954351624131538845),
 ( 1.000000000000000000, 1.000000000000000000) ) ) 
 REPRESENTATION_ITEM ( '' )  SURFACE ( )  );
#5600 = CARTESIAN_POINT ( 'NONE',  ( 109.1624594426973260, -0.009004164758061298027, -0.01318243916934112685 ) ) ;
#5601 = LINE ( 'NONE', #16242, #7299 ) ;
#5602 = CARTESIAN_POINT ( 'NONE',  ( -8.786685647604896232, 52.67761315067299677, 9.545808661480061019 ) ) ;
#5603 = CARTESIAN_POINT ( 'NONE',  ( 25.73574536432414916, -110.6664861019685873, 22.69874377039401381 ) ) ;
#5604 = CARTESIAN_POINT ( 'NONE',  ( 32.73300124599738581, 39.98094346392455378, -110.6325518752269517 ) ) ;
#5605 = VERTEX_POINT ( 'NONE', #18109 ) ;
#5606 = CARTESIAN_POINT ( 'NONE',  ( 16.75465622695653423, 62.05388459346063712, -127.9746229614479631 ) ) ;
#5607 = CARTESIAN_POINT ( 'NONE',  ( 26.11404676487257603, 110.5078194225164481, -24.64483677384740545 ) ) ;
#5608 = CARTESIAN_POINT ( 'NONE',  ( -4.473127245936434626, 47.80062405537817938, 12.17046501147466842 ) ) ;
#5609 = EDGE_CURVE ( 'NONE', #25165, #23320, #11644, .T. ) ;
#5610 = ORIENTED_EDGE ( 'NONE', *, *, #19384, .T. ) ;
#5611 = CARTESIAN_POINT ( 'NONE',  ( -1.031422197589716205, 15.60268798220698017, 43.06660437151292342 ) ) ;
#5612 = ORIENTED_EDGE ( 'NONE', *, *, #21079, .F. ) ;
#5613 = B_SPLINE_CURVE_WITH_KNOTS ( 'NONE', 3,
 ( #24731, #20661, #27283, #7594, #16350, #16205 ),
 .UNSPECIFIED., .F., .F.,
 ( 4, 2, 4 ),
 ( 3.108012608937941465E-17, 0.0006311571484586140290, 0.001262314296917197484 ),
 .UNSPECIFIED. ) ;
#5614 = EDGE_CURVE ( 'NONE', #23498, #13376, #14519, .T. ) ;
#5615 = EDGE_CURVE ( 'NONE', #11790, #604, #8702, .T. ) ;
#5616 = CARTESIAN_POINT ( 'NONE',  ( -55.24271866751342941, -0.008488649505345844185, 0.004256484107793130807 ) ) ;
#5617 = CARTESIAN_POINT ( 'NONE',  ( 25.81918753295378011, -102.8711004511196450, 46.82320532096481003 ) ) ;
#5618 = CARTESIAN_POINT ( 'NONE',  ( -1.031422197589716205, -1.530725436377144755, 45.78027046666445443 ) ) ;
#5619 = VECTOR ( 'NONE', #866, 1000.000000000000114 ) ;
#5620 = CARTESIAN_POINT ( 'NONE',  ( 1.834118845439484335, 144.2964192726484214, -15.34511559672534986 ) ) ;
#5621 = CARTESIAN_POINT ( 'NONE',  ( 1.833485406944043827, 138.1714136985314383, -44.33323125129781772 ) ) ;
#5622 = CARTESIAN_POINT ( 'NONE',  ( 10.93730112725945247, 108.9902118373741331, 104.7670965581011302 ) ) ;
#5623 = CARTESIAN_POINT ( 'NONE',  ( 1.833750490713697445, -125.5350013574264523, -72.78591676344089478 ) ) ;
#5624 = CARTESIAN_POINT ( 'NONE',  ( 25.69398547355842766, -45.25878216557502043, 103.4778695380287559 ) ) ;
#5625 = ORIENTED_EDGE ( 'NONE', *, *, #24669, .F. ) ;
#5626 = VERTEX_POINT ( 'NONE', #18691 ) ;
#5627 = DIRECTION ( 'NONE',  ( 0.000000000000000000, 0.000000000000000000, 1.000000000000000000 ) ) ;
#5628 = CARTESIAN_POINT ( 'NONE',  ( -20.57838717382308147, 18.89542499756500149, -23.26537097894111383 ) ) ;
#5629 = CARTESIAN_POINT ( 'NONE',  ( 2.263178607246703056, 84.32376080825709153, -118.4461883615806670 ) ) ;
#5630 = CARTESIAN_POINT ( 'NONE',  ( -1.323439229708141429, 12.01475235539445485, -44.47813215539048315 ) ) ;
#5631 = CARTESIAN_POINT ( 'NONE',  ( 2.108393763691208012, -84.36147263237489824, -118.2927144690668086 ) ) ;
#5632 = CARTESIAN_POINT ( 'NONE',  ( 1.833485406944057594, -137.8414413349088932, 45.34878176254188276 ) ) ;
#5633 = ORIENTED_EDGE ( 'NONE', *, *, #818, .F. ) ;
#5634 = CARTESIAN_POINT ( 'NONE',  ( 1.833603222531987598, -144.3605362014089337, 14.72553080638947343 ) ) ;
#5635 = CARTESIAN_POINT ( 'NONE',  ( 8.186469777910941659, -34.43598809570042363, -145.3272523831807632 ) ) ;
#5636 = CARTESIAN_POINT ( 'NONE',  ( -20.37983603106073716, -23.16947629293375854, -18.69865230096518616 ) ) ;
#5637 = B_SPLINE_CURVE_WITH_KNOTS ( 'NONE', 3,
 ( #15422, #11129, #19901, #186, #8975, #22212, #9109 ),
 .UNSPECIFIED., .F., .F.,
 ( 4, 3, 4 ),
 ( 0.000000000000000000, 0.006568092053401801411, 0.02506242213020845253 ),
 .UNSPECIFIED. ) ;
#5638 = B_SPLINE_CURVE_WITH_KNOTS ( 'NONE', 3,
 ( #4905, #24496, #11672, #11239, #727, #4612, #20011, #26769, #13533, #15844 ),
 .UNSPECIFIED., .F., .F.,
 ( 4, 3, 3, 4 ),
 ( 2.501853776554200607E-17, 0.0002669560319015822298, 0.0005492286108966468747, 0.0008315040496093393683 ),
 .UNSPECIFIED. ) ;
#5639 = CARTESIAN_POINT ( 'NONE',  ( -20.20700224038492010, -16.58740185276728241, -24.51628800869040958 ) ) ;
#5640 = CONICAL_SURFACE ( 'NONE', #16663, 34.60786435723138510, 0.8559913436420825139 ) ;
#5641 = CARTESIAN_POINT ( 'NONE',  ( 25.64681081121880624, 66.03065707438935306, 91.59071981940594753 ) ) ;
#5642 = EDGE_CURVE ( 'NONE', #27723, #13723, #18267, .T. ) ;
#5643 = VECTOR ( 'NONE', #14783, 1000.000000000000000 ) ;
#5644 = EDGE_LOOP ( 'NONE', ( #26535, #17551, #25318, #6890 ) ) ;
#5645 = CARTESIAN_POINT ( 'NONE',  ( 1.832998868059890096, -132.3466930259790217, -59.50898020732640958 ) ) ;
#5646 = CARTESIAN_POINT ( 'NONE',  ( 10.93730112725972248, -36.23586118136624634, 146.7718404940640653 ) ) ;
#5647 = ORIENTED_EDGE ( 'NONE', *, *, #14816, .F. ) ;
#5648 = EDGE_CURVE ( 'NONE', #26826, #13127, #11765, .T. ) ;
#5649 =( BOUNDED_SURFACE ( )  B_SPLINE_SURFACE ( 3, 1, ( 
 ( #20576, #857 ),
 ( #9643, #22320 ),
 ( #18407, #20140 ),
 ( #27184, #715 ) ),
 .UNSPECIFIED., .F., .F., .F. ) 
 B_SPLINE_SURFACE_WITH_KNOTS ( ( 4, 4 ),
 ( 2, 2 ),
 ( 0.000000000000000000, 1.000000000000000000 ),
 ( 0.000000000000000000, 1.000000000000000000 ),
 .UNSPECIFIED. ) 
 GEOMETRIC_REPRESENTATION_ITEM ( )  RATIONAL_B_SPLINE_SURFACE ( (
 ( 1.000000000000000000, 1.000000000000000000),
 ( 0.6386103224230316178, 0.9954351624131538845),
 ( 0.6386103224230316178, 0.9954351624131538845),
 ( 1.000000000000000000, 1.000000000000000000) ) ) 
 REPRESENTATION_ITEM ( '' )  SURFACE ( )  );
#5650 = EDGE_CURVE ( 'NONE', #21979, #11148, #7777, .T. ) ;
#5651 = ORIENTED_EDGE ( 'NONE', *, *, #22098, .F. ) ;
#5652 = ORIENTED_EDGE ( 'NONE', *, *, #28212, .T. ) ;
#5653 = CARTESIAN_POINT ( 'NONE',  ( 26.28373643307412166, -30.57614217577372884, -123.8418562193901096 ) ) ;
#5654 = CARTESIAN_POINT ( 'NONE',  ( 19.66333377628707879, -132.3257119126253940, 38.27269871461014361 ) ) ;
#5655 = CARTESIAN_POINT ( 'NONE',  ( 1.833691583653541013, 30.51806994139792550, -141.8642667235905037 ) ) ;
#5656 = B_SPLINE_CURVE_WITH_KNOTS ( 'NONE', 3,
 ( #11591, #14165, #1089, #15911, #5255, #20369 ),
 .UNSPECIFIED., .F., .F.,
 ( 4, 2, 4 ),
 ( 3.409603294638168262E-16, 0.003576372551511143149, 0.007152745103021945425 ),
 .UNSPECIFIED. ) ;
#5657 = CARTESIAN_POINT ( 'NONE',  ( -20.20700224038492721, -24.51628800869035274, 16.58740185276737122 ) ) ;
#5658 = VECTOR ( 'NONE', #3801, 1000.000000000000114 ) ;
#5659 = CIRCLE ( 'NONE', #23614, 53.53553390275978785 ) ;
#5660 = CARTESIAN_POINT ( 'NONE',  ( -22.34422965417124729, -37.30738373203622871, -6.759368364654178230 ) ) ;
#5661 = CARTESIAN_POINT ( 'NONE',  ( 1.833838850855487035, 132.5281727421685787, 59.10274688031898904 ) ) ;
#5662 = LINE ( 'NONE', #13993, #16718 ) ;
#5663 = CARTESIAN_POINT ( 'NONE',  ( 32.73300124599735739, -103.7392577722179823, 55.46353551261974957 ) ) ;
#5664 = CARTESIAN_POINT ( 'NONE',  ( 25.64681081121879203, -110.3564950173083474, 23.88203588908045916 ) ) ;
#5665 = CARTESIAN_POINT ( 'NONE',  ( 5.340103556456292644, 143.7310399800117011, 32.90561046456755179 ) ) ;
#5666 = EDGE_CURVE ( 'NONE', #8915, #22329, #11448, .T. ) ;
#5667 = B_SPLINE_CURVE_WITH_KNOTS ( 'NONE', 3,
 ( #22302, #17398, #8632, #15375, #26598, #19565 ),
 .UNSPECIFIED., .F., .F.,
 ( 4, 2, 4 ),
 ( 3.469446951953614189E-18, 0.0006311636237756632984, 0.001262327247551323344 ),
 .UNSPECIFIED. ) ;
#5668 = CARTESIAN_POINT ( 'NONE',  ( 25.64692872815577473, -66.10702795113353147, -91.53575854059484129 ) ) ;
#5669 = CARTESIAN_POINT ( 'NONE',  ( 1.833485406944057594, 97.49333871408690300, 107.4794113447412940 ) ) ;
#5670 = DIRECTION ( 'NONE',  ( -0.7637818620346801257, 0.6451161201712179993, -0.02150485345385064542 ) ) ;
#5671 = CARTESIAN_POINT ( 'NONE',  ( 32.73300124599738581, -115.8010721414081985, -20.69176323058746902 ) ) ;
#5672 = ADVANCED_FACE ( 'NONE', ( #18981 ), #24661, .F. ) ;
#5673 = VERTEX_POINT ( 'NONE', #7632 ) ;
#5674 = CARTESIAN_POINT ( 'NONE',  ( 13.36082413113063083, 37.97423473099294000, 148.1362653801003830 ) ) ;
#5675 = EDGE_CURVE ( 'NONE', #26606, #20294, #18455, .T. ) ;
#5676 = ORIENTED_EDGE ( 'NONE', *, *, #23849, .F. ) ;
#5677 = DIRECTION ( 'NONE',  ( 1.000000000000000000, -6.938893903907226837E-18, 1.734723475976806709E-18 ) ) ;
#5678 = CARTESIAN_POINT ( 'NONE',  ( 28.37603512858440880, 105.5302493666427353, 45.02094145483413712 ) ) ;
#5679 = ORIENTED_EDGE ( 'NONE', *, *, #4961, .F. ) ;
#5680 = AXIS2_PLACEMENT_3D ( 'NONE', #24713, #22543, #5105 ) ;
#5681 = ORIENTED_EDGE ( 'NONE', *, *, #8143, .T. ) ;
#5683 =( BOUNDED_SURFACE ( )  B_SPLINE_SURFACE ( 3, 1, ( 
 ( #12379, #6072 ),
 ( #7809, #14961 ),
 ( #25921, #10662 ),
 ( #23351, #23487 ) ),
 .UNSPECIFIED., .F., .F., .F. ) 
 B_SPLINE_SURFACE_WITH_KNOTS ( ( 4, 4 ),
 ( 2, 2 ),
 ( 0.000000000000000000, 1.000000000000000000 ),
 ( 0.000000000000000000, 1.000000000000000000 ),
 .UNSPECIFIED. ) 
 GEOMETRIC_REPRESENTATION_ITEM ( )  RATIONAL_B_SPLINE_SURFACE ( (
 ( 1.000000000000000000, 1.000000000000000000),
 ( 0.9956975270656954757, 0.8568959468854893125),
 ( 0.9956975270656954757, 0.8568959468854893125),
 ( 1.000000000000000000, 1.000000000000000000) ) ) 
 REPRESENTATION_ITEM ( '' )  SURFACE ( )  );
#5682 = VECTOR ( 'NONE', #871, 1000.000000000000000 ) ;
#5684 = ORIENTED_EDGE ( 'NONE', *, *, #4636, .T. ) ;
#5685 = CARTESIAN_POINT ( 'NONE',  ( 10.93730112725990367, -125.1380233598473950, -84.82621002473567273 ) ) ;
#5686 = CARTESIAN_POINT ( 'NONE',  ( -1.045287976400351981, 43.05558670614237116, -15.59869763335110449 ) ) ;
#5687 = B_SPLINE_CURVE_WITH_KNOTS ( 'NONE', 3,
 ( #28016, #17082, #21688, #28156, #15050, #6580, #17355, #17225 ),
 .UNSPECIFIED., .F., .F.,
 ( 4, 2, 2, 4 ),
 ( 3.469446951953614189E-18, 0.0002429592666046748086, 0.0004859185332093461478, 0.0009718370664186862240 ),
 .UNSPECIFIED. ) ;
#5688 = CARTESIAN_POINT ( 'NONE',  ( 16.75465622695653778, -142.1502242093126256, -4.637075857202995088 ) ) ;
#5689 = CARTESIAN_POINT ( 'NONE',  ( 6.224689322667630975, 141.5842213414019568, -43.30635742325229387 ) ) ;
#5690 = CARTESIAN_POINT ( 'NONE',  ( 25.64681081121879203, 35.28660243342691416, -107.2555980796237804 ) ) ;
#5691 = CARTESIAN_POINT ( 'NONE',  ( -1.463510566862830986, 29.09194585123833932, -35.90603835816513367 ) ) ;
#5692 = APPLICATION_CONTEXT ( 'automotive_design' ) ;
#5693 = CARTESIAN_POINT ( 'NONE',  ( -20.20700224038492010, 8.199606986804733211, 28.44216453106527709 ) ) ;
#5695 = CARTESIAN_POINT ( 'NONE',  ( 109.1721716018069657, 0.005082060336469409849, -0.01629455849720092692 ) ) ;
#5694 = CARTESIAN_POINT ( 'NONE',  ( -24.53239521893647179, -16.68574937150994231, -29.54733954334103174 ) ) ;
#5696 = CARTESIAN_POINT ( 'NONE',  ( 1.833603222531999810, 132.7445893798465590, -58.61467103263608891 ) ) ;
#5697 = EDGE_CURVE ( 'NONE', #7508, #27740, #9731, .T. ) ;
#5698 = EDGE_LOOP ( 'NONE', ( #3719, #15342, #17465, #15481 ) ) ;
#5699 = VERTEX_POINT ( 'NONE', #12348 ) ;
#5700 = DIRECTION ( 'NONE',  ( 0.000000000000000000, 0.000000000000000000, 1.000000000000000000 ) ) ;
#5701 = EDGE_CURVE ( 'NONE', #4874, #9075, #7341, .T. ) ;
#5703 = CARTESIAN_POINT ( 'NONE',  ( 25.64681081121879203, 75.86069728269103507, -83.63051021305824406 ) ) ;
#5702 = CARTESIAN_POINT ( 'NONE',  ( -1.113427685306995318, 28.52429901637220411, 35.91272432484627330 ) ) ;
#5704 = CARTESIAN_POINT ( 'NONE',  ( 55.49584447822657296, 48.74506217377881967, 53.73688382046282186 ) ) ;
#5705 = CARTESIAN_POINT ( 'NONE',  ( 1.831572820252008738, -116.8148281295963358, -86.09108691067891073 ) ) ;
#5706 = DIRECTION ( 'NONE',  ( -1.000000000000000000, -0.000000000000000000, -0.000000000000000000 ) ) ;
#5707 = ORIENTED_EDGE ( 'NONE', *, *, #23102, .T. ) ;
#5708 = CARTESIAN_POINT ( 'NONE',  ( -55.25719721206881729, -0.009391134844732829459, -0.006045473558784549006 ) ) ;
#5709 = ADVANCED_FACE ( 'NONE', ( #21934 ), #28312, .F. ) ;
#5710 = CARTESIAN_POINT ( 'NONE',  ( -55.24728320129491266, 0.003868537197317211632, -0.01402509393918151964 ) ) ;
#5711 = B_SPLINE_CURVE_WITH_KNOTS ( 'NONE', 3,
 ( #2709, #20119, #9484, #9054, #5154, #5005, #22590, #27012 ),
 .UNSPECIFIED., .F., .F.,
 ( 4, 2, 2, 4 ),
 ( 2.324173423859648542E-16, 0.002761568181852869838, 0.005523136363705506355, 0.01104627272741078026 ),
 .UNSPECIFIED. ) ;
#5712 = CARTESIAN_POINT ( 'NONE',  ( 1.833838848569429691, -14.99110384899624826, 144.3334397096298289 ) ) ;
#5713 = ORIENTED_EDGE ( 'NONE', *, *, #10070, .T. ) ;
#5714 = B_SPLINE_CURVE_WITH_KNOTS ( 'NONE', 3,
 ( #27968, #10306, #19065, #8008, #16770, #23687, #27697, #3937, #3799, #25412 ),
 .UNSPECIFIED., .F., .F.,
 ( 4, 3, 3, 4 ),
 ( 2.428612866367529932E-17, 0.0002669559177086305315, 0.0005339118354151180289, 0.001067817517169162515 ),
 .UNSPECIFIED. ) ;
#5715 = CARTESIAN_POINT ( 'NONE',  ( -55.25719721206881729, -0.007063345920780820901, -0.008651607285661404648 ) ) ;
#5716 = CARTESIAN_POINT ( 'NONE',  ( -5.986830583229487246, -49.46736940480267464, -11.27873876172122181 ) ) ;
#5717 = EDGE_CURVE ( 'NONE', #8132, #23403, #26536, .T. ) ;
#5718 = VECTOR ( 'NONE', #24019, 1000.000000000000114 ) ;
#5719 = VERTEX_POINT ( 'NONE', #22226 ) ;
#5720 = ORIENTED_EDGE ( 'NONE', *, *, #1960, .T. ) ;
#5721 = CARTESIAN_POINT ( 'NONE',  ( -1.619063947482194177, 29.22875152547808852, 35.99532424477347092 ) ) ;
#5722 = ORIENTED_EDGE ( 'NONE', *, *, #18217, .T. ) ;
#5723 = CARTESIAN_POINT ( 'NONE',  ( 32.73300124599735739, -55.46353551262085091, 103.7392577722174565 ) ) ;
#5724 = PRODUCT_CONTEXT ( 'NONE', #16352, 'mechanical' ) ;
#5725 = DIRECTION ( 'NONE',  ( 0.7563875759206388771, -0.4122509917856713724, 0.5078650950445698919 ) ) ;
#5726 = CARTESIAN_POINT ( 'NONE',  ( 1.833485406944043827, -59.50871042846314651, 132.3460930279889567 ) ) ;
#5727 = CARTESIAN_POINT ( 'NONE',  ( 1.833485406944057594, -117.7091014914944225, -84.86072343962690923 ) ) ;
#5728 = DIRECTION ( 'NONE',  ( 0.5914120900931444380, -0.7903769105750364510, 0.1598001217819286501 ) ) ;
#5729 = CARTESIAN_POINT ( 'NONE',  ( 109.1586900883932856, -0.007137750914552287197, -0.0001010081143883946364 ) ) ;
#5730 = CARTESIAN_POINT ( 'NONE',  ( 1.832998868059858122, 30.69214149074014841, 141.8272129421609691 ) ) ;
#5731 = ORIENTED_EDGE ( 'NONE', *, *, #3967, .T. ) ;
#5732 =( BOUNDED_SURFACE ( )  B_SPLINE_SURFACE ( 3, 1, ( 
 ( #7112, #4359 ),
 ( #13414, #4793 ),
 ( #26373, #21920 ),
 ( #19900, #10987 ) ),
 .UNSPECIFIED., .F., .F., .F. ) 
 B_SPLINE_SURFACE_WITH_KNOTS ( ( 4, 4 ),
 ( 2, 2 ),
 ( 0.000000000000000000, 1.000000000000000000 ),
 ( 0.000000000000000000, 1.000000000000000000 ),
 .UNSPECIFIED. ) 
 GEOMETRIC_REPRESENTATION_ITEM ( )  RATIONAL_B_SPLINE_SURFACE ( (
 ( 1.000000000000000000, 1.000000000000000000),
 ( 0.9934239774497838349, 0.8357310067453913582),
 ( 0.9934239774497838349, 0.8357310067453913582),
 ( 1.000000000000000000, 1.000000000000000000) ) ) 
 REPRESENTATION_ITEM ( '' )  SURFACE ( )  );
#5733 = CARTESIAN_POINT ( 'NONE',  ( 28.43349137099835744, -4.052139611197551616, -124.1860347533534252 ) ) ;
#5735 = CARTESIAN_POINT ( 'NONE',  ( -1.539760825549685519, -46.22267384399379608, 2.469813586483570855 ) ) ;
#5734 = CARTESIAN_POINT ( 'NONE',  ( -55.24340739397742794, -0.002421372372456151618, 0.009842732675348802793 ) ) ;
#5736 = LINE ( 'NONE', #10201, #19803 ) ;
#5737 = ORIENTED_EDGE ( 'NONE', *, *, #7671, .T. ) ;
#5738 = ORIENTED_EDGE ( 'NONE', *, *, #6733, .T. ) ;
#5739 = ORIENTED_EDGE ( 'NONE', *, *, #24669, .T. ) ;
#5740 = CARTESIAN_POINT ( 'NONE',  ( -20.21097721650786738, 9.464413208035470149, 28.05863614620928459 ) ) ;
#5741 = CARTESIAN_POINT ( 'NONE',  ( 10.93730112725945602, 84.82621002473440797, 125.1380233598478640 ) ) ;
#5742 = EDGE_CURVE ( 'NONE', #5899, #25988, #2071, .T. ) ;
#5743 = CARTESIAN_POINT ( 'NONE',  ( -24.53239521893647890, -6.738460611583005466, -33.25736993155761922 ) ) ;
#5744 = CARTESIAN_POINT ( 'NONE',  ( -24.53239521893653929, 30.86654523348686041, 14.09666242510765954 ) ) ;
#5745 = DIRECTION ( 'NONE',  ( 1.000000000000000000, -6.938893903907226837E-18, 1.734723475976806709E-18 ) ) ;
#5746 = EDGE_LOOP ( 'NONE', ( #10300, #11762, #18359, #8310 ) ) ;
#5747 = CARTESIAN_POINT ( 'NONE',  ( 1.833485406944043827, 72.09189602597706426, 125.9346397303438039 ) ) ;
#5748 = DIRECTION ( 'NONE',  ( 0.000000000000000000, 0.000000000000000000, 1.000000000000000000 ) ) ;
#5749 = ORIENTED_EDGE ( 'NONE', *, *, #20539, .F. ) ;
#5750 = CARTESIAN_POINT ( 'NONE',  ( -8.786685647604890903, 47.14957014837354876, -25.35688121747519119 ) ) ;
#5751 = CARTESIAN_POINT ( 'NONE',  ( 13.84597867724974840, -25.80666409311465159, -144.4146018799366402 ) ) ;
#5752 = CARTESIAN_POINT ( 'NONE',  ( -1.539760825549689294, 44.72358953107748647, 11.93465943778467597 ) ) ;
#5753 = CARTESIAN_POINT ( 'NONE',  ( 109.1721716018069515, -0.01127028715939363233, -0.01281875973823913897 ) ) ;
#5754 = ADVANCED_FACE ( 'NONE', ( #13147 ), #1834, .F. ) ;
#5755 = CARTESIAN_POINT ( 'NONE',  ( -20.57838717382308147, 18.89542499756533545, 23.26537097894084383 ) ) ;
#5756 = CARTESIAN_POINT ( 'NONE',  ( 109.1587776205901861, 0.004842060007769388025, -0.005502145856762321631 ) ) ;
#5757 = CARTESIAN_POINT ( 'NONE',  ( 109.1586900883932856, 0.007109207791181753125, -0.0006456433529162696654 ) ) ;
#5758 = ORIENTED_EDGE ( 'NONE', *, *, #18604, .T. ) ;
#5759 = B_SPLINE_CURVE_WITH_KNOTS ( 'NONE', 3,
 ( #21396, #21680, #23999, #14774, #10470, #3845, #21824, #2220 ),
 .UNSPECIFIED., .F., .F.,
 ( 4, 2, 2, 4 ),
 ( 2.030441771438897272E-17, 0.0002429592666046836720, 0.0004859185332093470693, 0.0009718370664186737557 ),
 .UNSPECIFIED. ) ;
#5760 = CARTESIAN_POINT ( 'NONE',  ( 26.11404676487257603, -83.38016054979729574, -76.59696442953277540 ) ) ;
#5761 = CARTESIAN_POINT ( 'NONE',  ( 109.1586059443104944, -0.005438258427231163275, -0.004524147648825544571 ) ) ;
#5762 = CARTESIAN_POINT ( 'NONE',  ( 109.1624594426973260, -0.01263706729758975501, -0.009754804742273411738 ) ) ;
#5763 = ORIENTED_EDGE ( 'NONE', *, *, #6361, .T. ) ;
#5764 = FACE_OUTER_BOUND ( 'NONE', #4518, .T. ) ;
#5765 = CARTESIAN_POINT ( 'NONE',  ( -1.046935749539997573, 45.77872888003167162, 1.275486069320633353 ) ) ;
#5766 = CARTESIAN_POINT ( 'NONE',  ( 109.1592201516379674, -0.0003082430541935533277, 0.007856029051018016685 ) ) ;
#5767 = CARTESIAN_POINT ( 'NONE',  ( -23.79223135445720061, 3.207301057648340503, -33.03345552685145492 ) ) ;
#5768 = CARTESIAN_POINT ( 'NONE',  ( -2.904412668506679118, 46.12477647685274462, -11.97478724945526629 ) ) ;
#5769 = B_SPLINE_CURVE_WITH_KNOTS ( 'NONE', 3,
 ( #528, #13480, #22276, #24592, #4851, #13620, #26159, #22419 ),
 .UNSPECIFIED., .F., .F.,
 ( 4, 2, 2, 4 ),
 ( 1.250926888277100303E-17, 0.0002429592666046810699, 0.0004859185332093496172, 0.0009718370664186909945 ),
 .UNSPECIFIED. ) ;
#5770 = CARTESIAN_POINT ( 'NONE',  ( 1.833691583653495716, -137.8971124741065637, -45.17974255430956276 ) ) ;
#5771 = CARTESIAN_POINT ( 'NONE',  ( 5.340103579038303572, 117.9209211655070106, -88.52145169228850818 ) ) ;
#5772 = B_SPLINE_CURVE_WITH_KNOTS ( 'NONE', 3,
 ( #8498, #1856, #19285, #12519, #15090, #2000, #23908 ),
 .UNSPECIFIED., .F., .F.,
 ( 4, 3, 4 ),
 ( 0.000000000000000000, 0.02398743853561418823, 0.04000277880656218088 ),
 .UNSPECIFIED. ) ;
#5773 = CARTESIAN_POINT ( 'NONE',  ( 1.833838848569426139, -58.85887272891280730, 132.6367525013575346 ) ) ;
#5774 = DIRECTION ( 'NONE',  ( -1.000000000000000000, 6.938893903907226837E-18, -1.734723475976806709E-18 ) ) ;
#5775 = LINE ( 'NONE', #18857, #16876 ) ;
#5776 = ORIENTED_EDGE ( 'NONE', *, *, #16868, .F. ) ;
#5777 =( BOUNDED_SURFACE ( )  B_SPLINE_SURFACE ( 3, 1, ( 
 ( #14675, #23478 ),
 ( #6206, #25354 ),
 ( #21008, #10094 ),
 ( #14952, #5779 ) ),
 .UNSPECIFIED., .F., .F., .F. ) 
 B_SPLINE_SURFACE_WITH_KNOTS ( ( 4, 4 ),
 ( 2, 2 ),
 ( 0.000000000000000000, 1.000000000000000000 ),
 ( 0.000000000000000000, 1.000000000000000000 ),
 .UNSPECIFIED. ) 
 GEOMETRIC_REPRESENTATION_ITEM ( )  RATIONAL_B_SPLINE_SURFACE ( (
 ( 1.000000000000000000, 1.000000000000000000),
 ( 0.6386103224230316178, 0.9954351624131538845),
 ( 0.6386103224230316178, 0.9954351624131538845),
 ( 1.000000000000000000, 1.000000000000000000) ) ) 
 REPRESENTATION_ITEM ( '' )  SURFACE ( )  );
#5778 = ORIENTED_EDGE ( 'NONE', *, *, #27657, .T. ) ;
#5779 = CARTESIAN_POINT ( 'NONE',  ( 2.430230287190592531, 57.85706160874325832, -133.5180086894985436 ) ) ;
#5780 = CARTESIAN_POINT ( 'NONE',  ( 1.893872463202045830, 107.2274879309827611, 97.83022426231997315 ) ) ;
#5781 = EDGE_CURVE ( 'NONE', #14642, #10702, #16254, .T. ) ;
#5782 = CARTESIAN_POINT ( 'NONE',  ( 1.833485406944043827, 84.86072343962726450, -117.7091014914941809 ) ) ;
#5783 = DIRECTION ( 'NONE',  ( 1.000000000000000000, -6.938893903907226837E-18, 1.734723475976806709E-18 ) ) ;
#5784 = DIRECTION ( 'NONE',  ( -1.000000000000000000, -0.000000000000000000, -0.000000000000000000 ) ) ;
#5785 = CARTESIAN_POINT ( 'NONE',  ( -1.583189561560253589, 38.94740041318330981, 25.21827308671188561 ) ) ;
#5786 = DIRECTION ( 'NONE',  ( -0.5946245182733607137, -0.5357871896547490298, 0.5994612328333164264 ) ) ;
#5787 = ORIENTED_EDGE ( 'NONE', *, *, #6742, .F. ) ;
#5788 = CARTESIAN_POINT ( 'NONE',  ( 32.73300124599732186, 0.000000000000000000, 0.000000000000000000 ) ) ;
#5789 = CARTESIAN_POINT ( 'NONE',  ( -20.24399999263415850, -18.44171895251379567, 23.20123049637386003 ) ) ;
#5790 = FACE_OUTER_BOUND ( 'NONE', #13400, .T. ) ;
#5791 = ADVANCED_FACE ( 'NONE', ( #20050 ), #16746, .F. ) ;
#5792 = B_SPLINE_CURVE_WITH_KNOTS ( 'NONE', 3,
 ( #26359, #6661, #9092, #20023 ),
 .UNSPECIFIED., .F., .F.,
 ( 4, 4 ),
 ( 1.534813690070764878E-16, 0.008383748772659597656 ),
 .UNSPECIFIED. ) ;
#5793 = EDGE_CURVE ( 'NONE', #11289, #26082, #19644, .T. ) ;
#5794 = CARTESIAN_POINT ( 'NONE',  ( 119.2224693531408803, 90.00000000000005684, 39.99999999999999289 ) ) ;
#5795 = CARTESIAN_POINT ( 'NONE',  ( 10.93730112725983439, -148.8212007290663621, 26.59437931460704263 ) ) ;
#5796 = ORIENTED_EDGE ( 'NONE', *, *, #22369, .T. ) ;
#5797 = CARTESIAN_POINT ( 'NONE',  ( 25.64704443564079739, -11.66968230815837337, -112.3065506427462736 ) ) ;
#5798 = VERTEX_POINT ( 'NONE', #54 ) ;
#5799 = B_SPLINE_CURVE_WITH_KNOTS ( 'NONE', 3,
 ( #11681, #22785, #9524, #13828, #20452, #26920, #18275, #26779 ),
 .UNSPECIFIED., .F., .F.,
 ( 4, 2, 2, 4 ),
 ( 2.189053321159284187E-16, 0.002761568181852863766, 0.005523136363705508090, 0.01104627272741077852 ),
 .UNSPECIFIED. ) ;
#5800 = ORIENTED_EDGE ( 'NONE', *, *, #12768, .F. ) ;
#5801 = ORIENTED_EDGE ( 'NONE', *, *, #19929, .F. ) ;
#5802 = CARTESIAN_POINT ( 'NONE',  ( 28.43349137099838586, -29.78331910005408645, -120.6297847406439985 ) ) ;
#5803 = EDGE_CURVE ( 'NONE', #12270, #18370, #15892, .T. ) ;
#5804 = CARTESIAN_POINT ( 'NONE',  ( -20.57838717382308147, 10.78122205917039977, 27.96569011373074076 ) ) ;
#5805 = DIRECTION ( 'NONE',  ( 1.000000000000000000, -6.938893903907226837E-18, 1.734723475976806709E-18 ) ) ;
#5806 = CARTESIAN_POINT ( 'NONE',  ( 9.884929003653626367, -4.203795436551307496, -150.4771565009631047 ) ) ;
#5807 = ORIENTED_EDGE ( 'NONE', *, *, #17627, .F. ) ;
#5808 = CARTESIAN_POINT ( 'NONE',  ( 10.93730112725996051, 20.69552240458543224, -149.7554878793147282 ) ) ;
#5809 = CARTESIAN_POINT ( 'NONE',  ( 5.340103556456536005, 88.52145167812754778, -117.9209211572677418 ) ) ;
#5810 = EDGE_CURVE ( 'NONE', #27903, #26589, #13130, .T. ) ;
#5811 = EDGE_CURVE ( 'NONE', #14545, #449, #20010, .T. ) ;
#5812 = FACE_OUTER_BOUND ( 'NONE', #24437, .T. ) ;
#5813 = CARTESIAN_POINT ( 'NONE',  ( -22.23342874802668234, -11.82490389046295043, 29.33662284748872651 ) ) ;
#5814 = CARTESIAN_POINT ( 'NONE',  ( -20.20898968516257810, 0.6607166829023055632, 29.59696826051171925 ) ) ;
#5815 = CARTESIAN_POINT ( 'NONE',  ( 1.833721034905656744, -142.0123736691684542, -29.82176961967059370 ) ) ;
#5816 = LINE ( 'NONE', #14575, #10062 ) ;
#5817 = CARTESIAN_POINT ( 'NONE',  ( -55.24390624410018802, 0.01032895241567037548, -0.001451500391950801341 ) ) ;
#5818 = CARTESIAN_POINT ( 'NONE',  ( 30.59141879584289114, -115.8270959620729030, 9.457572341076161848 ) ) ;
#5819 = CARTESIAN_POINT ( 'NONE',  ( -7.078251931573406708, 11.16394717458676311, -50.86685171665416050 ) ) ;
#5820 = CARTESIAN_POINT ( 'NONE',  ( 109.1778270068192853, -0.003465086990427028186, -0.008646067828078151524 ) ) ;
#5821 = CARTESIAN_POINT ( 'NONE',  ( 55.49584447822657296, 72.55110015779771970, -0.2676470673959188695 ) ) ;
#5822 =( BOUNDED_SURFACE ( )  B_SPLINE_SURFACE ( 3, 1, ( 
 ( #6783, #26340 ),
 ( #15527, #15106 ),
 ( #8792, #284 ),
 ( #10821, #23925 ) ),
 .UNSPECIFIED., .F., .F., .F. ) 
 B_SPLINE_SURFACE_WITH_KNOTS ( ( 4, 4 ),
 ( 2, 2 ),
 ( 0.000000000000000000, 1.000000000000000000 ),
 ( 0.000000000000000000, 1.000000000000000000 ),
 .UNSPECIFIED. ) 
 GEOMETRIC_REPRESENTATION_ITEM ( )  RATIONAL_B_SPLINE_SURFACE ( (
 ( 1.000000000000000000, 1.000000000000000000),
 ( 0.9934239774497837239, 0.8357310067453919133),
 ( 0.9934239774497837239, 0.8357310067453919133),
 ( 1.000000000000000000, 1.000000000000000000) ) ) 
 REPRESENTATION_ITEM ( '' )  SURFACE ( )  );
#5823 = ORIENTED_EDGE ( 'NONE', *, *, #20701, .T. ) ;
#5824 = ORIENTED_EDGE ( 'NONE', *, *, #5427, .T. ) ;
#5825 = FACE_OUTER_BOUND ( 'NONE', #4603, .T. ) ;
#5826 = CARTESIAN_POINT ( 'NONE',  ( -1.048994561756802391, 26.29622118251734619, 37.49601524795380669 ) ) ;
#5827 = ORIENTED_EDGE ( 'NONE', *, *, #5614, .F. ) ;
#5828 = ORIENTED_EDGE ( 'NONE', *, *, #23955, .F. ) ;
#5829 = ORIENTED_EDGE ( 'NONE', *, *, #24968, .T. ) ;
#5830 = CARTESIAN_POINT ( 'NONE',  ( 109.1586059443104944, 0.003294606663363240043, 0.006260042619939244421 ) ) ;
#5831 = ADVANCED_FACE ( 'NONE', ( #15882 ), #25576, .F. ) ;
#5832 = CARTESIAN_POINT ( 'NONE',  ( 55.79472521941428198, -58.42842213658356343, 43.35047097963431639 ) ) ;
#5833 = ADVANCED_FACE ( 'NONE', ( #27237 ), #28477, .F. ) ;
#5834 = CARTESIAN_POINT ( 'NONE',  ( 28.37603512858448340, -98.45183098818029066, 58.91311972676509612 ) ) ;
#5835 = CARTESIAN_POINT ( 'NONE',  ( 26.11404676487257603, -65.63269960453305885, 92.25884714080386573 ) ) ;
#5836 = CARTESIAN_POINT ( 'NONE',  ( 2.263178113027032978, -86.59154384226256695, 116.7985471375928768 ) ) ;
#5837 = CARTESIAN_POINT ( 'NONE',  ( 25.64708228042119842, 56.42152786924503260, 97.80372460135694723 ) ) ;
#5838 = DIRECTION ( 'NONE',  ( 1.000000000000000000, -6.938893903907226837E-18, 1.734723475976806709E-18 ) ) ;
#5839 = ORIENTED_EDGE ( 'NONE', *, *, #20303, .T. ) ;
#5840 = ORIENTED_EDGE ( 'NONE', *, *, #3412, .T. ) ;
#5841 = CARTESIAN_POINT ( 'NONE',  ( 25.64708228042119487, -107.3728320282186530, -34.92896069507395396 ) ) ;
#5843 = CARTESIAN_POINT ( 'NONE',  ( 0.000000000000000000, 0.000000000000000000, 0.000000000000000000 ) ) ;
#5842 = CARTESIAN_POINT ( 'NONE',  ( 2.433796855181205476, 144.8571464219891141, -13.76554153471544417 ) ) ;
#5844 = DIRECTION ( 'NONE',  ( 1.000000000000000000, -6.938893903907226837E-18, 1.734723475976806709E-18 ) ) ;
#5845 = CARTESIAN_POINT ( 'NONE',  ( 25.73574536432413851, 90.91878692682031726, 67.05280231777534539 ) ) ;
#5846 = ORIENTED_EDGE ( 'NONE', *, *, #19326, .T. ) ;
#5847 = CARTESIAN_POINT ( 'NONE',  ( -9.156249394959713683, -8.027840202794317648, -53.90509764945126392 ) ) ;
#5848 =( BOUNDED_SURFACE ( )  B_SPLINE_SURFACE ( 3, 1, ( 
 ( #16559, #1443 ),
 ( #11954, #9813 ),
 ( #3746, #23480 ),
 ( #21303, #14238 ) ),
 .UNSPECIFIED., .F., .F., .F. ) 
 B_SPLINE_SURFACE_WITH_KNOTS ( ( 4, 4 ),
 ( 2, 2 ),
 ( 0.000000000000000000, 1.000000000000000000 ),
 ( 0.000000000000000000, 1.000000000000000000 ),
 .UNSPECIFIED. ) 
 GEOMETRIC_REPRESENTATION_ITEM ( )  RATIONAL_B_SPLINE_SURFACE ( (
 ( 1.000000000000000000, 1.000000000000000000),
 ( 0.9960225298536222738, 0.9999952330161893110),
 ( 0.9960225298536222738, 0.9999952330161893110),
 ( 1.000000000000000000, 1.000000000000000000) ) ) 
 REPRESENTATION_ITEM ( '' )  SURFACE ( )  );
#5849 = CARTESIAN_POINT ( 'NONE',  ( -1.019300379054419725, 2.023851374323315078, 45.76814864815086992 ) ) ;
#5850 = CARTESIAN_POINT ( 'NONE',  ( 1.833485406944057594, -85.72460230293616235, -117.0814567582553281 ) ) ;
#5851 = ORIENTED_EDGE ( 'NONE', *, *, #27117, .T. ) ;
#5852 = ORIENTED_EDGE ( 'NONE', *, *, #5811, .F. ) ;
#5854 = CARTESIAN_POINT ( 'NONE',  ( 1.831572820252008738, -125.1738732943805132, -73.40899645746137026 ) ) ;
#5853 = B_SPLINE_CURVE_WITH_KNOTS ( 'NONE', 3,
 ( #3802, #1637, #8270, #12575 ),
 .UNSPECIFIED., .F., .F.,
 ( 4, 4 ),
 ( 0.000000000000000000, 0.008383560773332712074 ),
 .UNSPECIFIED. ) ;
#5855 = ORIENTED_EDGE ( 'NONE', *, *, #9371, .T. ) ;
#5856 = VECTOR ( 'NONE', #27005, 999.9999999999998863 ) ;
#5857 = ORIENTED_EDGE ( 'NONE', *, *, #3415, .T. ) ;
#5858 = CARTESIAN_POINT ( 'NONE',  ( 1.833838850093440387, 97.09738632349036891, 107.8375672471886020 ) ) ;
#5859 = ADVANCED_FACE ( 'NONE', ( #24965 ), #2950, .F. ) ;
#5860 = ORIENTED_EDGE ( 'NONE', *, *, #28321, .F. ) ;
#5861 = CARTESIAN_POINT ( 'NONE',  ( -1.463510566862828766, -43.13857742234517190, -16.57250862017402682 ) ) ;
#5862 = CARTESIAN_POINT ( 'NONE',  ( 32.73300124599732186, 0.000000000000000000, 0.000000000000000000 ) ) ;
#5863 = ADVANCED_FACE ( 'NONE', ( #7551 ), #4792, .F. ) ;
#5864 = CARTESIAN_POINT ( 'NONE',  ( -25.21435515916025594, 34.29329011225976132, 4.655591116594488099 ) ) ;
#5865 = EDGE_CURVE ( 'NONE', #28334, #20235, #11996, .T. ) ;
#5866 = CARTESIAN_POINT ( 'NONE',  ( -4.473127245936434626, -37.94261489385694830, 31.51789735524234004 ) ) ;
#5867 = DIRECTION ( 'NONE',  ( 0.7637818620346800147, 0.3617919495470829916, 0.5345501402766235088 ) ) ;
#5868 = CARTESIAN_POINT ( 'NONE',  ( 1.832998868059858122, 141.8272129421608554, 30.69214149074063513 ) ) ;
#5869 = CARTESIAN_POINT ( 'NONE',  ( 1.833485406944043827, -107.4794113447402566, -97.49333871408801144 ) ) ;
#5870 = ORIENTED_EDGE ( 'NONE', *, *, #4526, .T. ) ;
#5871 = EDGE_CURVE ( 'NONE', #21801, #3497, #28265, .T. ) ;
#5872 = CARTESIAN_POINT ( 'NONE',  ( -1.046936909428679563, -12.93351869073243243, 43.93225665392628088 ) ) ;
#5874 = CARTESIAN_POINT ( 'NONE',  ( -1.049819825607605672, 43.39756533277881800, -14.63675055554395321 ) ) ;
#5873 = CARTESIAN_POINT ( 'NONE',  ( 25.64681081121879203, -97.99105938547884875, -56.09509703373446854 ) ) ;
#5875 = CARTESIAN_POINT ( 'NONE',  ( -1.259920593601976169, 28.82601305773653877, -35.85909937955931071 ) ) ;
#5876 = ORIENTED_EDGE ( 'NONE', *, *, #7736, .F. ) ;
#5877 = ORIENTED_EDGE ( 'NONE', *, *, #13220, .T. ) ;
#5878 = CARTESIAN_POINT ( 'NONE',  ( -55.24340739397742084, -0.006539691034612123317, 0.007744344507854589339 ) ) ;
#5879 = CARTESIAN_POINT ( 'NONE',  ( 1.834118845439484335, -137.9527673765102520, -45.01070051384731130 ) ) ;
#5881 = CARTESIAN_POINT ( 'NONE',  ( 19.66333377628691892, -127.6002314355562675, 51.89484018353797268 ) ) ;
#5880 = FACE_OUTER_BOUND ( 'NONE', #6594, .T. ) ;
#5882 = CARTESIAN_POINT ( 'NONE',  ( -20.24419206586954090, 27.76448493191444200, -10.37009329716774708 ) ) ;
#5883 = CARTESIAN_POINT ( 'NONE',  ( -1.044557008772714513, -12.57891310333380552, -44.03203053429566438 ) ) ;
#5884 = ORIENTED_EDGE ( 'NONE', *, *, #599, .F. ) ;
#5885 = LINE ( 'NONE', #12896, #8807 ) ;
#5886 = CARTESIAN_POINT ( 'NONE',  ( -1.463510566862834539, 38.76366072687779507, -25.15876608740827436 ) ) ;
#5887 = ORIENTED_EDGE ( 'NONE', *, *, #25756, .F. ) ;
#5888 = CARTESIAN_POINT ( 'NONE',  ( -25.21435515916043002, 30.48034229288640162, -16.39063784838753790 ) ) ;
#5889 = CARTESIAN_POINT ( 'NONE',  ( 25.64699802086726166, -112.2675771984164754, 12.03888878460436729 ) ) ;
#5890 = CARTESIAN_POINT ( 'NONE',  ( 55.79472521941428198, 71.00924468211177043, -15.83764557006200135 ) ) ;
#5891 = DIRECTION ( 'NONE',  ( 0.000000000000000000, 5.223019709708233256E-21, -1.000000000000000000 ) ) ;
#5892 = CARTESIAN_POINT ( 'NONE',  ( 5.340103579038286696, 71.72120379026205228, -128.8311297206835206 ) ) ;
#5893 = CARTESIAN_POINT ( 'NONE',  ( -4.780792508754322157, 42.16805077400959334, -25.98388465890095489 ) ) ;
#5894 = CARTESIAN_POINT ( 'NONE',  ( 25.64660436782575559, -84.29628170537181120, -75.12017330820542327 ) ) ;
#5895 = EDGE_LOOP ( 'NONE', ( #10327, #26498, #10115, #5966 ) ) ;
#5896 = CARTESIAN_POINT ( 'NONE',  ( 10.93730112725972248, -36.23586118136624634, 146.7718404940640653 ) ) ;
#5897 =( BOUNDED_SURFACE ( )  B_SPLINE_SURFACE ( 3, 1, ( 
 ( #1708, #10922 ),
 ( #12927, #4298 ),
 ( #28453, #8619 ),
 ( #23765, #13201 ) ),
 .UNSPECIFIED., .F., .F., .F. ) 
 B_SPLINE_SURFACE_WITH_KNOTS ( ( 4, 4 ),
 ( 2, 2 ),
 ( 0.000000000000000000, 1.000000000000000000 ),
 ( 0.000000000000000000, 1.000000000000000000 ),
 .UNSPECIFIED. ) 
 GEOMETRIC_REPRESENTATION_ITEM ( )  RATIONAL_B_SPLINE_SURFACE ( (
 ( 1.000000000000000000, 1.000000000000000000),
 ( 0.6386103224230302855, 0.9954351624131538845),
 ( 0.6386103224230302855, 0.9954351624131538845),
 ( 1.000000000000000000, 1.000000000000000000) ) ) 
 REPRESENTATION_ITEM ( '' )  SURFACE ( )  );
#5898 = CARTESIAN_POINT ( 'NONE',  ( 109.1592201516379674, -0.007845213074654437332, 0.0005146241775982539042 ) ) ;
#5899 = VERTEX_POINT ( 'NONE', #4807 ) ;
#5900 = CARTESIAN_POINT ( 'NONE',  ( -1.463510566862834539, 38.76366072687779507, -25.15876608740827436 ) ) ;
#5901 = B_SPLINE_CURVE_WITH_KNOTS ( 'NONE', 3,
 ( #23455, #28162, #12903, #1558, #26292, #17504, #2101, #14650 ),
 .UNSPECIFIED., .F., .F.,
 ( 4, 2, 2, 4 ),
 ( 0.000000000000000000, 0.002761524886576655416, 0.005523049773153310832, 0.01104609954630661646 ),
 .UNSPECIFIED. ) ;
#5902 = EDGE_LOOP ( 'NONE', ( #14282, #18232, #26452, #12564 ) ) ;
#5903 = ADVANCED_FACE ( 'NONE', ( #22375 ), #7755, .F. ) ;
#5904 = EDGE_CURVE ( 'NONE', #7408, #12561, #27822, .T. ) ;
#5905 = EDGE_LOOP ( 'NONE', ( #17236, #19187, #121, #12751 ) ) ;
#5906 = FACE_OUTER_BOUND ( 'NONE', #11611, .T. ) ;
#5907 =( BOUNDED_SURFACE ( )  B_SPLINE_SURFACE ( 3, 1, ( 
 ( #10239, #14384 ),
 ( #19001, #6194 ),
 ( #16972, #1705 ),
 ( #10086, #25763 ) ),
 .UNSPECIFIED., .F., .F., .F. ) 
 B_SPLINE_SURFACE_WITH_KNOTS ( ( 4, 4 ),
 ( 2, 2 ),
 ( 0.000000000000000000, 1.000000000000000000 ),
 ( 0.000000000000000000, 1.000000000000000000 ),
 .UNSPECIFIED. ) 
 GEOMETRIC_REPRESENTATION_ITEM ( )  RATIONAL_B_SPLINE_SURFACE ( (
 ( 1.000000000000000000, 1.000000000000000000),
 ( 0.7789835883360578528, 0.9689951854195403280),
 ( 0.7789835883360578528, 0.9689951854195403280),
 ( 1.000000000000000000, 1.000000000000000000) ) ) 
 REPRESENTATION_ITEM ( '' )  SURFACE ( )  );
#5908 = CARTESIAN_POINT ( 'NONE',  ( -28.13707043255157103, 6.342158660427315020, 22.00298671236732773 ) ) ;
#5909 = FACE_OUTER_BOUND ( 'NONE', #16991, .T. ) ;
#5910 = ADVANCED_FACE ( 'NONE', ( #23381 ), #4617, .F. ) ;
#5911 = CARTESIAN_POINT ( 'NONE',  ( -8.786685647604890903, 52.67761315067286176, -9.545808661480789326 ) ) ;
#5912 = CARTESIAN_POINT ( 'NONE',  ( 109.1586900883932856, -0.0001010081143976501722, -0.007137750914550312215 ) ) ;
#5913 = CARTESIAN_POINT ( 'NONE',  ( 1.833691583653523027, 141.8642667235908164, 30.51806994139646534 ) ) ;
#5914 = CARTESIAN_POINT ( 'NONE',  ( -1.583189561560253589, 46.33203782964461936, -2.490696082060032790 ) ) ;
#5915 = CARTESIAN_POINT ( 'NONE',  ( -1.323830074806774615, -16.42382241777507090, 43.04593525292983003 ) ) ;
#5916 = CARTESIAN_POINT ( 'NONE',  ( -1.463510566862831208, -46.14841196428341874, -2.430838777910016901 ) ) ;
#5917 = ORIENTED_EDGE ( 'NONE', *, *, #10156, .T. ) ;
#5918 = ORIENTED_EDGE ( 'NONE', *, *, #16381, .F. ) ;
#5919 = CARTESIAN_POINT ( 'NONE',  ( 28.37603512858448340, 86.45299531409462190, 75.42810021528123343 ) ) ;
#5920 = CARTESIAN_POINT ( 'NONE',  ( 109.1624594426973118, -0.006914244825467878892, -0.01438905500501944622 ) ) ;
#5921 = CARTESIAN_POINT ( 'NONE',  ( 9.884929003653608603, 135.7578851563885962, 65.04493172071525464 ) ) ;
#5922 = DIRECTION ( 'NONE',  ( 0.000000000000000000, 0.000000000000000000, -1.000000000000000000 ) ) ;
#5923 = CARTESIAN_POINT ( 'NONE',  ( -1.619063947482197729, 11.94059994246222622, 44.80407745103770623 ) ) ;
#5924 = CARTESIAN_POINT ( 'NONE',  ( 109.1589550718175161, -0.004900004919101272859, 0.005777059646713168448 ) ) ;
#5925 = FACE_OUTER_BOUND ( 'NONE', #2870, .T. ) ;
#5926 = ORIENTED_EDGE ( 'NONE', *, *, #7937, .F. ) ;
#5927 = FACE_OUTER_BOUND ( 'NONE', #27002, .T. ) ;
#5928 = CARTESIAN_POINT ( 'NONE',  ( 32.73300124599769134, -51.32617430724849328, -105.8473486001054198 ) ) ;
#5929 = CARTESIAN_POINT ( 'NONE',  ( 25.64670758986458310, -11.30712635241913766, -112.3434365398309751 ) ) ;
#5930 = DIRECTION ( 'NONE',  ( 0.000000000000000000, 1.000000000000000000, 3.122502256758243698E-15 ) ) ;
#5931 = CARTESIAN_POINT ( 'NONE',  ( 32.73300124599735739, -62.10906484417306928, 99.90245962373816724 ) ) ;
#5932 = VERTEX_POINT ( 'NONE', #7992 ) ;
#5933 = CARTESIAN_POINT ( 'NONE',  ( -4.162674018437135359, 31.44946543094296487, -37.46098494546600932 ) ) ;
#5934 = CARTESIAN_POINT ( 'NONE',  ( 10.93730112725990011, -115.5857507957697976, -97.44200844886394464 ) ) ;
#5935 = VERTEX_POINT ( 'NONE', #18906 ) ;
#5936 = VECTOR ( 'NONE', #19344, 1000.000000000000114 ) ;
#5937 = EDGE_LOOP ( 'NONE', ( #21485, #14636, #20600, #20711 ) ) ;
#5938 = VECTOR ( 'NONE', #25326, 1000.000000000000000 ) ;
#5939 = VERTEX_POINT ( 'NONE', #16455 ) ;
#5940 = EDGE_CURVE ( 'NONE', #15925, #2427, #6989, .T. ) ;
#5941 = CARTESIAN_POINT ( 'NONE',  ( 1.833485406944043827, 29.64752363041542083, 142.0485807715646729 ) ) ;
#5942 = CARTESIAN_POINT ( 'NONE',  ( -7.078251931573400491, -20.86696228105191864, 47.71415099571825635 ) ) ;
#5943 =( BOUNDED_SURFACE ( )  B_SPLINE_SURFACE ( 3, 1, ( 
 ( #3294, #841 ),
 ( #7479, #12077 ),
 ( #27462, #3148 ),
 ( #20695, #558 ) ),
 .UNSPECIFIED., .F., .F., .F. ) 
 B_SPLINE_SURFACE_WITH_KNOTS ( ( 4, 4 ),
 ( 2, 2 ),
 ( 0.000000000000000000, 1.000000000000000000 ),
 ( 0.000000000000000000, 1.000000000000000000 ),
 .UNSPECIFIED. ) 
 GEOMETRIC_REPRESENTATION_ITEM ( )  RATIONAL_B_SPLINE_SURFACE ( (
 ( 1.000000000000000000, 1.000000000000000000),
 ( 0.9934239774497838349, 0.8357310067453913582),
 ( 0.9934239774497838349, 0.8357310067453913582),
 ( 1.000000000000000000, 1.000000000000000000) ) ) 
 REPRESENTATION_ITEM ( '' )  SURFACE ( )  );
#5944 = ADVANCED_FACE ( 'NONE', ( #1619 ), #1480, .F. ) ;
#5945 = CARTESIAN_POINT ( 'NONE',  ( 1.833750490713699444, 30.43107162406064603, -141.8829662951649482 ) ) ;
#5946 = EDGE_CURVE ( 'NONE', #710, #23103, #14279, .T. ) ;
#5947 = B_SPLINE_CURVE_WITH_KNOTS ( 'NONE', 3,
 ( #8625, #24177, #26046, #23631, #21441, #26316 ),
 .UNSPECIFIED., .F., .F.,
 ( 4, 2, 4 ),
 ( 5.135960789613967459E-18, 0.0004335151646191499485, 0.0008670303292382946928 ),
 .UNSPECIFIED. ) ;
#5948 = CARTESIAN_POINT ( 'NONE',  ( -18.41936578851711559, 29.33493038358074045, -30.66520733838660462 ) ) ;
#5949 = ORIENTED_EDGE ( 'NONE', *, *, #3654, .T. ) ;
#5950 = CARTESIAN_POINT ( 'NONE',  ( 1.833485406944043827, 59.50871042846404180, -132.3460930279885019 ) ) ;
#5951 = CARTESIAN_POINT ( 'NONE',  ( -20.20700224038492010, 18.19058640100223556, -23.35150625415664649 ) ) ;
#5952 = CARTESIAN_POINT ( 'NONE',  ( 25.98552792386799482, -110.4352299692911572, 24.57669147553951206 ) ) ;
#5953 = CARTESIAN_POINT ( 'NONE',  ( 109.1778270068192853, 0.008646067828082840481, 0.003465086990435519224 ) ) ;
#5954 = CARTESIAN_POINT ( 'NONE',  ( 10.93730112725990011, -151.0983828010092225, 4.928439153519769356 ) ) ;
#5955 = CARTESIAN_POINT ( 'NONE',  ( 25.64681081121879203, 75.24277141833607629, -84.18689316039970549 ) ) ;
#5956 = CARTESIAN_POINT ( 'NONE',  ( 10.93730112726005999, 128.3908183996603327, -79.81734490845792607 ) ) ;
#5957 = CARTESIAN_POINT ( 'NONE',  ( -55.25719721206881729, -0.007063345920780820901, -0.008651607285661404648 ) ) ;
#5958 = CARTESIAN_POINT ( 'NONE',  ( 109.1592201516379674, 0.0003082430541934987381, -0.007856029051018018419 ) ) ;
#5959 = CARTESIAN_POINT ( 'NONE',  ( 25.70243777736189728, 12.53519966262632224, -112.2504268534933232 ) ) ;
#5960 = VERTEX_POINT ( 'NONE', #19048 ) ;
#5961 = VERTEX_POINT ( 'NONE', #18616 ) ;
#5962 = CARTESIAN_POINT ( 'NONE',  ( -1.464342487929850778, 38.76467504336618219, 25.15873223207648834 ) ) ;
#5964 = ORIENTED_EDGE ( 'NONE', *, *, #21843, .T. ) ;
#5963 = FACE_OUTER_BOUND ( 'NONE', #18084, .T. ) ;
#5965 = EDGE_LOOP ( 'NONE', ( #16817, #18474, #12084, #435 ) ) ;
#5966 = ORIENTED_EDGE ( 'NONE', *, *, #24256, .F. ) ;
#5967 = VERTEX_POINT ( 'NONE', #23523 ) ;
#5968 = ADVANCED_FACE ( 'NONE', ( #14438 ), #23394, .F. ) ;
#5969 = DIRECTION ( 'NONE',  ( 0.000000000000000000, -1.000000000000000000, 0.000000000000000000 ) ) ;
#5970 = B_SPLINE_CURVE_WITH_KNOTS ( 'NONE', 3,
 ( #17265, #6342, #25517, #15821, #19849, #24329 ),
 .UNSPECIFIED., .F., .F.,
 ( 4, 2, 4 ),
 ( 1.144950348284594810E-17, 0.0006311636237756862835, 0.001262327247551361074 ),
 .UNSPECIFIED. ) ;
#5971 = CARTESIAN_POINT ( 'NONE',  ( -23.77929240705205771, -25.06639637888440220, -26.20227034809546041 ) ) ;
#5972 = DIRECTION ( 'NONE',  ( -0.5946245182733607137, -0.08110646981859605253, 0.7999021332774021165 ) ) ;
#5973 = CARTESIAN_POINT ( 'NONE',  ( -20.20612092514785019, 27.77903665678167400, -10.22177639105870384 ) ) ;
#5974 = CARTESIAN_POINT ( 'NONE',  ( 26.11404676487259024, 74.91683232331092768, -84.89295829319416953 ) ) ;
#5975 = CARTESIAN_POINT ( 'NONE',  ( 2.433796855181205476, 142.6247129145651797, -28.83182736670396196 ) ) ;
#5976 =( BOUNDED_SURFACE ( )  B_SPLINE_SURFACE ( 3, 1, ( 
 ( #20233, #22125 ),
 ( #17924, #7021 ),
 ( #15482, #244 ),
 ( #17791, #9029 ) ),
 .UNSPECIFIED., .F., .F., .F. ) 
 B_SPLINE_SURFACE_WITH_KNOTS ( ( 4, 4 ),
 ( 2, 2 ),
 ( 0.000000000000000000, 1.000000000000000000 ),
 ( 0.000000000000000000, 1.000000000000000000 ),
 .UNSPECIFIED. ) 
 GEOMETRIC_REPRESENTATION_ITEM ( )  RATIONAL_B_SPLINE_SURFACE ( (
 ( 1.000000000000000000, 1.000000000000000000),
 ( 0.7789835883360576307, 0.9689951854195403280),
 ( 0.7789835883360576307, 0.9689951854195403280),
 ( 1.000000000000000000, 1.000000000000000000) ) ) 
 REPRESENTATION_ITEM ( '' )  SURFACE ( )  );
#5977 = CARTESIAN_POINT ( 'NONE',  ( 1.832998868059890096, -73.01698022778269603, -125.4013017422238363 ) ) ;
#5978 = CARTESIAN_POINT ( 'NONE',  ( -1.113427685306998649, -44.18561238466747199, -12.28784199929917875 ) ) ;
#5979 = DIRECTION ( 'NONE',  ( 0.5946245182733607137, 0.3243201896541541562, 0.7356888587241667832 ) ) ;
#5980 = ORIENTED_EDGE ( 'NONE', *, *, #135, .F. ) ;
#5981 = VERTEX_POINT ( 'NONE', #10137 ) ;
#5982 = CARTESIAN_POINT ( 'NONE',  ( 25.64704443564077252, -107.3436266109710999, -35.01840413910241523 ) ) ;
#5984 = FACE_OUTER_BOUND ( 'NONE', #8722, .T. ) ;
#5983 = CARTESIAN_POINT ( 'NONE',  ( 109.1586059443104944, 0.001014167950289969608, 0.007001002073869790586 ) ) ;
#5985 = CARTESIAN_POINT ( 'NONE',  ( 10.93730112725932635, 0.000000000000000000, 0.000000000000000000 ) ) ;
#5986 = CARTESIAN_POINT ( 'NONE',  ( 14.74894986621300319, -1.023413983156987147E-16, 2.558534957892467869E-17 ) ) ;
#5987 = CARTESIAN_POINT ( 'NONE',  ( 25.70243777736189017, 91.80600962488489358, -65.79472741891171950 ) ) ;
#5988 = ORIENTED_EDGE ( 'NONE', *, *, #491, .F. ) ;
#5989 = CARTESIAN_POINT ( 'NONE',  ( -55.24390624410018802, -0.007503127514281482044, 0.007245494385991411469 ) ) ;
#5990 = CARTESIAN_POINT ( 'NONE',  ( -55.24300891470650754, 0.005486913146700745682, -0.008142823778062297305 ) ) ;
#5991 = B_SPLINE_CURVE_WITH_KNOTS ( 'NONE', 3,
 ( #2956, #7570, #14301, #16326, #16624, #25121, #14156, #18773, #18924, #22978 ),
 .UNSPECIFIED., .F., .F.,
 ( 4, 2, 2, 2, 4 ),
 ( 1.563658610346375379E-18, 0.0003346267210630954943, 0.0006692534421261893624, 0.001003880163189283230, 0.001338506884252377207 ),
 .UNSPECIFIED. ) ;
#5992 = CARTESIAN_POINT ( 'NONE',  ( 30.58324630866355420, 119.0579156359858786, 21.27395054437283761 ) ) ;
#5993 = VERTEX_POINT ( 'NONE', #21340 ) ;
#5994 = ORIENTED_EDGE ( 'NONE', *, *, #15572, .T. ) ;
#5995 = B_SPLINE_CURVE_WITH_KNOTS ( 'NONE', 3,
 ( #20152, #293, #2447, #585, #439, #9226, #20586 ),
 .UNSPECIFIED., .F., .F.,
 ( 4, 3, 4 ),
 ( 0.000000000000000000, 0.02398743853561337638, 0.04000277880656218088 ),
 .UNSPECIFIED. ) ;
#5996 = CARTESIAN_POINT ( 'NONE',  ( 1.831572820252008738, -29.20415387690465181, -142.1425225354583119 ) ) ;
#5997 = ADVANCED_FACE ( 'NONE', ( #12146 ), #18655, .T. ) ;
#5998 = ORIENTED_EDGE ( 'NONE', *, *, #21461, .T. ) ;
#5999 = ORIENTED_EDGE ( 'NONE', *, *, #7641, .T. ) ;
#6000 = EDGE_CURVE ( 'NONE', #5518, #9315, #2547, .T. ) ;
#6001 = AXIS2_PLACEMENT_3D ( 'NONE', #27226, #7541, #16297 ) ;
#6002 = EDGE_CURVE ( 'NONE', #531, #21908, #6627, .T. ) ;
#6003 = CARTESIAN_POINT ( 'NONE',  ( 2.430230287190592531, -16.65331920325641590, -144.5585181921887568 ) ) ;
#6004 = ORIENTED_EDGE ( 'NONE', *, *, #18657, .F. ) ;
#6005 = VECTOR ( 'NONE', #15139, 1000.000000000000114 ) ;
#6006 = CARTESIAN_POINT ( 'NONE',  ( 32.73300124599738581, -55.46353551261936587, -103.7392577722181812 ) ) ;
#6007 = CARTESIAN_POINT ( 'NONE',  ( 10.93730112725972425, -65.95960219663204782, 136.0306644680981094 ) ) ;
#6008 = CIRCLE ( 'NONE', #3237, 53.53553390275978785 ) ;
#6009 = CARTESIAN_POINT ( 'NONE',  ( 32.73300124599738581, 108.9684813982494092, -44.31599526637845798 ) ) ;
#6010 = CARTESIAN_POINT ( 'NONE',  ( 1.893872463202029843, 126.1771883101046825, -71.74819926215046451 ) ) ;
#6011 = CARTESIAN_POINT ( 'NONE',  ( 109.1778270068192853, -0.009307953841270272949, 0.0003511581237513249575 ) ) ;
#6012 = CARTESIAN_POINT ( 'NONE',  ( 109.1778270068192853, -0.0003511581237570398956, 0.009307953841262543021 ) ) ;
#6013 = CARTESIAN_POINT ( 'NONE',  ( 25.65782528836479770, -46.45532072021256198, 102.9197507294674523 ) ) ;
#6014 = CARTESIAN_POINT ( 'NONE',  ( 1.833485406944043827, 125.4007332306545379, 73.01664920993009389 ) ) ;
#6015 = B_SPLINE_CURVE_WITH_KNOTS ( 'NONE', 3,
 ( #22805, #20616, #16450, #3489 ),
 .UNSPECIFIED., .F., .F.,
 ( 4, 4 ),
 ( 1.904170172768910460E-16, 0.001982023823822945917 ),
 .UNSPECIFIED. ) ;
#6016 = CARTESIAN_POINT ( 'NONE',  ( 26.04756280548352976, -103.8403168215172627, -45.01666824410871470 ) ) ;
#6018 = CARTESIAN_POINT ( 'NONE',  ( -19.53423201713129842, 4.045852573675910766E-15, -28.92774122539760384 ) ) ;
#6017 = CARTESIAN_POINT ( 'NONE',  ( -20.20700224038492010, -16.58740185276728241, -24.51628800869040958 ) ) ;
#6019 = CARTESIAN_POINT ( 'NONE',  ( -1.619063947482197729, 29.22875152547757338, -35.99532424477389725 ) ) ;
#6020 =( BOUNDED_SURFACE ( )  B_SPLINE_SURFACE ( 3, 1, ( 
 ( #1227, #20515 ),
 ( #801, #944 ),
 ( #10026, #18788 ),
 ( #9583, #7586 ) ),
 .UNSPECIFIED., .F., .F., .F. ) 
 B_SPLINE_SURFACE_WITH_KNOTS ( ( 4, 4 ),
 ( 2, 2 ),
 ( 0.000000000000000000, 1.000000000000000000 ),
 ( 0.000000000000000000, 1.000000000000000000 ),
 .UNSPECIFIED. ) 
 GEOMETRIC_REPRESENTATION_ITEM ( )  RATIONAL_B_SPLINE_SURFACE ( (
 ( 1.000000000000000000, 1.000000000000000000),
 ( 0.7789835883360578528, 0.9689951854195403280),
 ( 0.7789835883360578528, 0.9689951854195403280),
 ( 1.000000000000000000, 1.000000000000000000) ) ) 
 REPRESENTATION_ITEM ( '' )  SURFACE ( )  );
#6021 = ORIENTED_EDGE ( 'NONE', *, *, #13771, .T. ) ;
#6022 = ORIENTED_EDGE ( 'NONE', *, *, #11157, .T. ) ;
#6023 = CARTESIAN_POINT ( 'NONE',  ( -5.986830583229487246, -50.53158596890438758, 4.559539818181663762 ) ) ;
#6024 = LINE ( 'NONE', #23591, #27268 ) ;
#6025 = CARTESIAN_POINT ( 'NONE',  ( -2.265401668238153032, -45.46007138824032978, 11.98901689611089516 ) ) ;
#6026 = CARTESIAN_POINT ( 'NONE',  ( 2.263178607246699503, 125.2099936970377740, -73.90841395012451187 ) ) ;
#6027 = FACE_OUTER_BOUND ( 'NONE', #8960, .T. ) ;
#6028 = ORIENTED_EDGE ( 'NONE', *, *, #3997, .F. ) ;
#6029 = CARTESIAN_POINT ( 'NONE',  ( 26.11404676487257603, -107.3263591096427945, -36.06104232266560672 ) ) ;
#6030 = CARTESIAN_POINT ( 'NONE',  ( 1.834118845439484335, 125.7578880615045023, 72.40084790867372533 ) ) ;
#6031 = ORIENTED_EDGE ( 'NONE', *, *, #7257, .T. ) ;
#6032 = FACE_OUTER_BOUND ( 'NONE', #5350, .T. ) ;
#6033 = CARTESIAN_POINT ( 'NONE',  ( 109.1589550718175161, 0.001793588804100394816, 0.007359857714025730933 ) ) ;
#6034 = EDGE_CURVE ( 'NONE', #17270, #8158, #82, .T. ) ;
#6035 = DIRECTION ( 'NONE',  ( -1.000000000000000000, 6.938893903907226837E-18, -1.734723475976806709E-18 ) ) ;
#6036 = VECTOR ( 'NONE', #21582, 1000.000000000000000 ) ;
#6037 = B_SPLINE_CURVE_WITH_KNOTS ( 'NONE', 3,
 ( #14206, #9353, #557, #7329, #988, #22445 ),
 .UNSPECIFIED., .F., .F.,
 ( 4, 2, 4 ),
 ( 9.659140056172959483E-18, 0.0006311571484586091501, 0.001262314296917208759 ),
 .UNSPECIFIED. ) ;
#6038 = CARTESIAN_POINT ( 'NONE',  ( -55.25297051322618813, -0.006313402748431807057, -0.01354497706059512932 ) ) ;
#6039 = CARTESIAN_POINT ( 'NONE',  ( -25.21435515916043357, -16.39063784838764093, -30.48034229288631991 ) ) ;
#6040 = CARTESIAN_POINT ( 'NONE',  ( -7.078251931573400491, 11.16394717458747898, 50.86685171665398997 ) ) ;
#6041 = ORIENTED_EDGE ( 'NONE', *, *, #19615, .T. ) ;
#6042 = CARTESIAN_POINT ( 'NONE',  ( -55.24390624410018802, -0.001811362924362171613, 0.01027195578988007209 ) ) ;
#6043 = EDGE_CURVE ( 'NONE', #15548, #21594, #12255, .T. ) ;
#6044 = COLOUR_RGB ( '',0.7921568627450980005, 0.8196078431372548767, 0.9333333333333333481 ) ;
#6045 = EDGE_CURVE ( 'NONE', #14195, #20657, #20670, .T. ) ;
#6046 = ORIENTED_EDGE ( 'NONE', *, *, #6162, .T. ) ;
#6047 = CARTESIAN_POINT ( 'NONE',  ( 2.433796855181219243, -142.0211193075558356, 31.67151202412923894 ) ) ;
#6048 = CARTESIAN_POINT ( 'NONE',  ( 32.73300124599740002, -8.473903470905288060, -117.3295799645430151 ) ) ;
#6049 = VERTEX_POINT ( 'NONE', #13809 ) ;
#6050 = CARTESIAN_POINT ( 'NONE',  ( 25.64681081121879203, -103.3177883989776547, -45.54494737132326776 ) ) ;
#6051 = LINE ( 'NONE', #5908, #2312 ) ;
#6052 = CARTESIAN_POINT ( 'NONE',  ( -1.050231094221201644, -13.91061116148162391, 43.63617436699752261 ) ) ;
#6053 = CIRCLE ( 'NONE', #19799, 53.53553390275978785 ) ;
#6054 = CARTESIAN_POINT ( 'NONE',  ( -20.24399999263414429, 18.44171895251396265, -23.20123049637371793 ) ) ;
#6055 = CARTESIAN_POINT ( 'NONE',  ( 1.833603222531976273, 138.1443021179086941, -44.41798579679396397 ) ) ;
#6056 = CARTESIAN_POINT ( 'NONE',  ( 2.433796855181205476, 43.58222566461644476, 138.8296532063089614 ) ) ;
#6057 = B_SPLINE_CURVE_WITH_KNOTS ( 'NONE', 3,
 ( #25324, #1271, #16836, #1412, #5893, #12492, #13318, #21694 ),
 .UNSPECIFIED., .F., .F.,
 ( 4, 2, 2, 4 ),
 ( 2.211348276820754320E-16, 0.002761568181852864200, 0.005523136363705507222, 0.01104627272741079066 ),
 .UNSPECIFIED. ) ;
#6058 = CARTESIAN_POINT ( 'NONE',  ( -1.155001620486257208, -28.62773628245643209, 35.88346938217584636 ) ) ;
#6059 = CARTESIAN_POINT ( 'NONE',  ( 60.46576798286869803, -4.195655488513964285E-16, 1.048913872128491071E-16 ) ) ;
#6060 = CARTESIAN_POINT ( 'NONE',  ( 25.64681081121879203, 34.49579773461926635, -107.5125461021399218 ) ) ;
#6061 = ORIENTED_EDGE ( 'NONE', *, *, #350, .F. ) ;
#6062 = AXIS2_PLACEMENT_3D ( 'NONE', #11020, #6284, #19781 ) ;
#6063 = ORIENTED_EDGE ( 'NONE', *, *, #189, .F. ) ;
#6064 = CARTESIAN_POINT ( 'NONE',  ( 26.11404676487256893, -110.9778746459748362, 22.43340081644731043 ) ) ;
#6065 = CARTESIAN_POINT ( 'NONE',  ( 1.833485406944043827, 59.50871042846404180, -132.3460930279885019 ) ) ;
#6066 = CARTESIAN_POINT ( 'NONE',  ( 25.64681081121879203, 34.49579773461785948, 107.5125461021403765 ) ) ;
#6067 = LINE ( 'NONE', #25357, #25323 ) ;
#6068 = CARTESIAN_POINT ( 'NONE',  ( -1.323830074806773727, 43.04593525292991529, 16.42382241777492524 ) ) ;
#6069 = CARTESIAN_POINT ( 'NONE',  ( 32.73300124599737160, -84.80615050150427692, 81.52272205837169849 ) ) ;
#6070 = CARTESIAN_POINT ( 'NONE',  ( 2.433796855181205476, 98.43889364294005873, -107.1581411821775305 ) ) ;
#6071 = ORIENTED_EDGE ( 'NONE', *, *, #18094, .F. ) ;
#6072 = CARTESIAN_POINT ( 'NONE',  ( 2.430230287190589422, 107.1617224697477297, -98.44218333480664285 ) ) ;
#6073 = CARTESIAN_POINT ( 'NONE',  ( -1.031422197589716205, -15.60268798220608844, 43.06660437151324317 ) ) ;
#6074 = CARTESIAN_POINT ( 'NONE',  ( 25.64708010899964918, 23.42206246795159430, -110.4552579818683427 ) ) ;
#6075 = ADVANCED_FACE ( 'NONE', ( #1008 ), #14975, .T. ) ;
#6076 = EDGE_CURVE ( 'NONE', #2443, #7281, #718, .T. ) ;
#6077 = DIRECTION ( 'NONE',  ( 0.000000000000000000, 5.223019709708233256E-21, -1.000000000000000000 ) ) ;
#6078 = CARTESIAN_POINT ( 'NONE',  ( -28.41354790283022069, -23.16239616762932130, -1.249099604786995332 ) ) ;
#6079 = EDGE_LOOP ( 'NONE', ( #16994, #12421, #3435, #13684 ) ) ;
#6081 = EDGE_CURVE ( 'NONE', #22569, #14235, #17587, .T. ) ;
#6080 = CARTESIAN_POINT ( 'NONE',  ( -8.786685647604887350, -38.68584556812326980, -37.00619870957918778 ) ) ;
#6082 = B_SPLINE_CURVE_WITH_KNOTS ( 'NONE', 3,
 ( #13724, #15587, #7135, #17890 ),
 .UNSPECIFIED., .F., .F.,
 ( 4, 4 ),
 ( 5.988792064294042516E-16, 0.008383748772660088583 ),
 .UNSPECIFIED. ) ;
#6083 = CARTESIAN_POINT ( 'NONE',  ( -4.178947244162637631, -11.88256963646706410, 47.46809051147732816 ) ) ;
#6084 = VERTEX_POINT ( 'NONE', #3169 ) ;
#6085 = AXIS2_PLACEMENT_3D ( 'NONE', #16129, #26917, #7228 ) ;
#6086 = B_SPLINE_CURVE_WITH_KNOTS ( 'NONE', 3,
 ( #16915, #3950, #13007, #12580, #23970, #25704, #17041 ),
 .UNSPECIFIED., .F., .F.,
 ( 4, 3, 4 ),
 ( 0.000000000000000000, 0.009512539173626361963, 0.02506242213020844212 ),
 .UNSPECIFIED. ) ;
#6087 = EDGE_CURVE ( 'NONE', #12327, #4924, #13954, .T. ) ;
#6088 = ORIENTED_EDGE ( 'NONE', *, *, #14221, .T. ) ;
#6089 = ORIENTED_EDGE ( 'NONE', *, *, #3755, .T. ) ;
#6090 = VECTOR ( 'NONE', #9449, 1000.000000000000114 ) ;
#6091 = CARTESIAN_POINT ( 'NONE',  ( 32.73300124599738581, -28.19767303745521758, -114.2056417606550696 ) ) ;
#6092 = CARTESIAN_POINT ( 'NONE',  ( 16.75465622695631041, -112.2763423369177076, -87.30527857298577032 ) ) ;
#6093 = B_SPLINE_CURVE_WITH_KNOTS ( 'NONE', 3,
 ( #28437, #10907, #13618, #8602, #4274, #17367, #26156, #6447, #17511, #13058 ),
 .UNSPECIFIED., .F., .F.,
 ( 4, 3, 3, 4 ),
 ( 3.816391647148975608E-17, 0.0002669559177086190931, 0.0005339118354150969954, 0.001067817517169159913 ),
 .UNSPECIFIED. ) ;
#6094 = CARTESIAN_POINT ( 'NONE',  ( -1.583189561560252701, 16.68617981233703063, -43.29471907393747898 ) ) ;
#6095 = CARTESIAN_POINT ( 'NONE',  ( -55.24390624410018802, -0.009374879212966679906, -0.004572280736703028189 ) ) ;
#6096 = VERTEX_POINT ( 'NONE', #24642 ) ;
#6097 = CARTESIAN_POINT ( 'NONE',  ( 119.2224693531408803, 0.000000000000000000, 0.000000000000000000 ) ) ;
#6098 = DIRECTION ( 'NONE',  ( 0.000000000000000000, 0.000000000000000000, 1.000000000000000000 ) ) ;
#6099 = CARTESIAN_POINT ( 'NONE',  ( -8.786685647604894456, 7.199674155859698388, 53.04920435127174017 ) ) ;
#6100 = VECTOR ( 'NONE', #20103, 1000.000000000000341 ) ;
#6101 = CARTESIAN_POINT ( 'NONE',  ( 1.834118845439484335, 144.3336252355296949, 14.99112450600294721 ) ) ;
#6102 = CARTESIAN_POINT ( 'NONE',  ( 26.11404676487259024, 24.64483677384848903, 110.5078194225162207 ) ) ;
#6103 = CARTESIAN_POINT ( 'NONE',  ( 109.1624594426973260, 0.01318243916934103317, -0.009004164758061436805 ) ) ;
#6104 = EDGE_CURVE ( 'NONE', #16608, #7408, #24109, .T. ) ;
#6105 = CARTESIAN_POINT ( 'NONE',  ( 28.37599760073042532, 108.5491283158102078, 37.15642189426440467 ) ) ;
#6106 = DIRECTION ( 'NONE',  ( -1.000000000000000000, 0.000000000000000000, 0.000000000000000000 ) ) ;
#6107 = CARTESIAN_POINT ( 'NONE',  ( -5.986830583229487246, -26.01297580803291964, 43.56094206392985058 ) ) ;
#6108 = VERTEX_POINT ( 'NONE', #20869 ) ;
#6109 = ORIENTED_EDGE ( 'NONE', *, *, #16965, .F. ) ;
#6111 = EDGE_CURVE ( 'NONE', #12390, #3917, #11398, .T. ) ;
#6110 = CARTESIAN_POINT ( 'NONE',  ( 26.11404676487259024, -24.64483677384768967, -110.5078194225163912 ) ) ;
#6112 = CARTESIAN_POINT ( 'NONE',  ( 26.04756280548353686, 36.02883009343639031, 107.2904246402795962 ) ) ;
#6113 = EDGE_LOOP ( 'NONE', ( #4661, #3823, #8152, #20027 ) ) ;
#6114 = EDGE_LOOP ( 'NONE', ( #5926, #22735, #27924, #13100 ) ) ;
#6115 = VERTEX_POINT ( 'NONE', #8203 ) ;
#6116 = CIRCLE ( 'NONE', #4253, 37.50000000000001421 ) ;
#6117 = CARTESIAN_POINT ( 'NONE',  ( 10.93730112725945247, 97.44200844886275092, 115.5857507957704087 ) ) ;
#6118 = AXIS2_PLACEMENT_3D ( 'NONE', #13720, #774, #6986 ) ;
#6119 = CARTESIAN_POINT ( 'NONE',  ( 25.73574536432417048, -83.41179791497809504, -76.18908113044840036 ) ) ;
#6120 = CARTESIAN_POINT ( 'NONE',  ( 109.1586900883932856, 0.001582822706032828994, 0.006960773163852194793 ) ) ;
#6121 = CARTESIAN_POINT ( 'NONE',  ( -16.86833981943427929, 5.948101187262172296, 43.82216161736197790 ) ) ;
#6122 = LINE ( 'NONE', #17308, #13913 ) ;
#6123 = B_SPLINE_CURVE_WITH_KNOTS ( 'NONE', 3,
 ( #18360, #7603, #16068, #7025 ),
 .UNSPECIFIED., .F., .F.,
 ( 4, 4 ),
 ( 0.000000000000000000, 0.01077107196513893937 ),
 .UNSPECIFIED. ) ;
#6124 = CARTESIAN_POINT ( 'NONE',  ( -20.90916690077966322, -5.322316104228261402, -39.20864005633521998 ) ) ;
#6125 = B_SPLINE_CURVE_WITH_KNOTS ( 'NONE', 3,
 ( #9189, #22443, #128, #5008, #26596, #13352, #17537, #2414 ),
 .UNSPECIFIED., .F., .F.,
 ( 4, 2, 2, 4 ),
 ( 3.469446951953614189E-18, 0.0002429592666046752423, 0.0004859185332093470151, 0.0009718370664186726715 ),
 .UNSPECIFIED. ) ;
#6126 = FACE_OUTER_BOUND ( 'NONE', #27063, .T. ) ;
#6127 = CARTESIAN_POINT ( 'NONE',  ( 109.1586900883932856, 0.001582822706032828994, 0.006960773163852194793 ) ) ;
#6128 = CARTESIAN_POINT ( 'NONE',  ( 10.93730112725978287, -133.3192575531804209, 71.28103789254889477 ) ) ;
#6129 = ORIENTED_EDGE ( 'NONE', *, *, #16347, .T. ) ;
#6130 = ORIENTED_EDGE ( 'NONE', *, *, #19817, .T. ) ;
#6132 = CARTESIAN_POINT ( 'NONE',  ( 25.64681081121879203, -91.59071981940616070, 66.03065707438906884 ) ) ;
#6131 = CARTESIAN_POINT ( 'NONE',  ( 25.64708010899963853, 112.9112661935490252, -0.05470523945908801339 ) ) ;
#6133 = ADVANCED_FACE ( 'NONE', ( #1837 ), #5907, .F. ) ;
#6134 = CARTESIAN_POINT ( 'NONE',  ( 25.64681081121880624, -102.9795863647025556, -46.30456157731431688 ) ) ;
#6135 = DIRECTION ( 'NONE',  ( 0.000000000000000000, 0.000000000000000000, 1.000000000000000000 ) ) ;
#6136 = CARTESIAN_POINT ( 'NONE',  ( -9.156249394959713683, 38.17928057392048657, 38.89149400288364689 ) ) ;
#6137 =( GEOMETRIC_REPRESENTATION_CONTEXT ( 3 ) GLOBAL_UNCERTAINTY_ASSIGNED_CONTEXT ( ( #22652 ) ) GLOBAL_UNIT_ASSIGNED_CONTEXT ( ( #24161, #965, #24874 ) ) REPRESENTATION_CONTEXT ( 'NONE', 'WORKASPACE' ) );
#6138 = ORIENTED_EDGE ( 'NONE', *, *, #5793, .F. ) ;
#6139 = VECTOR ( 'NONE', #2344, 1000.000000000000114 ) ;
#6141 = EDGE_CURVE ( 'NONE', #27833, #142, #16557, .T. ) ;
#6140 = CARTESIAN_POINT ( 'NONE',  ( -2.911734481061415636, 25.69892591260268588, -40.13920818157085080 ) ) ;
#6142 = CARTESIAN_POINT ( 'NONE',  ( -20.20700224038492721, 23.35150625415659320, -18.19058640100232438 ) ) ;
#6143 = ORIENTED_EDGE ( 'NONE', *, *, #17857, .T. ) ;
#6144 = ORIENTED_EDGE ( 'NONE', *, *, #27487, .F. ) ;
#6145 = EDGE_CURVE ( 'NONE', #14235, #21908, #7793, .T. ) ;
#6146 = CARTESIAN_POINT ( 'NONE',  ( -20.20700224038492721, 0.9908225410482660589, 29.58392382092671724 ) ) ;
#6147 = ORIENTED_EDGE ( 'NONE', *, *, #22425, .T. ) ;
#6148 = ORIENTED_EDGE ( 'NONE', *, *, #19817, .F. ) ;
#6149 = CARTESIAN_POINT ( 'NONE',  ( 1.833206308920070970, -14.42724735286750892, -144.3905119031281288 ) ) ;
#6150 = ORIENTED_EDGE ( 'NONE', *, *, #778, .T. ) ;
#6151 = CARTESIAN_POINT ( 'NONE',  ( -1.044557008772713402, 1.643388457097889166, -45.76404748504490527 ) ) ;
#6153 =( BOUNDED_SURFACE ( )  B_SPLINE_SURFACE ( 3, 1, ( 
 ( #6925, #28351 ),
 ( #151, #13374 ),
 ( #17701, #26201 ),
 ( #286, #15394 ) ),
 .UNSPECIFIED., .F., .F., .F. ) 
 B_SPLINE_SURFACE_WITH_KNOTS ( ( 4, 4 ),
 ( 2, 2 ),
 ( 0.000000000000000000, 1.000000000000000000 ),
 ( 0.000000000000000000, 1.000000000000000000 ),
 .UNSPECIFIED. ) 
 GEOMETRIC_REPRESENTATION_ITEM ( )  RATIONAL_B_SPLINE_SURFACE ( (
 ( 1.000000000000000000, 1.000000000000000000),
 ( 0.7789835883360578528, 0.9689951854195403280),
 ( 0.7789835883360578528, 0.9689951854195403280),
 ( 1.000000000000000000, 1.000000000000000000) ) ) 
 REPRESENTATION_ITEM ( '' )  SURFACE ( )  );
#6152 = PRODUCT_DEFINITION_FORMATION_WITH_SPECIFIED_SOURCE ( 'ANY', '', #15175, .NOT_KNOWN. ) ;
#6154 = EDGE_CURVE ( 'NONE', #21801, #14085, #25346, .T. ) ;
#6155 = CARTESIAN_POINT ( 'NONE',  ( -1.045287976400365970, 28.14015102489882736, 36.12803364096558312 ) ) ;
#6156 = AXIS2_PLACEMENT_3D ( 'NONE', #27922, #21730, #12661 ) ;
#6157 = CARTESIAN_POINT ( 'NONE',  ( 25.87036335909428075, -110.7910326764400537, -22.53739730344160108 ) ) ;
#6158 = CARTESIAN_POINT ( 'NONE',  ( 2.430230287190592531, -116.8646894862417867, 86.70145658344620188 ) ) ;
#6159 = CARTESIAN_POINT ( 'NONE',  ( 13.36082413113061307, 152.7944199136427414, 6.345145185218579620 ) ) ;
#6160 = CARTESIAN_POINT ( 'NONE',  ( 28.37644542392840563, -4.054996728115051852, 124.2737818798215130 ) ) ;
#6161 = B_SPLINE_CURVE_WITH_KNOTS ( 'NONE', 3,
 ( #16298, #14425, #5360, #11984, #1049, #5661, #23234, #18162, #3485, #618 ),
 .UNSPECIFIED., .F., .F.,
 ( 4, 3, 3, 4 ),
 ( 4.443059973708341306E-17, 0.0002669559177086151358, 0.0005339118354150905986, 0.001067817517169165767 ),
 .UNSPECIFIED. ) ;
#6162 = EDGE_CURVE ( 'NONE', #27119, #2065, #19302, .T. ) ;
#6163 = CARTESIAN_POINT ( 'NONE',  ( 28.37599760073042532, 109.6580863494834688, -33.74340001060989636 ) ) ;
#6164 = CARTESIAN_POINT ( 'NONE',  ( -25.21435515916043357, -34.29329011225959079, -4.655591116594231416 ) ) ;
#6165 = CARTESIAN_POINT ( 'NONE',  ( -1.539763995773680838, 29.16712963492463473, -35.94321074656906490 ) ) ;
#6166 = ORIENTED_EDGE ( 'NONE', *, *, #28005, .F. ) ;
#6167 = ORIENTED_EDGE ( 'NONE', *, *, #26802, .F. ) ;
#6168 = CARTESIAN_POINT ( 'NONE',  ( -1.239374126674604337, 44.48112152129363750, 11.92219841463783503 ) ) ;
#6169 = CARTESIAN_POINT ( 'NONE',  ( 1.833838850855474600, -72.63194208529564833, 125.6242502389383588 ) ) ;
#6170 = CARTESIAN_POINT ( 'NONE',  ( -28.13707043255157103, -14.07296284901345551, -18.06394523322448009 ) ) ;
#6171 = ADVANCED_FACE ( 'NONE', ( #19270 ), #754, .F. ) ;
#6172 = DIRECTION ( 'NONE',  ( -1.000000000000000000, 0.000000000000000000, -0.000000000000000000 ) ) ;
#6173 = CARTESIAN_POINT ( 'NONE',  ( -2.904412668506655582, 2.864640348250632851, -47.56768199507435213 ) ) ;
#6174 = EDGE_LOOP ( 'NONE', ( #18149, #10810, #9898, #4845 ) ) ;
#6175 = CARTESIAN_POINT ( 'NONE',  ( -22.23342874802669300, 20.31166691703127114, -24.24669006619380696 ) ) ;
#6176 = CARTESIAN_POINT ( 'NONE',  ( -1.619063947482201282, 38.92136151114908671, -25.20140673341387227 ) ) ;
#6177 = VECTOR ( 'NONE', #2751, 1000.000000000000227 ) ;
#6178 = VERTEX_POINT ( 'NONE', #1430 ) ;
#6179 = CARTESIAN_POINT ( 'NONE',  ( 25.64681081121880624, -112.3352186517031441, 11.38886654529637887 ) ) ;
#6180 = CARTESIAN_POINT ( 'NONE',  ( 25.64681081121879203, -56.09509703373275613, -97.99105938547980088 ) ) ;
#6181 = CARTESIAN_POINT ( 'NONE',  ( 26.11404676487256893, -110.9778746459748362, 22.43340081644731043 ) ) ;
#6182 = CARTESIAN_POINT ( 'NONE',  ( -20.20700224038492010, -0.9908225410476447781, 29.58392382092673500 ) ) ;
#6183 = EDGE_LOOP ( 'NONE', ( #8402, #27796, #21809, #2267 ) ) ;
#6184 = CARTESIAN_POINT ( 'NONE',  ( 9.884929003653608603, 27.17402761732343919, 148.0628878137281390 ) ) ;
#6185 = CARTESIAN_POINT ( 'NONE',  ( 26.11404676487259024, 22.43340081644921113, -110.9778746459744667 ) ) ;
#6186 = ORIENTED_EDGE ( 'NONE', *, *, #12602, .T. ) ;
#6187 = FACE_OUTER_BOUND ( 'NONE', #2650, .T. ) ;
#6188 = CARTESIAN_POINT ( 'NONE',  ( 1.833485406944043827, 96.69979900902318093, -108.1939177044916107 ) ) ;
#6189 = CARTESIAN_POINT ( 'NONE',  ( 25.64692232868537758, 103.0161468101953517, -46.22343382108633136 ) ) ;
#6190 = CARTESIAN_POINT ( 'NONE',  ( -15.02187109954783040, -21.95370994985601953, -40.82269973458228662 ) ) ;
#6191 = AXIS2_PLACEMENT_3D ( 'NONE', #23562, #17052, #25850 ) ;
#6192 = CARTESIAN_POINT ( 'NONE',  ( -25.21435515916025594, 1.749597353048488237E-16, -4.373993382621220594E-17 ) ) ;
#6193 = CARTESIAN_POINT ( 'NONE',  ( -1.323439229708141207, -46.01398008004442630, 2.317790194800218195 ) ) ;
#6194 = CARTESIAN_POINT ( 'NONE',  ( -7.078251931573400491, 44.92740138729166688, -26.33626633876239609 ) ) ;
#6195 = CARTESIAN_POINT ( 'NONE',  ( 32.73300124599741423, -84.80615050150312584, -81.52272205837286378 ) ) ;
#6196 = DIRECTION ( 'NONE',  ( -1.000000000000000000, -0.000000000000000000, -0.000000000000000000 ) ) ;
#6197 = CARTESIAN_POINT ( 'NONE',  ( -1.539763995773687499, -29.16712963492436828, 35.94321074656927095 ) ) ;
#6198 = EDGE_CURVE ( 'NONE', #2342, #10460, #25124, .T. ) ;
#6199 = CARTESIAN_POINT ( 'NONE',  ( 109.1587776205901861, -0.007297420966932451417, -0.0006832286435016619213 ) ) ;
#6200 = CARTESIAN_POINT ( 'NONE',  ( 25.64681081121879203, -46.30456157731261868, -102.9795863647033229 ) ) ;
#6201 = CARTESIAN_POINT ( 'NONE',  ( -20.20612092514785019, -10.22177639105880864, -27.77903665678161360 ) ) ;
#6202 = EDGE_LOOP ( 'NONE', ( #22759, #21348, #23197, #16355 ) ) ;
#6203 = EDGE_CURVE ( 'NONE', #8387, #3421, #15514, .T. ) ;
#6204 = EDGE_LOOP ( 'NONE', ( #28020, #4417, #4966, #23605 ) ) ;
#6205 = ORIENTED_EDGE ( 'NONE', *, *, #8240, .F. ) ;
#6206 = CARTESIAN_POINT ( 'NONE',  ( 109.1721716018069515, -0.01467989464938416512, -0.008708654716135893342 ) ) ;
#6207 = CARTESIAN_POINT ( 'NONE',  ( 55.79472521941426777, 30.25520714117996590, -66.16469064668267208 ) ) ;
#6208 = CARTESIAN_POINT ( 'NONE',  ( 109.1592201516379674, -0.006174480289200349852, -0.004867031887010190086 ) ) ;
#6209 = DIRECTION ( 'NONE',  ( 0.000000000000000000, -1.000000000000000000, 0.000000000000000000 ) ) ;
#6210 = CARTESIAN_POINT ( 'NONE',  ( -1.113427685307007087, 42.96952363574832390, -16.03057832159165486 ) ) ;
#6211 = LINE ( 'NONE', #10659, #21311 ) ;
#6212 = CARTESIAN_POINT ( 'NONE',  ( -9.156249394959713683, -53.74753343182709386, -9.022661520477562647 ) ) ;
#6213 = ORIENTED_EDGE ( 'NONE', *, *, #1533, .T. ) ;
#6214 = DIRECTION ( 'NONE',  ( -1.000000000000000000, -0.000000000000000000, -0.000000000000000000 ) ) ;
#6215 = CARTESIAN_POINT ( 'NONE',  ( -1.583189561560255143, -46.33203782964464068, -2.490696082059702832 ) ) ;
#6216 = CARTESIAN_POINT ( 'NONE',  ( 1.833603222531972499, 117.6571262511690037, -84.93295186324742474 ) ) ;
#6217 = CARTESIAN_POINT ( 'NONE',  ( -20.20612092514784663, -28.48192215759672408, -8.058517256680987728 ) ) ;
#6218 = ORIENTED_EDGE ( 'NONE', *, *, #253, .F. ) ;
#6219 = CARTESIAN_POINT ( 'NONE',  ( 2.263178113027048077, 43.59477710889728286, 138.7064940342179966 ) ) ;
#6220 = CARTESIAN_POINT ( 'NONE',  ( -1.050229599974473293, 0.2556477501659514262, -45.79907399707867199 ) ) ;
#6221 = VERTEX_POINT ( 'NONE', #4007 ) ;
#6222 = ORIENTED_EDGE ( 'NONE', *, *, #16319, .F. ) ;
#6223 = ORIENTED_EDGE ( 'NONE', *, *, #10963, .T. ) ;
#6224 = CARTESIAN_POINT ( 'NONE',  ( 1.834118845439484335, -117.2918069668806424, 85.43746956709813389 ) ) ;
#6225 = CARTESIAN_POINT ( 'NONE',  ( -1.239374126674604337, 25.08410696974242882, -38.61989855450947573 ) ) ;
#6226 = EDGE_CURVE ( 'NONE', #5185, #26195, #3503, .T. ) ;
#6227 = EDGE_CURVE ( 'NONE', #6545, #976, #15146, .T. ) ;
#6228 = CARTESIAN_POINT ( 'NONE',  ( 9.884929003653626367, -91.84919534721861112, -119.2676479132383065 ) ) ;
#6229 = FACE_OUTER_BOUND ( 'NONE', #6777, .T. ) ;
#6230 = ORIENTED_EDGE ( 'NONE', *, *, #5353, .F. ) ;
#6231 = EDGE_CURVE ( 'NONE', #20099, #5993, #2397, .T. ) ;
#6232 = CARTESIAN_POINT ( 'NONE',  ( 1.833691583653584978, 59.34641645332813198, -132.4191286035299413 ) ) ;
#6233 = B_SPLINE_CURVE_WITH_KNOTS ( 'NONE', 3,
 ( #3496, #12280, #21046, #10139, #22010, #3926, #9995 ),
 .UNSPECIFIED., .F., .F.,
 ( 4, 3, 4 ),
 ( 0.000000000000000000, 0.02398743853561342496, 0.04000277880656223639 ),
 .UNSPECIFIED. ) ;
#6234 = CARTESIAN_POINT ( 'NONE',  ( -10.86508079875781263, -22.20099862734791074, 46.07061504567109012 ) ) ;
#6235 = EDGE_CURVE ( 'NONE', #26116, #19494, #12419, .T. ) ;
#6236 = DIRECTION ( 'NONE',  ( 0.000000000000000000, 0.000000000000000000, 1.000000000000000000 ) ) ;
#6237 = CARTESIAN_POINT ( 'NONE',  ( -7.711401346138435642, 45.70592430511758408, 25.75361633141439199 ) ) ;
#6238 = FACE_OUTER_BOUND ( 'NONE', #27687, .T. ) ;
#6239 = CARTESIAN_POINT ( 'NONE',  ( 1.832998868059890096, 84.86110816369605914, 117.7096351258390712 ) ) ;
#6240 = CARTESIAN_POINT ( 'NONE',  ( 32.73300124599741423, 117.3295799645430435, -8.473903470904879498 ) ) ;
#6241 = CARTESIAN_POINT ( 'NONE',  ( 55.79472521941426777, -43.35047097963490614, 58.42842213658313000 ) ) ;
#6242 = VERTEX_POINT ( 'NONE', #19547 ) ;
#6243 = ORIENTED_EDGE ( 'NONE', *, *, #3127, .F. ) ;
#6244 = CARTESIAN_POINT ( 'NONE',  ( -1.619063947482197729, 44.80407745103800465, 11.94059994246113021 ) ) ;
#6245 = ORIENTED_EDGE ( 'NONE', *, *, #1076, .T. ) ;
#6246 = ORIENTED_EDGE ( 'NONE', *, *, #6081, .T. ) ;
#6247 = VERTEX_POINT ( 'NONE', #4715 ) ;
#6248 = CARTESIAN_POINT ( 'NONE',  ( -1.045287976400362417, -15.59869763335038506, 43.05558670614261985 ) ) ;
#6249 = EDGE_CURVE ( 'NONE', #13718, #7372, #20317, .T. ) ;
#6250 = CARTESIAN_POINT ( 'NONE',  ( -1.019300379054419725, -42.90269154183418010, 16.06793277092037187 ) ) ;
#6251 = CARTESIAN_POINT ( 'NONE',  ( 2.430230287190592531, 28.83279105684623644, -142.6294793592095118 ) ) ;
#6252 = EDGE_CURVE ( 'NONE', #1405, #22236, #26578, .T. ) ;
#6253 = CARTESIAN_POINT ( 'NONE',  ( -20.20997486282892552, 1.395963739018065216E-16, 29.60348406988233450 ) ) ;
#6254 = B_SPLINE_CURVE_WITH_KNOTS ( 'NONE', 3,
 ( #18666, #3689, #12052, #25451, #10337, #5726 ),
 .UNSPECIFIED., .F., .F.,
 ( 4, 2, 4 ),
 ( 1.110764993427085326E-17, 0.0006311636237756891024, 0.001262327247551367146 ),
 .UNSPECIFIED. ) ;
#6255 = CARTESIAN_POINT ( 'NONE',  ( -10.86508079875781618, 50.67624451685635734, 6.877801422380954044 ) ) ;
#6256 = LINE ( 'NONE', #15425, #18559 ) ;
#6257 = CARTESIAN_POINT ( 'NONE',  ( -1.019300379054419947, 44.15350047934399669, -12.21833869579480236 ) ) ;
#6258 = CARTESIAN_POINT ( 'NONE',  ( -1.046936909428682450, 27.93981068760674802, 36.28616897897423144 ) ) ;
#6259 = LINE ( 'NONE', #19338, #23520 ) ;
#6260 = ORIENTED_EDGE ( 'NONE', *, *, #21640, .T. ) ;
#6261 = ORIENTED_EDGE ( 'NONE', *, *, #8531, .T. ) ;
#6263 = CARTESIAN_POINT ( 'NONE',  ( 109.1592201516379674, 0.007856029051018016685, 0.0003082430541935266563 ) ) ;
#6262 = CARTESIAN_POINT ( 'NONE',  ( 25.64692872815574631, 112.9107203549055924, 0.3216598674787775058 ) ) ;
#6264 = B_SPLINE_CURVE_WITH_KNOTS ( 'NONE', 3,
 ( #21063, #15932, #20927, #1351, #24743, #10011 ),
 .UNSPECIFIED., .F., .F.,
 ( 4, 2, 4 ),
 ( 4.653458371169123007E-16, 0.003576372551511270217, 0.007152745103022075529 ),
 .UNSPECIFIED. ) ;
#6265 = CARTESIAN_POINT ( 'NONE',  ( -15.02187109954788191, -45.60876405941872491, 8.264310930412850809 ) ) ;
#6266 = CARTESIAN_POINT ( 'NONE',  ( 25.98107933586716456, 1.091357942392178204, -113.1286487641202569 ) ) ;
#6267 = CARTESIAN_POINT ( 'NONE',  ( 1.893872463202039391, -71.74819926215087662, -126.1771883101044693 ) ) ;
#6268 = EDGE_LOOP ( 'NONE', ( #23361, #12832, #24833, #19188 ) ) ;
#6269 = CARTESIAN_POINT ( 'NONE',  ( -2.911734481061396540, 12.03743348210780439, -46.11606034418766598 ) ) ;
#6270 = B_SPLINE_CURVE_WITH_KNOTS ( 'NONE', 3,
 ( #7444, #2676, #22560, #20226, #25144, #27135, #20383, #524, #9318, #16062 ),
 .UNSPECIFIED., .F., .F.,
 ( 4, 2, 2, 2, 4 ),
 ( 4.210279659405072890E-18, 0.0003346267210630970664, 0.0006692534421261899045, 0.001003880163189282580, 0.001338506884252375472 ),
 .UNSPECIFIED. ) ;
#6271 = CARTESIAN_POINT ( 'NONE',  ( -5.986830583229487246, -26.01297580803291964, 43.56094206392985058 ) ) ;
#6272 = CARTESIAN_POINT ( 'NONE',  ( 16.05277956358198566, -99.31161228512409878, -103.3141821208293578 ) ) ;
#6273 = VERTEX_POINT ( 'NONE', #26034 ) ;
#6274 = EDGE_LOOP ( 'NONE', ( #4199, #20343, #22437, #18264 ) ) ;
#6275 = CARTESIAN_POINT ( 'NONE',  ( -1.259920593601966177, -16.33409644610522449, 43.01175804832023886 ) ) ;
#6276 = ORIENTED_EDGE ( 'NONE', *, *, #6000, .F. ) ;
#6277 = CARTESIAN_POINT ( 'NONE',  ( 1.832998868059890096, 117.0819875546695670, 85.72499093308135798 ) ) ;
#6278 = VERTEX_POINT ( 'NONE', #17797 ) ;
#6279 = CARTESIAN_POINT ( 'NONE',  ( -4.178947244162626973, 31.41809272265978947, 37.51424432987617053 ) ) ;
#6280 = CARTESIAN_POINT ( 'NONE',  ( -1.583189561560255143, -43.29471907393753582, -16.68617981233685299 ) ) ;
#6281 = ORIENTED_EDGE ( 'NONE', *, *, #25296, .F. ) ;
#6282 = CARTESIAN_POINT ( 'NONE',  ( 26.11404676487257603, -76.59696442953247697, 83.38016054979757996 ) ) ;
#6283 = EDGE_CURVE ( 'NONE', #26195, #14327, #8648, .T. ) ;
#6284 = DIRECTION ( 'NONE',  ( 1.000000000000000000, -6.938893903907226837E-18, 1.734723475976806709E-18 ) ) ;
#6285 = ADVANCED_FACE ( 'NONE', ( #6603 ), #10689, .F. ) ;
#6286 = CARTESIAN_POINT ( 'NONE',  ( -1.031422197589716205, -28.14735071801717936, 36.13727897780158571 ) ) ;
#6287 = CARTESIAN_POINT ( 'NONE',  ( -55.24271866751342941, -0.008433070970613520956, 0.004365563123935277227 ) ) ;
#6288 = CARTESIAN_POINT ( 'NONE',  ( -1.050229599974477734, 14.39582765040461254, -43.47850826583058392 ) ) ;
#6289 = CARTESIAN_POINT ( 'NONE',  ( 1.831572820252008738, -132.1614873090345270, -59.92262167723569632 ) ) ;
#6290 = EDGE_CURVE ( 'NONE', #8378, #10268, #13196, .T. ) ;
#6291 = DIRECTION ( 'NONE',  ( 0.5914120900931444380, 0.7903769105750353408, -0.1598001217819338404 ) ) ;
#6292 = DIRECTION ( 'NONE',  ( -1.000000000000000000, -0.000000000000000000, -0.000000000000000000 ) ) ;
#6293 = CARTESIAN_POINT ( 'NONE',  ( 26.04756280548354752, -112.4366864265128640, 12.93458011762439419 ) ) ;
#6294 = ORIENTED_EDGE ( 'NONE', *, *, #10006, .F. ) ;
#6295 = ORIENTED_EDGE ( 'NONE', *, *, #5361, .F. ) ;
#6296 = CARTESIAN_POINT ( 'NONE',  ( 25.64692872815576052, 56.73392579406848313, -97.62272225320887742 ) ) ;
#6297 = CARTESIAN_POINT ( 'NONE',  ( 2.263178607246673746, 118.4461883615815339, 84.32376080825592624 ) ) ;
#6298 = CARTESIAN_POINT ( 'NONE',  ( 55.79472521941426777, -42.17269936297599031, -59.28412330436345457 ) ) ;
#6299 = CARTESIAN_POINT ( 'NONE',  ( -8.786685647604896232, 25.35688121747570278, 47.14957014837326454 ) ) ;
#6300 = CARTESIAN_POINT ( 'NONE',  ( 1.893872463202063150, 84.54426271294425987, 117.9862474593099648 ) ) ;
#6301 = CARTESIAN_POINT ( 'NONE',  ( -25.21435515916043002, 23.92354251275938992, -25.00736669481030106 ) ) ;
#6302 = ORIENTED_EDGE ( 'NONE', *, *, #5642, .F. ) ;
#6303 = CARTESIAN_POINT ( 'NONE',  ( 2.433796855181205476, -107.1581411821778858, -98.43889364293970345 ) ) ;
#6304 = CARTESIAN_POINT ( 'NONE',  ( 109.1587776205901861, 0.0008489206734500592518, 0.007280006032835109955 ) ) ;
#6305 = DIRECTION ( 'NONE',  ( 0.000000000000000000, -5.223019709708233256E-21, 1.000000000000000000 ) ) ;
#6306 = CARTESIAN_POINT ( 'NONE',  ( 10.93730112725932635, 0.000000000000000000, 0.000000000000000000 ) ) ;
#6307 = CARTESIAN_POINT ( 'NONE',  ( 1.833721034905648972, 117.6051524288283758, 85.00517831633722210 ) ) ;
#6308 = ORIENTED_EDGE ( 'NONE', *, *, #6675, .F. ) ;
#6309 = CARTESIAN_POINT ( 'NONE',  ( -1.583189561560255143, -11.94859433442934282, -44.83405390829668136 ) ) ;
#6311 = CARTESIAN_POINT ( 'NONE',  ( 1.831572820252009626, -14.18623102066865549, 144.4165162501762154 ) ) ;
#6310 = B_SPLINE_CURVE_WITH_KNOTS ( 'NONE', 3,
 ( #4929, #9406, #22502, #13133, #15561, #24235 ),
 .UNSPECIFIED., .F., .F.,
 ( 4, 2, 4 ),
 ( 0.000000000000000000, 0.0004335151646191525506, 0.0008670303292383051011 ),
 .UNSPECIFIED. ) ;
#6312 =( BOUNDED_SURFACE ( )  B_SPLINE_SURFACE ( 3, 1, ( 
 ( #5041, #22628 ),
 ( #1020, #11820 ),
 ( #22482, #9385 ),
 ( #11523, #11674 ) ),
 .UNSPECIFIED., .F., .F., .F. ) 
 B_SPLINE_SURFACE_WITH_KNOTS ( ( 4, 4 ),
 ( 2, 2 ),
 ( 0.000000000000000000, 1.000000000000000000 ),
 ( 0.000000000000000000, 1.000000000000000000 ),
 .UNSPECIFIED. ) 
 GEOMETRIC_REPRESENTATION_ITEM ( )  RATIONAL_B_SPLINE_SURFACE ( (
 ( 1.000000000000000000, 1.000000000000000000),
 ( 0.6386103224230316178, 0.9954351624131538845),
 ( 0.6386103224230316178, 0.9954351624131538845),
 ( 1.000000000000000000, 1.000000000000000000) ) ) 
 REPRESENTATION_ITEM ( '' )  SURFACE ( )  );
#6313 = ORIENTED_EDGE ( 'NONE', *, *, #4751, .T. ) ;
#6314 = ADVANCED_FACE ( 'NONE', ( #6882 ), #9584, .F. ) ;
#6315 = CARTESIAN_POINT ( 'NONE',  ( 25.64681081121879203, 97.57530875170684226, -56.81519825470653018 ) ) ;
#6316 = CARTESIAN_POINT ( 'NONE',  ( 1.833485406944043827, 0.5339064996905048543, -145.1085452359073145 ) ) ;
#6317 = CARTESIAN_POINT ( 'NONE',  ( 2.108985857320901935, 108.8271972979199944, 96.26411661813067155 ) ) ;
#6318 = B_SPLINE_CURVE_WITH_KNOTS ( 'NONE', 3,
 ( #11957, #20731, #5631, #9657, #7663, #14397 ),
 .UNSPECIFIED., .F., .F.,
 ( 4, 2, 4 ),
 ( 8.673617379884035472E-18, 0.0006311636237756913792, 0.001262327247551374085 ),
 .UNSPECIFIED. ) ;
#6319 = EDGE_CURVE ( 'NONE', #4812, #24848, #9173, .T. ) ;
#6320 = DIRECTION ( 'NONE',  ( 0.7563875759206388771, -0.5078650950445684487, -0.4122509917856733708 ) ) ;
#6321 = CARTESIAN_POINT ( 'NONE',  ( 1.834118845439484335, 29.99597360113265054, -141.9759513273461664 ) ) ;
#6322 = DIRECTION ( 'NONE',  ( -0.7563875759206388771, 0.6104009704506910827, -0.2351350468682930628 ) ) ;
#6323 = CARTESIAN_POINT ( 'NONE',  ( -20.90916690077961704, -28.59207721780126477, 27.35210456531406109 ) ) ;
#6324 = CARTESIAN_POINT ( 'NONE',  ( 109.1592201516379674, -0.004368284148529054563, -0.006536841731953389224 ) ) ;
#6325 = CARTESIAN_POINT ( 'NONE',  ( -8.786685647604855376, -7.199674155859337787, -53.04920435127184675 ) ) ;
#6326 = CARTESIAN_POINT ( 'NONE',  ( -6.588769196390762417, 4.956336548259653974, -51.10255870850470217 ) ) ;
#6327 = CARTESIAN_POINT ( 'NONE',  ( -8.786685647604885574, 6.096987947571466530E-17, -1.524246986892866633E-17 ) ) ;
#6328 = DIRECTION ( 'NONE',  ( 1.000000000000000000, -6.938893903907226837E-18, 1.734723475976806709E-18 ) ) ;
#6329 = CARTESIAN_POINT ( 'NONE',  ( -20.21097721712959938, -23.76068428613694294, -17.67178718142850258 ) ) ;
#6330 = CARTESIAN_POINT ( 'NONE',  ( -20.20700224038492721, 29.58392382092673500, 0.9908225410479544193 ) ) ;
#6331 = DIRECTION ( 'NONE',  ( -0.000000000000000000, 1.000000000000000000, -0.000000000000000000 ) ) ;
#6332 = ORIENTED_EDGE ( 'NONE', *, *, #24868, .T. ) ;
#6333 = VERTEX_POINT ( 'NONE', #26718 ) ;
#6334 = CARTESIAN_POINT ( 'NONE',  ( -1.049819825607597235, -43.39756533277870432, 14.63675055554426407 ) ) ;
#6335 = LINE ( 'NONE', #8763, #20826 ) ;
#6336 = CARTESIAN_POINT ( 'NONE',  ( 1.834118845439484335, -85.14950727125936680, 117.5010238212695697 ) ) ;
#6337 = CARTESIAN_POINT ( 'NONE',  ( 30.58324630866348670, 119.8048187378266505, -16.55818995381025616 ) ) ;
#6338 = CARTESIAN_POINT ( 'NONE',  ( 19.66333377628713563, -137.3914191246404926, 9.924285918886006641 ) ) ;
#6339 = VERTEX_POINT ( 'NONE', #17934 ) ;
#6340 = CARTESIAN_POINT ( 'NONE',  ( 1.833206310202317946, 30.89799345102960970, 141.7818020564279493 ) ) ;
#6341 = DIRECTION ( 'NONE',  ( 1.000000000000000000, -6.938893903907226837E-18, 1.734723475976806709E-18 ) ) ;
#6342 = CARTESIAN_POINT ( 'NONE',  ( 2.263178113027036531, 46.26071604342251931, -137.8402779654365702 ) ) ;
#6343 = VERTEX_POINT ( 'NONE', #11471 ) ;
#6344 = CARTESIAN_POINT ( 'NONE',  ( 25.64699802086720481, -45.70780507840510865, 103.2460182674616362 ) ) ;
#6345 = CARTESIAN_POINT ( 'NONE',  ( -1.050230347699842692, 0.0002315326058698765721, -45.79907861674080749 ) ) ;
#6346 = ORIENTED_EDGE ( 'NONE', *, *, #14189, .F. ) ;
#6347 = ORIENTED_EDGE ( 'NONE', *, *, #24073, .F. ) ;
#6348 = EDGE_CURVE ( 'NONE', #15181, #25910, #21699, .T. ) ;
#6349 = EDGE_LOOP ( 'NONE', ( #17581, #26671, #547, #17859 ) ) ;
#6350 =( BOUNDED_SURFACE ( )  B_SPLINE_SURFACE ( 3, 1, ( 
 ( #5545, #16193 ),
 ( #14312, #797 ),
 ( #27416, #16335 ),
 ( #14029, #27121 ) ),
 .UNSPECIFIED., .F., .F., .F. ) 
 B_SPLINE_SURFACE_WITH_KNOTS ( ( 4, 4 ),
 ( 2, 2 ),
 ( 0.000000000000000000, 1.000000000000000000 ),
 ( 0.000000000000000000, 1.000000000000000000 ),
 .UNSPECIFIED. ) 
 GEOMETRIC_REPRESENTATION_ITEM ( )  RATIONAL_B_SPLINE_SURFACE ( (
 ( 1.000000000000000000, 1.000000000000000000),
 ( 0.9934239774497837239, 0.8357310067453919133),
 ( 0.9934239774497837239, 0.8357310067453919133),
 ( 1.000000000000000000, 1.000000000000000000) ) ) 
 REPRESENTATION_ITEM ( '' )  SURFACE ( )  );
#6351 = EDGE_CURVE ( 'NONE', #17891, #21070, #3376, .T. ) ;
#6352 = EDGE_CURVE ( 'NONE', #9016, #13373, #12293, .T. ) ;
#6353 = DIRECTION ( 'NONE',  ( -1.000000000000000000, -0.000000000000000000, -0.000000000000000000 ) ) ;
#6354 = CARTESIAN_POINT ( 'NONE',  ( 6.224689322667630975, 139.9988794244332269, 48.18553814190077844 ) ) ;
#6355 = CARTESIAN_POINT ( 'NONE',  ( -12.94347594948497537, -42.93165645342824632, 23.08810053288727104 ) ) ;
#6356 = CARTESIAN_POINT ( 'NONE',  ( 16.75465622695633883, 120.7871673903176912, 75.09093759626908593 ) ) ;
#6357 = ORIENTED_EDGE ( 'NONE', *, *, #17672, .F. ) ;
#6358 = B_SPLINE_CURVE_WITH_KNOTS ( 'NONE', 3,
 ( #3983, #24142, #10763, #2092, #14918, #10895, #28291, #28155 ),
 .UNSPECIFIED., .F., .F.,
 ( 4, 2, 2, 4 ),
 ( 0.000000000000000000, 0.002761524886576654115, 0.005523049773153308230, 0.01104609954630660952 ),
 .UNSPECIFIED. ) ;
#6359 = CARTESIAN_POINT ( 'NONE',  ( 2.430230287190592531, 1.451610819317743051, 145.5073573687466819 ) ) ;
#6360 = CARTESIAN_POINT ( 'NONE',  ( -21.81686047589426991, -16.72402253294291796, 34.70276904128906637 ) ) ;
#6361 = EDGE_CURVE ( 'NONE', #1161, #24022, #12770, .T. ) ;
#6362 = DIRECTION ( 'NONE',  ( 0.5946245182733607137, -0.3994439555666229325, -0.6977579871484549390 ) ) ;
#6363 = CARTESIAN_POINT ( 'NONE',  ( -1.045287976400365970, 45.76855895860943235, -1.530335034934267258 ) ) ;
#6364 = CARTESIAN_POINT ( 'NONE',  ( -22.34422965417122953, 6.759368364654329220, -37.30738373203623581 ) ) ;
#6365 = CARTESIAN_POINT ( 'NONE',  ( -55.24300891470648622, -0.009812809446890113918, -0.0003472257464246985225 ) ) ;
#6366 = B_SPLINE_CURVE_WITH_KNOTS ( 'NONE', 3,
 ( #16079, #24884, #5145, #2996, #11779, #9611, #19372, #23164 ),
 .UNSPECIFIED., .F., .F.,
 ( 4, 2, 2, 4 ),
 ( 1.551583845779545699E-17, 0.0002429592666046777902, 0.0004859185332093400762, 0.0009718370664186931629 ),
 .UNSPECIFIED. ) ;
#6367 = CARTESIAN_POINT ( 'NONE',  ( 6.224689322667647851, 43.30635742325564763, -141.5842213414009336 ) ) ;
#6368 = CARTESIAN_POINT ( 'NONE',  ( 32.73300124599738581, -92.86301839380070078, 72.21147546950520280 ) ) ;
#6369 = CIRCLE ( 'NONE', #27969, 151.1787379149930359 ) ;
#6370 = ORIENTED_EDGE ( 'NONE', *, *, #6778, .T. ) ;
#6371 = CIRCLE ( 'NONE', #19252, 143.8872038478949946 ) ;
#6372 = EDGE_CURVE ( 'NONE', #7039, #22163, #24602, .T. ) ;
#6373 = ORIENTED_EDGE ( 'NONE', *, *, #417, .F. ) ;
#6374 = CARTESIAN_POINT ( 'NONE',  ( -1.619063947482194177, -46.30105812165547974, 2.489035965910640247 ) ) ;
#6375 = CARTESIAN_POINT ( 'NONE',  ( -1.048996300304487095, 45.79145529752471333, -0.7649764263853394697 ) ) ;
#6376 = ORIENTED_EDGE ( 'NONE', *, *, #18126, .F. ) ;
#6377 = EDGE_LOOP ( 'NONE', ( #11424, #18656 ) ) ;
#6378 = VERTEX_POINT ( 'NONE', #20785 ) ;
#6379 = CARTESIAN_POINT ( 'NONE',  ( 109.1589550718174877, -0.001354998915261381278, -0.007453082872776636315 ) ) ;
#6380 = EDGE_CURVE ( 'NONE', #6789, #5543, #6264, .T. ) ;
#6381 = ADVANCED_FACE ( 'NONE', ( #13628 ), #605, .T. ) ;
#6382 = FACE_OUTER_BOUND ( 'NONE', #14801, .T. ) ;
#6383 = CARTESIAN_POINT ( 'NONE',  ( -21.41427618760458529, 25.94789270595506991, -16.60878262545428541 ) ) ;
#6384 = CARTESIAN_POINT ( 'NONE',  ( 1.832998868059858122, 125.4013017422230831, 73.01698022778400343 ) ) ;
#6385 = CARTESIAN_POINT ( 'NONE',  ( 109.1721716018069515, -0.01616973485710002101, -0.005466227998627423527 ) ) ;
#6386 = CARTESIAN_POINT ( 'NONE',  ( -20.57838717382308147, 7.715628353033680220, -28.96176188950220975 ) ) ;
#6387 = CARTESIAN_POINT ( 'NONE',  ( -21.81686047589415622, 38.17230180719270294, 5.181745222995608025 ) ) ;
#6388 = CARTESIAN_POINT ( 'NONE',  ( 25.64692232868535982, -110.3753891203787987, 23.79507962493589801 ) ) ;
#6389 = B_SPLINE_CURVE_WITH_KNOTS ( 'NONE', 3,
 ( #7149, #9299, #4830, #4687, #11587, #26972, #20363, #22693, #24845, #651, #13595, #13458, #24271 ),
 .UNSPECIFIED., .F., .F.,
 ( 4, 3, 3, 3, 4 ),
 ( 9.813077866773594792E-18, 0.0007657099931970658743, 0.001531419946797928045, 0.002296279302920156435, 0.003061450627205745956 ),
 .UNSPECIFIED. ) ;
#6390 = CARTESIAN_POINT ( 'NONE',  ( 25.81918753295378011, 102.8711004511199860, -46.82320532096414922 ) ) ;
#6391 = CARTESIAN_POINT ( 'NONE',  ( 24.01988960052077360, -69.18817751538357186, 111.2910478357996169 ) ) ;
#6392 = ORIENTED_EDGE ( 'NONE', *, *, #11541, .F. ) ;
#6393 = VERTEX_POINT ( 'NONE', #14450 ) ;
#6394 = CARTESIAN_POINT ( 'NONE',  ( -1.031422197589716205, -12.69107518035472637, 44.01264471863859740 ) ) ;
#6395 = CARTESIAN_POINT ( 'NONE',  ( -18.41936578851712980, -41.75701384111727776, 7.566034416291218534 ) ) ;
#6396 = CARTESIAN_POINT ( 'NONE',  ( 5.340103556456445411, -17.70136535450003734, 146.3832391989195401 ) ) ;
#6397 = CARTESIAN_POINT ( 'NONE',  ( -4.162674018437148682, 41.48630000627055381, -25.90909455705125453 ) ) ;
#6398 = CARTESIAN_POINT ( 'NONE',  ( -1.619063947482201282, 35.99532424477380488, -29.22875152547769062 ) ) ;
#6399 = ORIENTED_EDGE ( 'NONE', *, *, #8029, .T. ) ;
#6400 = CARTESIAN_POINT ( 'NONE',  ( -4.178947244162631414, 11.88256963646738740, -47.46809051147726422 ) ) ;
#6401 = EDGE_CURVE ( 'NONE', #6438, #12091, #22752, .T. ) ;
#6402 = CARTESIAN_POINT ( 'NONE',  ( 2.433796855181219243, 118.5671979538068257, -84.34988187690807138 ) ) ;
#6403 = CARTESIAN_POINT ( 'NONE',  ( -20.24419206586951603, 23.20105925399726132, -18.44224248888881590 ) ) ;
#6404 = ORIENTED_EDGE ( 'NONE', *, *, #27428, .T. ) ;
#6405 = ORIENTED_EDGE ( 'NONE', *, *, #22642, .T. ) ;
#6406 = EDGE_CURVE ( 'NONE', #10758, #8004, #10040, .T. ) ;
#6407 = CARTESIAN_POINT ( 'NONE',  ( -20.20700224038492721, 27.82980252387819675, -10.08426345511598932 ) ) ;
#6408 = CARTESIAN_POINT ( 'NONE',  ( 25.73574536432413495, 107.1893601970595142, 35.67555431182866954 ) ) ;
#6409 = ORIENTED_EDGE ( 'NONE', *, *, #27548, .F. ) ;
#6410 = EDGE_CURVE ( 'NONE', #5380, #11657, #8296, .T. ) ;
#6411 = B_SPLINE_CURVE_WITH_KNOTS ( 'NONE', 3,
 ( #2883, #859, #9644, #13953, #5318, #4754 ),
 .UNSPECIFIED., .F., .F.,
 ( 4, 2, 4 ),
 ( 4.906538933386797396E-18, 0.0004335184443140297200, 0.0008670368886280544526 ),
 .UNSPECIFIED. ) ;
#6412 = B_SPLINE_CURVE_WITH_KNOTS ( 'NONE', 3,
 ( #21868, #28192, #1997, #17257, #24045, #19838, #18236, #550 ),
 .UNSPECIFIED., .F., .F.,
 ( 4, 2, 2, 4 ),
 ( 2.196627850418165012E-16, 0.002761568181852864633, 0.005523136363705508957, 0.01104627272741078546 ),
 .UNSPECIFIED. ) ;
#6413 = DIRECTION ( 'NONE',  ( 0.000000000000000000, 5.223019709708233256E-21, -1.000000000000000000 ) ) ;
#6414 = ADVANCED_FACE ( 'NONE', ( #14592 ), #13607, .F. ) ;
#6415 = VERTEX_POINT ( 'NONE', #28242 ) ;
#6416 = CARTESIAN_POINT ( 'NONE',  ( -1.463510566862832318, 2.430838777910187432, -46.14841196428340453 ) ) ;
#6417 = CARTESIAN_POINT ( 'NONE',  ( 25.64681081121879203, -35.28660243342623204, 107.2555980796239936 ) ) ;
#6418 = CARTESIAN_POINT ( 'NONE',  ( -1.155031165708884755, -38.31525684316158475, -25.28071330859873100 ) ) ;
#6419 = B_SPLINE_CURVE_WITH_KNOTS ( 'NONE', 3,
 ( #5641, #14831, #12669, #21454, #25518, #21168, #18592, #3758 ),
 .UNSPECIFIED., .F., .F.,
 ( 4, 2, 2, 4 ),
 ( 0.000000000000000000, 0.0002429588503611252793, 0.0004859177007222505586, 0.0009718354014444827941 ),
 .UNSPECIFIED. ) ;
#6420 = CARTESIAN_POINT ( 'NONE',  ( 109.1721716018069657, -0.01368917435591426694, 0.01019541462303507999 ) ) ;
#6421 = CARTESIAN_POINT ( 'NONE',  ( 2.430230287190572103, 145.5073573687466819, 1.451610819318258194 ) ) ;
#6422 = CARTESIAN_POINT ( 'NONE',  ( 10.93730112725996229, -10.89264110824889364, -150.7858122213663989 ) ) ;
#6423 = VERTEX_POINT ( 'NONE', #8542 ) ;
#6424 = CARTESIAN_POINT ( 'NONE',  ( 1.833691583653537904, 125.4903330494899194, 72.86287859464628980 ) ) ;
#6426 = CARTESIAN_POINT ( 'NONE',  ( 10.93730112725945247, 97.44200844886275092, 115.5857507957704087 ) ) ;
#6425 = CARTESIAN_POINT ( 'NONE',  ( 109.1589550718175161, 0.003980125429509219145, 0.006445391216541659571 ) ) ;
#6427 = VECTOR ( 'NONE', #11559, 1000.000000000000114 ) ;
#6428 = CARTESIAN_POINT ( 'NONE',  ( -1.583189561560255143, -11.94859433442934282, -44.83405390829668136 ) ) ;
#6429 = ORIENTED_EDGE ( 'NONE', *, *, #11904, .F. ) ;
#6430 = VERTEX_POINT ( 'NONE', #17442 ) ;
#6431 = CARTESIAN_POINT ( 'NONE',  ( 32.73300124599738581, -72.21147546950486174, -92.86301839380092815 ) ) ;
#6432 = CARTESIAN_POINT ( 'NONE',  ( -1.058197053496154671, 25.48582931365525184, 38.06270006878825995 ) ) ;
#6433 = CARTESIAN_POINT ( 'NONE',  ( -55.24271866751342941, -0.008433070970613524425, -0.004365563123939557658 ) ) ;
#6434 = B_SPLINE_CURVE_WITH_KNOTS ( 'NONE', 3,
 ( #28464, #4309, #13086, #21872, #2128, #25646 ),
 .UNSPECIFIED., .F., .F.,
 ( 4, 2, 4 ),
 ( 3.729292374017667178E-16, 0.003576372551511173073, 0.007152745103021973180 ),
 .UNSPECIFIED. ) ;
#6435 = CARTESIAN_POINT ( 'NONE',  ( -15.02187109954787303, 21.95370994985631086, 40.82269973458213030 ) ) ;
#6436 = CARTESIAN_POINT ( 'NONE',  ( 26.11404676487257603, -67.46175819463425682, 90.92995828888176391 ) ) ;
#6437 = CARTESIAN_POINT ( 'NONE',  ( 2.263178113027061400, -137.8402779654366839, -46.26071604342208587 ) ) ;
#6438 = VERTEX_POINT ( 'NONE', #27838 ) ;
#6439 = CARTESIAN_POINT ( 'NONE',  ( 10.93730112725932635, 0.000000000000000000, 0.000000000000000000 ) ) ;
#6440 = CARTESIAN_POINT ( 'NONE',  ( 109.1592201516379674, -0.001127733110588171120, -0.007780772729122754396 ) ) ;
#6441 = CARTESIAN_POINT ( 'NONE',  ( -21.41430102051744200, -30.75470819672111134, 1.815007301162295805 ) ) ;
#6442 = CARTESIAN_POINT ( 'NONE',  ( 2.263178113027051186, -46.26071604342163113, 137.8402779654368260 ) ) ;
#6443 = EDGE_CURVE ( 'NONE', #18869, #243, #23147, .T. ) ;
#6444 = ORIENTED_EDGE ( 'NONE', *, *, #21940, .T. ) ;
#6445 = CARTESIAN_POINT ( 'NONE',  ( -55.24271866751342941, 0.006757859501006707216, 0.006671293903669109175 ) ) ;
#6446 = EDGE_CURVE ( 'NONE', #10146, #26248, #3800, .T. ) ;
#6447 = CARTESIAN_POINT ( 'NONE',  ( 1.833838848569444568, 14.99110384899719151, -144.3334397096296584 ) ) ;
#6448 = CARTESIAN_POINT ( 'NONE',  ( -1.058473599757826067, -35.99997772736190882, 28.32531354681322711 ) ) ;
#6449 = CIRCLE ( 'NONE', #26202, 151.1787379149930359 ) ;
#6450 = B_SPLINE_CURVE_WITH_KNOTS ( 'NONE', 3,
 ( #22673, #11568, #13580, #2943, #22819, #11426, #7404, #20347 ),
 .UNSPECIFIED., .F., .F.,
 ( 4, 2, 2, 4 ),
 ( 7.757919228897728493E-18, 0.0002429592666046789286, 0.0004859185332093501051, 0.0009718370664186827546 ),
 .UNSPECIFIED. ) ;
#6451 = ORIENTED_EDGE ( 'NONE', *, *, #16120, .T. ) ;
#6452 = CARTESIAN_POINT ( 'NONE',  ( 10.93730112725936898, 142.1801301103782578, 51.37919228020297879 ) ) ;
#6453 = VERTEX_POINT ( 'NONE', #19331 ) ;
#6454 = CARTESIAN_POINT ( 'NONE',  ( -28.13707043255157103, 12.83104814250454062, -18.96624908365850359 ) ) ;
#6455 = CARTESIAN_POINT ( 'NONE',  ( 2.433796855181205476, -1.451562450950653949, 145.5024947199069629 ) ) ;
#6456 = CARTESIAN_POINT ( 'NONE',  ( -1.323439229708126774, -12.01475235539415642, 44.47813215539056131 ) ) ;
#6457 = CARTESIAN_POINT ( 'NONE',  ( -1.045287976400383290, 36.12803364096649972, 28.14015102489766917 ) ) ;
#6458 = CARTESIAN_POINT ( 'NONE',  ( -1.019300379054419725, 44.15350047934416011, 12.21833869579419130 ) ) ;
#6459 = FACE_BOUND ( 'NONE', #1210, .T. ) ;
#6460 = CARTESIAN_POINT ( 'NONE',  ( 1.833721034905639646, -138.1171912769427763, -44.50273803002078665 ) ) ;
#6461 = CARTESIAN_POINT ( 'NONE',  ( -21.41430102051752016, 16.60879216503635547, -25.94791611261620545 ) ) ;
#6462 = CARTESIAN_POINT ( 'NONE',  ( 26.11404676487257603, 108.0249973236472130, -33.91085499298264239 ) ) ;
#6463 = CARTESIAN_POINT ( 'NONE',  ( -23.77929240705207192, -17.17389748746940370, 31.93650644494359270 ) ) ;
#6464 = CARTESIAN_POINT ( 'NONE',  ( 16.05277956358235159, 99.31161228512438299, 103.3141821208282920 ) ) ;
#6465 = FACE_OUTER_BOUND ( 'NONE', #19604, .T. ) ;
#6466 = CARTESIAN_POINT ( 'NONE',  ( 109.1721716018069657, 0.01629455849720090610, 0.005082060336469467095 ) ) ;
#6467 = ORIENTED_EDGE ( 'NONE', *, *, #23171, .T. ) ;
#6468 = VECTOR ( 'NONE', #9900, 1000.000000000000114 ) ;
#6469 = ORIENTED_EDGE ( 'NONE', *, *, #5609, .T. ) ;
#6470 = CARTESIAN_POINT ( 'NONE',  ( 25.64692872815577118, 103.0182448446673789, 46.21877827526595439 ) ) ;
#6471 = CARTESIAN_POINT ( 'NONE',  ( -55.24390624410018802, -0.007245494385991085341, 0.007503127514277716827 ) ) ;
#6472 = CARTESIAN_POINT ( 'NONE',  ( 28.37599760073042532, -93.86375353586211645, 65.97809271467107806 ) ) ;
#6473 = CIRCLE ( 'NONE', #5077, 117.6351876552689504 ) ;
#6474 = CARTESIAN_POINT ( 'NONE',  ( 109.1721716018069515, -0.007126480965768089773, 0.01550977894511842634 ) ) ;
#6475 = CARTESIAN_POINT ( 'NONE',  ( -28.41354790283022069, -19.47297445639558333, -12.60397206714825558 ) ) ;
#6476 = CARTESIAN_POINT ( 'NONE',  ( 28.37603512858356680, -13.77584568114216523, -113.9023475466376567 ) ) ;
#6477 = CARTESIAN_POINT ( 'NONE',  ( 32.73300124599735739, -44.31599526638029118, 108.9684813982487412 ) ) ;
#6478 = VERTEX_POINT ( 'NONE', #17306 ) ;
#6479 = CARTESIAN_POINT ( 'NONE',  ( -1.056502255334265339, -43.40574022158784118, -14.64009593116085739 ) ) ;
#6480 = CARTESIAN_POINT ( 'NONE',  ( 109.1624594426973118, -0.01582142368019174780, 0.002129375066974411451 ) ) ;
#6481 = VECTOR ( 'NONE', #26572, 999.9999999999998863 ) ;
#6482 = DIRECTION ( 'NONE',  ( 1.000000000000000000, -6.938893903907226837E-18, 1.734723475976806709E-18 ) ) ;
#6483 = CARTESIAN_POINT ( 'NONE',  ( 8.186469829614441807, 77.65916164626527518, -127.5731248499969439 ) ) ;
#6484 = ADVANCED_FACE ( 'NONE', ( #8680 ), #12526, .F. ) ;
#6485 = CARTESIAN_POINT ( 'NONE',  ( -1.464342487929857661, -43.13914623307948659, 16.57334911911557285 ) ) ;
#6486 =( BOUNDED_SURFACE ( )  B_SPLINE_SURFACE ( 3, 1, ( 
 ( #20048, #22514 ),
 ( #24542, #2781 ),
 ( #4805, #7123 ),
 ( #9416, #15880 ) ),
 .UNSPECIFIED., .F., .F., .F. ) 
 B_SPLINE_SURFACE_WITH_KNOTS ( ( 4, 4 ),
 ( 2, 2 ),
 ( 0.000000000000000000, 1.000000000000000000 ),
 ( 0.000000000000000000, 1.000000000000000000 ),
 .UNSPECIFIED. ) 
 GEOMETRIC_REPRESENTATION_ITEM ( )  RATIONAL_B_SPLINE_SURFACE ( (
 ( 1.000000000000000000, 1.000000000000000000),
 ( 0.6386103224230316178, 0.9954351624131538845),
 ( 0.6386103224230316178, 0.9954351624131538845),
 ( 1.000000000000000000, 1.000000000000000000) ) ) 
 REPRESENTATION_ITEM ( '' )  SURFACE ( )  );
#6487 = ORIENTED_EDGE ( 'NONE', *, *, #24795, .T. ) ;
#6488 = AXIS2_PLACEMENT_3D ( 'NONE', #2769, #9407, #13559 ) ;
#6489 = CARTESIAN_POINT ( 'NONE',  ( 2.108985857320915702, -46.11505917359347961, -137.7807691131292813 ) ) ;
#6490 = EDGE_CURVE ( 'NONE', #18732, #25406, #25695, .T. ) ;
#6491 = FACE_OUTER_BOUND ( 'NONE', #12810, .T. ) ;
#6492 = EDGE_LOOP ( 'NONE', ( #13124, #11810, #472, #14123 ) ) ;
#6493 = EDGE_CURVE ( 'NONE', #12120, #14327, #1635, .T. ) ;
#6494 = EDGE_LOOP ( 'NONE', ( #5082, #15860, #3017, #1733 ) ) ;
#6495 = VERTEX_POINT ( 'NONE', #1766 ) ;
#6496 = VECTOR ( 'NONE', #22555, 1000.000000000000114 ) ;
#6497 = FACE_OUTER_BOUND ( 'NONE', #9285, .T. ) ;
#6498 = CARTESIAN_POINT ( 'NONE',  ( 1.832998868059858122, 97.49378069860945573, -107.4798986104849803 ) ) ;
#6499 = CARTESIAN_POINT ( 'NONE',  ( 5.340103579038066428, 144.6887562507423297, 28.39990973304521304 ) ) ;
#6500 = AXIS2_PLACEMENT_3D ( 'NONE', #18540, #3283, #18233 ) ;
#6501 = CARTESIAN_POINT ( 'NONE',  ( -1.619063947482197729, 29.22875152547757338, -35.99532424477389725 ) ) ;
#6502 = CARTESIAN_POINT ( 'NONE',  ( 2.433796855181205476, 98.43889364294005873, -107.1581411821775305 ) ) ;
#6503 = DIRECTION ( 'NONE',  ( 0.000000000000000000, 5.223019709707975211E-21, -1.000000000000000000 ) ) ;
#6504 = CARTESIAN_POINT ( 'NONE',  ( -55.24271866751342941, -0.001545935011630300039, 0.009369360294295641864 ) ) ;
#6505 = CARTESIAN_POINT ( 'NONE',  ( 13.36082413113061307, 6.345145185220180117, -152.7944199136426846 ) ) ;
#6506 = EDGE_CURVE ( 'NONE', #5301, #10441, #27869, .T. ) ;
#6507 = CARTESIAN_POINT ( 'NONE',  ( 5.340103556456319289, 126.5279493230358270, 75.71042922800570807 ) ) ;
#6508 = CARTESIAN_POINT ( 'NONE',  ( -1.058473599757826067, -35.99997772736190882, 28.32531354681322711 ) ) ;
#6509 = CARTESIAN_POINT ( 'NONE',  ( -55.25297051322618813, 0.002853887643044372355, 0.01466904165775517396 ) ) ;
#6510 = AXIS2_PLACEMENT_3D ( 'NONE', #1607, #23508, #10276 ) ;
#6511 = VECTOR ( 'NONE', #16826, 1000.000000000000114 ) ;
#6512 = EDGE_CURVE ( 'NONE', #27747, #18251, #12573, .T. ) ;
#6513 = FACE_OUTER_BOUND ( 'NONE', #23311, .T. ) ;
#6514 = CARTESIAN_POINT ( 'NONE',  ( -28.13707043255157103, 7.802116958609309094, 21.52861750560930432 ) ) ;
#6515 = CARTESIAN_POINT ( 'NONE',  ( -1.583189561560256253, -38.94740041318311796, -25.21827308671218404 ) ) ;
#6516 = ORIENTED_EDGE ( 'NONE', *, *, #4081, .F. ) ;
#6518 = CIRCLE ( 'NONE', #8355, 34.60786435723138510 ) ;
#6517 =( BOUNDED_SURFACE ( )  B_SPLINE_SURFACE ( 3, 1, ( 
 ( #8180, #12615 ),
 ( #27882, #8725 ),
 ( #21536, #1675 ),
 ( #25734, #17352 ) ),
 .UNSPECIFIED., .F., .F., .F. ) 
 B_SPLINE_SURFACE_WITH_KNOTS ( ( 4, 4 ),
 ( 2, 2 ),
 ( 0.000000000000000000, 1.000000000000000000 ),
 ( 0.000000000000000000, 1.000000000000000000 ),
 .UNSPECIFIED. ) 
 GEOMETRIC_REPRESENTATION_ITEM ( )  RATIONAL_B_SPLINE_SURFACE ( (
 ( 1.000000000000000000, 1.000000000000000000),
 ( 0.9960225298536222738, 0.9999952330161893110),
 ( 0.9960225298536222738, 0.9999952330161893110),
 ( 1.000000000000000000, 1.000000000000000000) ) ) 
 REPRESENTATION_ITEM ( '' )  SURFACE ( )  );
#6519 = ORIENTED_EDGE ( 'NONE', *, *, #12197, .F. ) ;
#6520 = CARTESIAN_POINT ( 'NONE',  ( -5.986830583229487246, -50.53158596890438758, 4.559539818181663762 ) ) ;
#6521 = DIRECTION ( 'NONE',  ( -1.000000000000000000, -0.000000000000000000, -0.000000000000000000 ) ) ;
#6522 = ORIENTED_EDGE ( 'NONE', *, *, #10132, .T. ) ;
#6523 = VERTEX_POINT ( 'NONE', #21360 ) ;
#6524 = EDGE_LOOP ( 'NONE', ( #20313, #22871, #1858, #5359 ) ) ;
#6525 = LINE ( 'NONE', #2176, #2823 ) ;
#6526 = DIRECTION ( 'NONE',  ( -1.000000000000000000, -0.000000000000000000, -0.000000000000000000 ) ) ;
#6527 = VECTOR ( 'NONE', #23541, 1000.000000000000000 ) ;
#6528 = CARTESIAN_POINT ( 'NONE',  ( 13.36082413113063083, 25.56125765253660376, -150.7747251079859723 ) ) ;
#6529 = CARTESIAN_POINT ( 'NONE',  ( 25.64692872815576408, 66.10702795113414254, 91.53575854059441497 ) ) ;
#6530 = CARTESIAN_POINT ( 'NONE',  ( -20.90916690077962770, 27.35210456531415346, 28.59207721780114753 ) ) ;
#6531 = CARTESIAN_POINT ( 'NONE',  ( 109.1624594426973260, 0.006066618937909673721, 0.01476644236456053048 ) ) ;
#6532 = EDGE_CURVE ( 'NONE', #23680, #6666, #10711, .T. ) ;
#6533 = CARTESIAN_POINT ( 'NONE',  ( -9.156249394959706578, 53.90509764945129945, 8.027840202794124025 ) ) ;
#6534 = CARTESIAN_POINT ( 'NONE',  ( 25.64681081121879203, 112.9102952884414464, -0.4157506337731811663 ) ) ;
#6535 = DIRECTION ( 'NONE',  ( 1.000000000000000000, -6.938893903907226837E-18, 1.734723475976806709E-18 ) ) ;
#6536 = EDGE_CURVE ( 'NONE', #4951, #19079, #15280, .T. ) ;
#6537 = ORIENTED_EDGE ( 'NONE', *, *, #7073, .F. ) ;
#6538 = ORIENTED_EDGE ( 'NONE', *, *, #14907, .T. ) ;
#6540 = CARTESIAN_POINT ( 'NONE',  ( -24.53239521893651087, 6.738460611583212412, 33.25736993155762633 ) ) ;
#6539 = CARTESIAN_POINT ( 'NONE',  ( 25.64708010899964563, 91.37928813995172561, 66.32331961783411600 ) ) ;
#6541 = CARTESIAN_POINT ( 'NONE',  ( 2.433796855181233454, 96.28145139437833677, -109.1007109081216129 ) ) ;
#6542 = CARTESIAN_POINT ( 'NONE',  ( -1.619063947482197729, 11.94059994246222622, 44.80407745103770623 ) ) ;
#6543 = CARTESIAN_POINT ( 'NONE',  ( -6.588769196390762417, 44.25609997968906839, -26.02756986588556742 ) ) ;
#6544 = DIRECTION ( 'NONE',  ( -1.000000000000000000, -0.000000000000000000, -0.000000000000000000 ) ) ;
#6545 = VERTEX_POINT ( 'NONE', #23954 ) ;
#6546 = CARTESIAN_POINT ( 'NONE',  ( -1.619063947482201282, 11.94059994246159384, -44.80407745103787676 ) ) ;
#6547 = CARTESIAN_POINT ( 'NONE',  ( -1.619063947482194177, 25.20140673341374438, -38.92136151114915066 ) ) ;
#6548 = CARTESIAN_POINT ( 'NONE',  ( 28.43349137099833257, -86.10800331998733270, -89.57679848841901560 ) ) ;
#6549 = ORIENTED_EDGE ( 'NONE', *, *, #8425, .F. ) ;
#6550 = VERTEX_POINT ( 'NONE', #4214 ) ;
#6551 = CARTESIAN_POINT ( 'NONE',  ( -1.539763995773680172, -16.63252574783015092, 43.19716353142347742 ) ) ;
#6552 = VECTOR ( 'NONE', #10338, 999.9999999999998863 ) ;
#6553 = ORIENTED_EDGE ( 'NONE', *, *, #27078, .F. ) ;
#6554 = CARTESIAN_POINT ( 'NONE',  ( -1.619063947482197729, -11.94059994246129008, 44.80407745103795492 ) ) ;
#6555 = VECTOR ( 'NONE', #27266, 1000.000000000000114 ) ;
#6556 = ORIENTED_EDGE ( 'NONE', *, *, #13903, .F. ) ;
#6557 =( BOUNDED_SURFACE ( )  B_SPLINE_SURFACE ( 3, 1, ( 
 ( #4070, #1350 ),
 ( #1907, #6250 ),
 ( #15003, #27544 ),
 ( #3508, #7855 ) ),
 .UNSPECIFIED., .F., .F., .F. ) 
 B_SPLINE_SURFACE_WITH_KNOTS ( ( 4, 4 ),
 ( 2, 2 ),
 ( 0.000000000000000000, 1.000000000000000000 ),
 ( 0.000000000000000000, 1.000000000000000000 ),
 .UNSPECIFIED. ) 
 GEOMETRIC_REPRESENTATION_ITEM ( )  RATIONAL_B_SPLINE_SURFACE ( (
 ( 1.000000000000000000, 1.000000000000000000),
 ( 0.9934239774497838349, 0.8357310067453913582),
 ( 0.9934239774497838349, 0.8357310067453913582),
 ( 1.000000000000000000, 1.000000000000000000) ) ) 
 REPRESENTATION_ITEM ( '' )  SURFACE ( )  );
#6558 = CARTESIAN_POINT ( 'NONE',  ( -1.019300379054419725, 42.90269154183429379, -16.06793277092006988 ) ) ;
#6559 = FACE_OUTER_BOUND ( 'NONE', #16555, .T. ) ;
#6560 = EDGE_LOOP ( 'NONE', ( #25256, #19297, #5796, #3024 ) ) ;
#6561 = CARTESIAN_POINT ( 'NONE',  ( -55.24390624410018802, -0.009209468562450790971, 0.004896917417127758312 ) ) ;
#6562 = CARTESIAN_POINT ( 'NONE',  ( 55.49584447822657296, -7.317474139116119325, 72.18163437663937998 ) ) ;
#6563 = CARTESIAN_POINT ( 'NONE',  ( 1.833206308920113825, 126.0392061186632304, -71.90885838897261806 ) ) ;
#6564 = CARTESIAN_POINT ( 'NONE',  ( -1.045287976400365970, -37.92705037016778391, -25.66401692419976399 ) ) ;
#6565 = EDGE_CURVE ( 'NONE', #2087, #26529, #3152, .T. ) ;
#6566 = CARTESIAN_POINT ( 'NONE',  ( 9.884929003653608603, -71.59798461011239112, -132.4189379373577822 ) ) ;
#6567 = CARTESIAN_POINT ( 'NONE',  ( 1.894214914920933301, 144.2521558665609405, -16.12044375672139296 ) ) ;
#6568 = EDGE_CURVE ( 'NONE', #27740, #5273, #23772, .T. ) ;
#6569 = VECTOR ( 'NONE', #14593, 1000.000000000000000 ) ;
#6570 = FACE_OUTER_BOUND ( 'NONE', #22624, .T. ) ;
#6571 = LINE ( 'NONE', #24136, #18966 ) ;
#6572 = CARTESIAN_POINT ( 'NONE',  ( -25.21435515916025594, 1.749597353048488237E-16, -4.373993382621220594E-17 ) ) ;
#6573 = ADVANCED_FACE ( 'NONE', ( #24531 ), #5732, .F. ) ;
#6574 = ORIENTED_EDGE ( 'NONE', *, *, #5528, .T. ) ;
#6575 = VERTEX_POINT ( 'NONE', #15421 ) ;
#6576 = CARTESIAN_POINT ( 'NONE',  ( 25.64681081121879203, 83.63051021306002042, -75.86069728268907397 ) ) ;
#6577 = CARTESIAN_POINT ( 'NONE',  ( 109.1587776205901577, 0.002185517590245255552, 0.006995903587858435038 ) ) ;
#6578 = CARTESIAN_POINT ( 'NONE',  ( 5.340103579038293802, 143.7310399932982250, -32.90561047415462070 ) ) ;
#6579 = CARTESIAN_POINT ( 'NONE',  ( 24.01988960052059241, 61.78678588190025778, 115.5642432877694290 ) ) ;
#6580 = CARTESIAN_POINT ( 'NONE',  ( 25.69398547355838502, -90.93418986874847576, 66.98507266663722248 ) ) ;
#6581 = CARTESIAN_POINT ( 'NONE',  ( 25.87036335909428075, 90.88222105969153120, -67.25332031939053934 ) ) ;
#6582 = ADVANCED_FACE ( 'NONE', ( #13134 ), #20241, .T. ) ;
#6583 = B_SPLINE_CURVE_WITH_KNOTS ( 'NONE', 3,
 ( #24324, #17683, #4585, #24622, #19566, #15233, #17399, #2418 ),
 .UNSPECIFIED., .F., .F.,
 ( 4, 2, 2, 4 ),
 ( 0.000000000000000000, 0.002761524886576653681, 0.005523049773153307362, 0.01104609954630661472 ),
 .UNSPECIFIED. ) ;
#6584 = ORIENTED_EDGE ( 'NONE', *, *, #12391, .F. ) ;
#6585 = CARTESIAN_POINT ( 'NONE',  ( 2.063896406836605024, 57.85593781835414973, 133.2511741302122346 ) ) ;
#6586 = CARTESIAN_POINT ( 'NONE',  ( -6.588769196390763305, 26.02756986588603993, 44.25609997968876996 ) ) ;
#6587 = CARTESIAN_POINT ( 'NONE',  ( -1.239374126674604337, -38.61989855450920572, 25.08410696974284448 ) ) ;
#6588 = CARTESIAN_POINT ( 'NONE',  ( 25.64704443564077252, 112.2786464378873603, 11.93517308299176349 ) ) ;
#6589 = CARTESIAN_POINT ( 'NONE',  ( 25.64692232868535626, 110.3753891203789266, -23.79507962493517326 ) ) ;
#6590 = ORIENTED_EDGE ( 'NONE', *, *, #226, .F. ) ;
#6591 = CIRCLE ( 'NONE', #26788, 37.50000000000001421 ) ;
#6592 = CARTESIAN_POINT ( 'NONE',  ( 109.1624594426973118, 0.01438905500501946530, -0.006914244825467830320 ) ) ;
#6593 = DIRECTION ( 'NONE',  ( 0.7637818620346800147, -0.6451161201712182214, -0.02150485345384170119 ) ) ;
#6594 = EDGE_LOOP ( 'NONE', ( #8188, #4477, #13126, #16065 ) ) ;
#6595 = CARTESIAN_POINT ( 'NONE',  ( 2.433796855181233454, -138.8296532063085351, -43.58222566461785163 ) ) ;
#6596 = VECTOR ( 'NONE', #20188, 1000.000000000000114 ) ;
#6597 = CARTESIAN_POINT ( 'NONE',  ( -25.21435515916043357, -25.00736669481038987, -23.92354251275926558 ) ) ;
#6598 = CARTESIAN_POINT ( 'NONE',  ( -28.13707043255157103, 6.342158660427001493, -22.00298671236742010 ) ) ;
#6599 = VERTEX_POINT ( 'NONE', #22211 ) ;
#6600 = B_SPLINE_CURVE_WITH_KNOTS ( 'NONE', 3,
 ( #20563, #846, #25051, #9786, #21128, #1414, #18555 ),
 .UNSPECIFIED., .F., .F.,
 ( 4, 3, 4 ),
 ( 3.179800655392250756E-17, 0.02816610861753246833, 0.04000277880656213925 ),
 .UNSPECIFIED. ) ;
#6601 = FACE_OUTER_BOUND ( 'NONE', #16229, .T. ) ;
#6602 = DIRECTION ( 'NONE',  ( 0.000000000000000000, 0.000000000000000000, -1.000000000000000000 ) ) ;
#6603 = FACE_OUTER_BOUND ( 'NONE', #19119, .T. ) ;
#6604 = CARTESIAN_POINT ( 'NONE',  ( 55.79472521941426777, 0.7279028900803861113, -72.75035398477135118 ) ) ;
#6605 = CARTESIAN_POINT ( 'NONE',  ( 6.224689322667647851, -144.2687111683197543, 33.28770499679286843 ) ) ;
#6606 = ADVANCED_FACE ( 'NONE', ( #4930 ), #2768, .F. ) ;
#6607 = CARTESIAN_POINT ( 'NONE',  ( 25.64681081121879203, -91.10197563707990298, 66.70335573067838197 ) ) ;
#6608 = VECTOR ( 'NONE', #7202, 1000.000000000000114 ) ;
#6609 = CARTESIAN_POINT ( 'NONE',  ( 10.93730112725945602, 104.7670965581007607, 108.9902118373744742 ) ) ;
#6610 = CARTESIAN_POINT ( 'NONE',  ( 99.22246935314079508, 90.00000000000005684, -40.00000000000000711 ) ) ;
#6611 = CARTESIAN_POINT ( 'NONE',  ( -1.619063947482201282, -16.67502769180592992, -43.26576862488428077 ) ) ;
#6612 = ORIENTED_EDGE ( 'NONE', *, *, #6410, .T. ) ;
#6613 = ADVANCED_FACE ( 'NONE', ( #17736 ), #17642, .F. ) ;
#6614 = ORIENTED_EDGE ( 'NONE', *, *, #21785, .F. ) ;
#6615 = B_SPLINE_CURVE_WITH_KNOTS ( 'NONE', 3,
 ( #8238, #23085, #12396, #5654, #27660, #8384, #9981 ),
 .UNSPECIFIED., .F., .F.,
 ( 4, 3, 4 ),
 ( 0.000000000000000000, 0.02398743853561352557, 0.04000277880656219476 ),
 .UNSPECIFIED. ) ;
#6616 = LINE ( 'NONE', #26590, #23966 ) ;
#6617 = CARTESIAN_POINT ( 'NONE',  ( -12.82751273423882843, 44.03362901247002981, -21.21958768041810117 ) ) ;
#6618 = CARTESIAN_POINT ( 'NONE',  ( -8.786685647604885574, 6.617461520090397715E-15, -53.53553390275978785 ) ) ;
#6619 = LINE ( 'NONE', #13350, #6036 ) ;
#6620 = CARTESIAN_POINT ( 'NONE',  ( 26.11404676487257603, 55.62948129436244926, 98.61392875273382685 ) ) ;
#6621 = DIRECTION ( 'NONE',  ( -0.7637818620346800147, -0.3617919495470753866, 0.5345501402766286159 ) ) ;
#6622 = EDGE_LOOP ( 'NONE', ( #12454, #17141, #8309, #22019 ) ) ;
#6623 = DIRECTION ( 'NONE',  ( 0.7637818620346800147, -0.6201872550346642088, 0.1788995134688892708 ) ) ;
#6624 = CARTESIAN_POINT ( 'NONE',  ( -55.24728320129491266, -0.0006547948648734058493, -0.01453410071985278100 ) ) ;
#6625 = CARTESIAN_POINT ( 'NONE',  ( -1.048171036023496594, -36.44209502233728415, -27.73816396939552931 ) ) ;
#6626 = FACE_OUTER_BOUND ( 'NONE', #10019, .T. ) ;
#6628 = CARTESIAN_POINT ( 'NONE',  ( 26.28373643307407548, -125.5716026420346765, -22.43832507403785215 ) ) ;
#6627 = B_SPLINE_CURVE_WITH_KNOTS ( 'NONE', 3,
 ( #2884, #18410, #20718, #11946, #13665, #7216, #7652, #24779, #18260, #27481 ),
 .UNSPECIFIED., .F., .F.,
 ( 4, 3, 3, 4 ),
 ( 1.387778780781445676E-17, 0.0002669559177086302604, 0.0005339118354151229078, 0.001067817517169169237 ),
 .UNSPECIFIED. ) ;
#6629 = CARTESIAN_POINT ( 'NONE',  ( -7.711401346138435642, 45.70592430511758408, 25.75361633141439199 ) ) ;
#6630 = CARTESIAN_POINT ( 'NONE',  ( 25.64681081121879203, 12.21581276189956711, -112.2483031020012305 ) ) ;
#6631 = B_SPLINE_CURVE_WITH_KNOTS ( 'NONE', 3,
 ( #27568, #21379, #7884, #3532, #1234, #18944, #1373, #1654, #19087, #25439 ),
 .UNSPECIFIED., .F., .F.,
 ( 4, 2, 2, 2, 4 ),
 ( 8.420559318810145779E-18, 0.0003346267210630978796, 0.0006692534421261874108, 0.001003880163189276942, 0.001338506884252366365 ),
 .UNSPECIFIED. ) ;
#6632 = CARTESIAN_POINT ( 'NONE',  ( 1.833485406944043827, -117.0814567582538501, -85.72460230293812344 ) ) ;
#6633 = VERTEX_POINT ( 'NONE', #11548 ) ;
#6634 = VERTEX_POINT ( 'NONE', #37 ) ;
#6635 = ORIENTED_EDGE ( 'NONE', *, *, #4637, .T. ) ;
#6636 = CARTESIAN_POINT ( 'NONE',  ( 109.1624594426973118, 0.006914244825467785217, 0.01438905500501948959 ) ) ;
#6637 = CARTESIAN_POINT ( 'NONE',  ( 109.1586900883932856, -0.003656351050324928211, 0.006130969560693650365 ) ) ;
#6638 = CARTESIAN_POINT ( 'NONE',  ( -1.019300379054419725, 25.26451264419644716, -38.21680004809172004 ) ) ;
#6639 =( BOUNDED_SURFACE ( )  B_SPLINE_SURFACE ( 3, 1, ( 
 ( #20832, #3547 ),
 ( #12198, #1390 ),
 ( #27300, #10198 ),
 ( #1537, #9907 ) ),
 .UNSPECIFIED., .F., .F., .F. ) 
 B_SPLINE_SURFACE_WITH_KNOTS ( ( 4, 4 ),
 ( 2, 2 ),
 ( 0.000000000000000000, 1.000000000000000000 ),
 ( 0.000000000000000000, 1.000000000000000000 ),
 .UNSPECIFIED. ) 
 GEOMETRIC_REPRESENTATION_ITEM ( )  RATIONAL_B_SPLINE_SURFACE ( (
 ( 1.000000000000000000, 1.000000000000000000),
 ( 0.6386103224230302855, 0.9954351624131538845),
 ( 0.6386103224230302855, 0.9954351624131538845),
 ( 1.000000000000000000, 1.000000000000000000) ) ) 
 REPRESENTATION_ITEM ( '' )  SURFACE ( )  );
#6640 = ORIENTED_EDGE ( 'NONE', *, *, #23679, .F. ) ;
#6641 = CARTESIAN_POINT ( 'NONE',  ( 1.833485406944043827, 72.09189602597706426, 125.9346397303438039 ) ) ;
#6642 = ADVANCED_FACE ( 'NONE', ( #4640 ), #19327, .T. ) ;
#6643 = CARTESIAN_POINT ( 'NONE',  ( 2.433796855181205476, -109.1007109081232471, 96.28145139437646094 ) ) ;
#6644 = ORIENTED_EDGE ( 'NONE', *, *, #1602, .T. ) ;
#6645 = CARTESIAN_POINT ( 'NONE',  ( -1.464342487929864323, -25.15873223207664466, 38.76467504336611114 ) ) ;
#6646 = EDGE_CURVE ( 'NONE', #12003, #704, #779, .T. ) ;
#6647 = B_SPLINE_CURVE_WITH_KNOTS ( 'NONE', 3,
 ( #1290, #13849, #20472, #11702, #757, #8207, #18856, #18293 ),
 .UNSPECIFIED., .F., .F.,
 ( 4, 2, 2, 4 ),
 ( 6.938893903907228378E-18, 0.0002429588503611289385, 0.0004859177007222509380, 0.0009718354014444895161 ),
 .UNSPECIFIED. ) ;
#6648 = VERTEX_POINT ( 'NONE', #8832 ) ;
#6649 = CARTESIAN_POINT ( 'NONE',  ( -4.473127245936434626, 41.70021447285091654, 26.34600523034491815 ) ) ;
#6650 = CARTESIAN_POINT ( 'NONE',  ( -55.24300891470650754, -0.005486913146700035313, 0.008142823778062066586 ) ) ;
#6651 = EDGE_CURVE ( 'NONE', #10661, #16635, #18628, .T. ) ;
#6652 = B_SPLINE_CURVE_WITH_KNOTS ( 'NONE', 3,
 ( #23961, #6681, #4363, #15284, #4494, #21923, #1912, #15137 ),
 .UNSPECIFIED., .F., .F.,
 ( 4, 2, 2, 4 ),
 ( 2.223105199230524488E-16, 0.002761568181852866802, 0.005523136363705516763, 0.01104627272741080628 ),
 .UNSPECIFIED. ) ;
#6653 = CARTESIAN_POINT ( 'NONE',  ( 1.833485406944043827, -0.5339064996894915538, 145.1085452359073145 ) ) ;
#6654 = CARTESIAN_POINT ( 'NONE',  ( -1.619063947482194177, 25.20140673341374438, -38.92136151114915066 ) ) ;
#6655 =( BOUNDED_SURFACE ( )  B_SPLINE_SURFACE ( 3, 1, ( 
 ( #1895, #19463 ),
 ( #13392, #23941 ),
 ( #16, #10972 ),
 ( #172, #12978 ) ),
 .UNSPECIFIED., .F., .F., .F. ) 
 B_SPLINE_SURFACE_WITH_KNOTS ( ( 4, 4 ),
 ( 2, 2 ),
 ( 0.000000000000000000, 1.000000000000000000 ),
 ( 0.000000000000000000, 1.000000000000000000 ),
 .UNSPECIFIED. ) 
 GEOMETRIC_REPRESENTATION_ITEM ( )  RATIONAL_B_SPLINE_SURFACE ( (
 ( 1.000000000000000000, 1.000000000000000000),
 ( 0.6386103224230302855, 0.9954351624131538845),
 ( 0.6386103224230302855, 0.9954351624131538845),
 ( 1.000000000000000000, 1.000000000000000000) ) ) 
 REPRESENTATION_ITEM ( '' )  SURFACE ( )  );
#6656 = CARTESIAN_POINT ( 'NONE',  ( -55.24390624410018802, 0.001811362924359719581, 0.01027195578987765215 ) ) ;
#6657 = CARTESIAN_POINT ( 'NONE',  ( 26.11404676487257603, 33.91085499298377925, 108.0249973236468577 ) ) ;
#6658 = CARTESIAN_POINT ( 'NONE',  ( -7.733045908741322805, -45.70676731105703539, 25.81515396910911875 ) ) ;
#6659 = FACE_OUTER_BOUND ( 'NONE', #25396, .T. ) ;
#6660 = CARTESIAN_POINT ( 'NONE',  ( 1.833603222531973831, 14.72553080638994594, 144.3605362014088769 ) ) ;
#6661 = CARTESIAN_POINT ( 'NONE',  ( 30.59138290137879679, -9.457588828075969900, 115.8270707793589196 ) ) ;
#6662 = EDGE_LOOP ( 'NONE', ( #8585, #27210, #21299, #17706 ) ) ;
#6663 = ORIENTED_EDGE ( 'NONE', *, *, #9267, .T. ) ;
#6664 = CARTESIAN_POINT ( 'NONE',  ( 2.108393763691192468, -126.4628696952924116, 71.53437599919774925 ) ) ;
#6665 = LINE ( 'NONE', #12563, #15262 ) ;
#6666 = VERTEX_POINT ( 'NONE', #17867 ) ;
#6667 = ORIENTED_EDGE ( 'NONE', *, *, #20530, .F. ) ;
#6668 = ORIENTED_EDGE ( 'NONE', *, *, #10400, .T. ) ;
#6669 = CARTESIAN_POINT ( 'NONE',  ( -20.24419206586951603, -1.282847120831435594, -29.61012937815439372 ) ) ;
#6670 = B_SPLINE_CURVE_WITH_KNOTS ( 'NONE', 3,
 ( #14130, #1329, #18900, #27671, #7987, #11987, #23375 ),
 .UNSPECIFIED., .F., .F.,
 ( 4, 3, 4 ),
 ( 4.201076225734585017E-16, 0.02816610861753247180, 0.04000277880656250701 ),
 .UNSPECIFIED. ) ;
#6671 = EDGE_CURVE ( 'NONE', #25959, #14622, #21021, .T. ) ;
#6672 = CARTESIAN_POINT ( 'NONE',  ( 1.832998868059858122, -107.4798986104866572, 97.49378069860762253 ) ) ;
#6673 = B_SPLINE_CURVE_WITH_KNOTS ( 'NONE', 3,
 ( #11170, #6293, #8583, #6856, #26137, #28421, #360, #1950 ),
 .UNSPECIFIED., .F., .F.,
 ( 4, 2, 2, 4 ),
 ( 7.757919228897728493E-18, 0.0002429592666046767060, 0.0004859185332093456599, 0.0009718370664186836219 ),
 .UNSPECIFIED. ) ;
#6674 = CARTESIAN_POINT ( 'NONE',  ( 25.73574536432415982, 11.00659994954150278, 112.4329083163018481 ) ) ;
#6675 = EDGE_CURVE ( 'NONE', #11364, #13776, #3728, .T. ) ;
#6676 = CARTESIAN_POINT ( 'NONE',  ( 2.430230287190589422, -145.5073573687466819, 1.451610819317230572 ) ) ;
#6677 = CARTESIAN_POINT ( 'NONE',  ( 109.1587776205901861, 0.006305329297950502086, -0.003736572840496154083 ) ) ;
#6678 = CARTESIAN_POINT ( 'NONE',  ( -1.619063947482197729, 29.22875152547757338, -35.99532424477389725 ) ) ;
#6679 = B_SPLINE_CURVE_WITH_KNOTS ( 'NONE', 3,
 ( #10255, #5634, #21018, #14826, #1302, #19016, #12250, #25361, #27797, #23639 ),
 .UNSPECIFIED., .F., .F.,
 ( 4, 3, 3, 4 ),
 ( 3.295974604355933479E-17, 0.0002669559177086193642, 0.0005339118354150988385, 0.001067817517169165550 ),
 .UNSPECIFIED. ) ;
#6680 = CARTESIAN_POINT ( 'NONE',  ( -22.23342874802668234, 30.68433055777684970, -7.677086057585063017 ) ) ;
#6681 = CARTESIAN_POINT ( 'NONE',  ( -2.265401668238144151, 36.42007794497294526, 29.73100299756526965 ) ) ;
#6682 = CARTESIAN_POINT ( 'NONE',  ( 28.43349137099830415, -105.5221910860621932, 65.60227321965550118 ) ) ;
#6683 = CARTESIAN_POINT ( 'NONE',  ( -1.048172774974298616, 27.73787987941060607, 36.44231470008685392 ) ) ;
#6684 = CARTESIAN_POINT ( 'NONE',  ( 16.05277956358200342, 103.3141821208296562, -99.31161228512374350 ) ) ;
#6685 =( BOUNDED_SURFACE ( )  B_SPLINE_SURFACE ( 3, 1, ( 
 ( #19151, #3893 ),
 ( #17260, #4162 ),
 ( #17123, #14823 ),
 ( #21446, #16861 ) ),
 .UNSPECIFIED., .F., .F., .F. ) 
 B_SPLINE_SURFACE_WITH_KNOTS ( ( 4, 4 ),
 ( 2, 2 ),
 ( 0.000000000000000000, 1.000000000000000000 ),
 ( 0.000000000000000000, 1.000000000000000000 ),
 .UNSPECIFIED. ) 
 GEOMETRIC_REPRESENTATION_ITEM ( )  RATIONAL_B_SPLINE_SURFACE ( (
 ( 1.000000000000000000, 1.000000000000000000),
 ( 0.9960225298536222738, 0.9999952330161893110),
 ( 0.9960225298536222738, 0.9999952330161893110),
 ( 1.000000000000000000, 1.000000000000000000) ) ) 
 REPRESENTATION_ITEM ( '' )  SURFACE ( )  );
#6686 = ORIENTED_EDGE ( 'NONE', *, *, #18420, .F. ) ;
#6687 = ORIENTED_EDGE ( 'NONE', *, *, #21067, .T. ) ;
#6689 = CARTESIAN_POINT ( 'NONE',  ( -4.178947244162641184, -47.46809051147732106, -11.88256963646720266 ) ) ;
#6688 = CARTESIAN_POINT ( 'NONE',  ( 25.64704443564076541, 91.26857357624568579, 66.47548630737885844 ) ) ;
#6690 = CARTESIAN_POINT ( 'NONE',  ( 1.833838850855461500, -144.3055354793886522, -15.25659494068255384 ) ) ;
#6691 = CARTESIAN_POINT ( 'NONE',  ( -1.058197053496169548, 38.06270006878853707, -25.48582931365482906 ) ) ;
#6692 = CARTESIAN_POINT ( 'NONE',  ( 25.70243777736187241, 0.7331659071611001943, -112.9457924277214005 ) ) ;
#6693 = CARTESIAN_POINT ( 'NONE',  ( 32.73300124599737160, -75.82012867748541396, 89.94078864464039214 ) ) ;
#6694 = ORIENTED_EDGE ( 'NONE', *, *, #17960, .F. ) ;
#6695 = CARTESIAN_POINT ( 'NONE',  ( 2.108393763691204903, 145.2872457912032758, 1.280847988472279431 ) ) ;
#6696 = ORIENTED_EDGE ( 'NONE', *, *, #16505, .T. ) ;
#6697 = CARTESIAN_POINT ( 'NONE',  ( 28.37644542392835234, 86.16884085958076867, -89.64009552702822248 ) ) ;
#6698 = CARTESIAN_POINT ( 'NONE',  ( -20.20700224038492721, -29.58392382092672790, 0.9908225410481621420 ) ) ;
#6699 = ORIENTED_EDGE ( 'NONE', *, *, #4961, .T. ) ;
#6700 = ORIENTED_EDGE ( 'NONE', *, *, #10589, .T. ) ;
#6701 = CARTESIAN_POINT ( 'NONE',  ( 119.2224693531408803, 0.000000000000000000, 19.99999999999997513 ) ) ;
#6702 = VERTEX_POINT ( 'NONE', #1048 ) ;
#6703 = CARTESIAN_POINT ( 'NONE',  ( -16.86833981943424021, -39.83928801320577406, 19.19877306373892978 ) ) ;
#6704 = VERTEX_POINT ( 'NONE', #12269 ) ;
#6705 = CARTESIAN_POINT ( 'NONE',  ( 25.87036335909428786, 67.25332031939144883, 90.88222105969083486 ) ) ;
#6706 = ADVANCED_FACE ( 'NONE', ( #25381 ), #24298, .F. ) ;
#6707 = EDGE_CURVE ( 'NONE', #23277, #6842, #4537, .T. ) ;
#6708 = ORIENTED_EDGE ( 'NONE', *, *, #28376, .T. ) ;
#6709 = CARTESIAN_POINT ( 'NONE',  ( 1.833485406944043827, 144.3694338680886915, -14.63699153649211127 ) ) ;
#6710 = CARTESIAN_POINT ( 'NONE',  ( -20.37983603106073716, 27.81368274044725553, 10.62371319148611981 ) ) ;
#6711 = CARTESIAN_POINT ( 'NONE',  ( 109.1592201516379674, -0.006649399203953433417, 0.004194960840990133617 ) ) ;
#6712 = CARTESIAN_POINT ( 'NONE',  ( -90.83090735639699176, 2.449293598294706119E-15, 20.00000000000000000 ) ) ;
#6713 = CARTESIAN_POINT ( 'NONE',  ( 109.1721716018069657, -0.007126480965770814156, -0.01550977894512763945 ) ) ;
#6714 = CARTESIAN_POINT ( 'NONE',  ( 25.98107933586726404, -1.091357942391386615, 113.1286487641201006 ) ) ;
#6715 = CARTESIAN_POINT ( 'NONE',  ( -1.239374126674604337, 38.61989855450939046, -25.08410696974256027 ) ) ;
#6716 = ORIENTED_EDGE ( 'NONE', *, *, #22245, .F. ) ;
#6717 = CARTESIAN_POINT ( 'NONE',  ( 25.87036335909426654, 83.35447252092961890, -76.38467849957065425 ) ) ;
#6719 = CARTESIAN_POINT ( 'NONE',  ( -8.786685647604896232, 23.24040270374459993, 48.22796981442743913 ) ) ;
#6718 = CARTESIAN_POINT ( 'NONE',  ( -28.41354790283022069, 18.00456980371921034, 14.62505768302780851 ) ) ;
#6720 = B_SPLINE_CURVE_WITH_KNOTS ( 'NONE', 3,
 ( #5, #13377, #4760, #11236 ),
 .UNSPECIFIED., .F., .F.,
 ( 4, 4 ),
 ( 1.040834085586084257E-17, 0.008383560773332680849 ),
 .UNSPECIFIED. ) ;
#6721 = DIRECTION ( 'NONE',  ( 0.000000000000000000, 5.223019709708233256E-21, -1.000000000000000000 ) ) ;
#6722 = CARTESIAN_POINT ( 'NONE',  ( 19.66333377628701840, 127.6002314355565659, -51.89484018353712003 ) ) ;
#6723 = CARTESIAN_POINT ( 'NONE',  ( -7.078251931573400491, 47.71415099571833451, 20.86696228105175166 ) ) ;
#6724 = VERTEX_POINT ( 'NONE', #11841 ) ;
#6725 = CARTESIAN_POINT ( 'NONE',  ( 1.833206308920100058, -107.3376449983721130, -97.64934899952810099 ) ) ;
#6726 = CARTESIAN_POINT ( 'NONE',  ( 28.37603512858356325, 114.7183465482399782, -1.794342805483269965 ) ) ;
#6727 = CARTESIAN_POINT ( 'NONE',  ( 25.64681081121879203, 112.3352186517030731, 11.38886654529711961 ) ) ;
#6728 = CARTESIAN_POINT ( 'NONE',  ( 109.1586900883932856, 0.004851151255031855604, -0.005236795036868175865 ) ) ;
#6729 = B_SPLINE_CURVE_WITH_KNOTS ( 'NONE', 3,
 ( #6060, #26040, #12652, #16976, #28049, #8208, #25767, #14814, #23475, #21436 ),
 .UNSPECIFIED., .F., .F.,
 ( 4, 3, 3, 4 ),
 ( 1.387778780781445676E-17, 0.0002669560319015715504, 0.0005492286108966297443, 0.0008315040496093390431 ),
 .UNSPECIFIED. ) ;
#6730 = ORIENTED_EDGE ( 'NONE', *, *, #12160, .F. ) ;
#6731 = CARTESIAN_POINT ( 'NONE',  ( 55.49584447822657296, -14.82242356767984326, 71.02133150427250996 ) ) ;
#6732 =( BOUNDED_SURFACE ( )  B_SPLINE_SURFACE ( 3, 1, ( 
 ( #23575, #19507 ),
 ( #1941, #2074 ),
 ( #4107, #10879 ),
 ( #15168, #28411 ) ),
 .UNSPECIFIED., .F., .F., .F. ) 
 B_SPLINE_SURFACE_WITH_KNOTS ( ( 4, 4 ),
 ( 2, 2 ),
 ( 0.000000000000000000, 1.000000000000000000 ),
 ( 0.000000000000000000, 1.000000000000000000 ),
 .UNSPECIFIED. ) 
 GEOMETRIC_REPRESENTATION_ITEM ( )  RATIONAL_B_SPLINE_SURFACE ( (
 ( 1.000000000000000000, 1.000000000000000000),
 ( 0.6386103224230302855, 0.9954351624131538845),
 ( 0.6386103224230302855, 0.9954351624131538845),
 ( 1.000000000000000000, 1.000000000000000000) ) ) 
 REPRESENTATION_ITEM ( '' )  SURFACE ( )  );
#6733 = EDGE_CURVE ( 'NONE', #22385, #13658, #420, .T. ) ;
#6734 = CARTESIAN_POINT ( 'NONE',  ( 10.93730112725990367, -142.1801301103781157, -51.37919228020433593 ) ) ;
#6735 = CARTESIAN_POINT ( 'NONE',  ( 1.833809397773885630, -97.22957127128904631, 107.7184108265659859 ) ) ;
#6736 = ORIENTED_EDGE ( 'NONE', *, *, #14506, .T. ) ;
#6737 = FACE_OUTER_BOUND ( 'NONE', #21262, .T. ) ;
#6738 = EDGE_CURVE ( 'NONE', #6333, #9063, #24809, .T. ) ;
#6739 = CARTESIAN_POINT ( 'NONE',  ( -1.045287976400362417, -1.530335034934427574, -45.76855895860943235 ) ) ;
#6740 = ORIENTED_EDGE ( 'NONE', *, *, #26003, .F. ) ;
#6741 = B_SPLINE_CURVE_WITH_KNOTS ( 'NONE', 3,
 ( #16921, #3670, #27424, #16343, #10030, #22992, #16490, #3253 ),
 .UNSPECIFIED., .F., .F.,
 ( 4, 2, 2, 4 ),
 ( 1.250926888277100303E-17, 0.0002429592666046815307, 0.0004859185332093505388, 0.0009718370664186885008 ),
 .UNSPECIFIED. ) ;
#6742 = EDGE_CURVE ( 'NONE', #11657, #5017, #1784, .T. ) ;
#6743 = CARTESIAN_POINT ( 'NONE',  ( 25.69398547355838502, 55.82723250638906620, -98.18017599249780858 ) ) ;
#6744 = PLANE ( 'NONE',  #9361 ) ;
#6745 = DIRECTION ( 'NONE',  ( -0.5946245182733607137, -0.6487139525627746428, 0.4749651461092231908 ) ) ;
#6746 = CARTESIAN_POINT ( 'NONE',  ( -20.57838717382308147, 16.28767523336121315, -25.16001208503110931 ) ) ;
#6747 = CARTESIAN_POINT ( 'NONE',  ( 25.64681081121879203, 110.5293738517608375, 23.06870491922360245 ) ) ;
#6748 = VERTEX_POINT ( 'NONE', #18292 ) ;
#6749 = CARTESIAN_POINT ( 'NONE',  ( 109.1589550718174877, 0.001014448720240637355, -0.007507020724817408015 ) ) ;
#6750 = CARTESIAN_POINT ( 'NONE',  ( -8.786685647604885574, 6.096987947571466530E-17, -1.524246986892866633E-17 ) ) ;
#6751 = CARTESIAN_POINT ( 'NONE',  ( 25.98552792386801258, -47.00040718953707142, -102.9121737515625199 ) ) ;
#6752 = FACE_OUTER_BOUND ( 'NONE', #21366, .T. ) ;
#6753 = ORIENTED_EDGE ( 'NONE', *, *, #5615, .F. ) ;
#6754 = ORIENTED_EDGE ( 'NONE', *, *, #3257, .T. ) ;
#6755 = ORIENTED_EDGE ( 'NONE', *, *, #8248, .T. ) ;
#6756 = CARTESIAN_POINT ( 'NONE',  ( -20.24419206586952313, -29.61012937815440083, 1.282847120831551280 ) ) ;
#6757 = VECTOR ( 'NONE', #7948, 1000.000000000000114 ) ;
#6758 = CARTESIAN_POINT ( 'NONE',  ( -55.24728320129491266, -0.005114031043466088153, -0.01362040845703062046 ) ) ;
#6759 = CARTESIAN_POINT ( 'NONE',  ( 25.73574536432417403, -24.27578079247234299, 110.3312765349292164 ) ) ;
#6760 = CARTESIAN_POINT ( 'NONE',  ( 2.430230287190589422, -84.35270093935336888, 118.5711603495678474 ) ) ;
#6761 = CARTESIAN_POINT ( 'NONE',  ( -1.619063947482197729, -46.30105812165550105, -2.489035965909997206 ) ) ;
#6762 = CARTESIAN_POINT ( 'NONE',  ( -12.82751273423880711, 33.78816682541337002, 35.32125660155409008 ) ) ;
#6763 = ORIENTED_EDGE ( 'NONE', *, *, #25225, .T. ) ;
#6764 = CARTESIAN_POINT ( 'NONE',  ( 2.108985857320877955, 31.46042399111245658, 141.8463279126002590 ) ) ;
#6765 = CARTESIAN_POINT ( 'NONE',  ( -4.473127245936434626, -49.22197550883367256, 3.196405119334318812 ) ) ;
#6766 = CARTESIAN_POINT ( 'NONE',  ( 25.64707127832796019, -0.04449220797097835911, 112.9112343549835487 ) ) ;
#6767 = CARTESIAN_POINT ( 'NONE',  ( -55.24728320129491266, 0.0006547948648740692726, 0.01453410071985259712 ) ) ;
#6768 = CARTESIAN_POINT ( 'NONE',  ( 25.70243777736189728, -75.03063812271992106, -84.42566495012526673 ) ) ;
#6769 = DIRECTION ( 'NONE',  ( -0.7563875759206388771, -0.5490129373055306905, -0.3556158456312839555 ) ) ;
#6770 =( BOUNDED_SURFACE ( )  B_SPLINE_SURFACE ( 3, 1, ( 
 ( #8810, #447 ),
 ( #11111, #19731 ),
 ( #15407, #9091 ),
 ( #13682, #26635 ) ),
 .UNSPECIFIED., .F., .F., .F. ) 
 B_SPLINE_SURFACE_WITH_KNOTS ( ( 4, 4 ),
 ( 2, 2 ),
 ( 0.000000000000000000, 1.000000000000000000 ),
 ( 0.000000000000000000, 1.000000000000000000 ),
 .UNSPECIFIED. ) 
 GEOMETRIC_REPRESENTATION_ITEM ( )  RATIONAL_B_SPLINE_SURFACE ( (
 ( 1.000000000000000000, 1.000000000000000000),
 ( 0.9960225298536222738, 0.9999952330161893110),
 ( 0.9960225298536222738, 0.9999952330161893110),
 ( 1.000000000000000000, 1.000000000000000000) ) ) 
 REPRESENTATION_ITEM ( '' )  SURFACE ( )  );
#6771 = EDGE_CURVE ( 'NONE', #14914, #15111, #1452, .T. ) ;
#6772 = CARTESIAN_POINT ( 'NONE',  ( 10.93730112725932635, 0.000000000000000000, 0.000000000000000000 ) ) ;
#6773 = CARTESIAN_POINT ( 'NONE',  ( 1.833721034905647862, -117.6051524288277790, -85.00517831633806054 ) ) ;
#6774 = EDGE_LOOP ( 'NONE', ( #4759, #7242, #2571, #7910 ) ) ;
#6775 = EDGE_CURVE ( 'NONE', #21576, #17227, #9680, .T. ) ;
#6776 = ORIENTED_EDGE ( 'NONE', *, *, #599, .T. ) ;
#6777 = EDGE_LOOP ( 'NONE', ( #2607, #12413, #11492, #3365 ) ) ;
#6778 = EDGE_CURVE ( 'NONE', #7362, #6115, #5527, .T. ) ;
#6779 = B_SPLINE_CURVE_WITH_KNOTS ( 'NONE', 3,
 ( #15454, #28407, #15589, #6705, #8708, #24263, #9002, #17894 ),
 .UNSPECIFIED., .F., .F.,
 ( 4, 2, 2, 4 ),
 ( 3.469446951953614189E-18, 0.0002429592666046763265, 0.0004859185332093491835, 0.0009718370664186922955 ),
 .UNSPECIFIED. ) ;
#6780 = B_SPLINE_CURVE_WITH_KNOTS ( 'NONE', 3,
 ( #22843, #2968, #16049, #27122, #25275, #9579 ),
 .UNSPECIFIED., .F., .F.,
 ( 4, 2, 4 ),
 ( 7.757919228897728493E-18, 0.003570751334075633956, 0.007141502668151267913 ),
 .UNSPECIFIED. ) ;
#6781 = CARTESIAN_POINT ( 'NONE',  ( -1.031422197589711764, -43.06660437151319343, -15.60268798220621100 ) ) ;
#6782 = CARTESIAN_POINT ( 'NONE',  ( 1.831572820252008738, 97.82994539998530570, -107.1759352627496185 ) ) ;
#6783 = CARTESIAN_POINT ( 'NONE',  ( -55.24390624410018802, 0.01027195578987812573, -0.001811362924359468263 ) ) ;
#6784 = ORIENTED_EDGE ( 'NONE', *, *, #713, .T. ) ;
#6785 = CARTESIAN_POINT ( 'NONE',  ( -21.81686047589431965, -33.92779429964186733, 18.24499610240074432 ) ) ;
#6786 = CARTESIAN_POINT ( 'NONE',  ( -1.539763995773685057, -11.93465967526326921, -44.72359274866478529 ) ) ;
#6787 = ORIENTED_EDGE ( 'NONE', *, *, #7491, .T. ) ;
#6788 = CARTESIAN_POINT ( 'NONE',  ( -1.539760825549689516, -25.17088484262114179, 38.84664866728805066 ) ) ;
#6789 = VERTEX_POINT ( 'NONE', #5358 ) ;
#6790 = CARTESIAN_POINT ( 'NONE',  ( -23.79248802219722236, 32.40806545715341258, 7.157555990716568672 ) ) ;
#6791 = LINE ( 'NONE', #15535, #12992 ) ;
#6792 = CARTESIAN_POINT ( 'NONE',  ( 109.1586059443104944, 0.006971743774739760056, 0.001198897580739020224 ) ) ;
#6793 = DIRECTION ( 'NONE',  ( -0.7563875759206388771, 0.5078650950445624535, -0.4122509917856805317 ) ) ;
#6794 = CARTESIAN_POINT ( 'NONE',  ( 1.833206310202336153, 73.19872434058787292, 125.2945016693813045 ) ) ;
#6795 = CARTESIAN_POINT ( 'NONE',  ( 32.73300124599739291, 105.8473486001057466, -51.32617430724801721 ) ) ;
#6796 = CARTESIAN_POINT ( 'NONE',  ( 30.59141879584280588, 33.33270905817592933, 111.3296561588013134 ) ) ;
#6797 = CARTESIAN_POINT ( 'NONE',  ( -20.24399999263415140, -24.70869149526192032, 16.36687688782885530 ) ) ;
#6798 = B_SPLINE_CURVE_WITH_KNOTS ( 'NONE', 3,
 ( #25135, #11594, #18067, #16195, #20374, #26846 ),
 .UNSPECIFIED., .F., .F.,
 ( 4, 2, 4 ),
 ( 4.336808689942017255E-19, 0.0006311571484585985249, 0.001262314296917196399 ),
 .UNSPECIFIED. ) ;
#6799 = CARTESIAN_POINT ( 'NONE',  ( 2.430230287190592531, -109.1043569252007615, -96.28466919684210268 ) ) ;
#6800 = CARTESIAN_POINT ( 'NONE',  ( -1.619063947482197729, -43.26576862488445130, -16.67502769180545386 ) ) ;
#6801 = CARTESIAN_POINT ( 'NONE',  ( -16.86833981943427929, -5.948101187261880085, -43.82216161736206317 ) ) ;
#6802 = CARTESIAN_POINT ( 'NONE',  ( 25.98552792386801968, -1.078856412010039678, -113.1317367103340104 ) ) ;
#6803 = ORIENTED_EDGE ( 'NONE', *, *, #24011, .F. ) ;
#6804 = ORIENTED_EDGE ( 'NONE', *, *, #14816, .T. ) ;
#6805 = CARTESIAN_POINT ( 'NONE',  ( -1.045287976400365970, 1.530335034933814731, -45.76855895860946788 ) ) ;
#6806 = CARTESIAN_POINT ( 'NONE',  ( -1.583189561560253589, -25.21827308671203127, 38.94740041318322454 ) ) ;
#6807 = ORIENTED_EDGE ( 'NONE', *, *, #5614, .T. ) ;
#6808 = EDGE_CURVE ( 'NONE', #2120, #422, #3184, .T. ) ;
#6809 = ORIENTED_EDGE ( 'NONE', *, *, #7597, .F. ) ;
#6810 = ORIENTED_EDGE ( 'NONE', *, *, #460, .T. ) ;
#6811 = ADVANCED_FACE ( 'NONE', ( #14122 ), #17469, .F. ) ;
#6812 =( BOUNDED_SURFACE ( )  B_SPLINE_SURFACE ( 3, 1, ( 
 ( #2364, #8873 ),
 ( #15461, #20211 ),
 ( #6713, #11304 ),
 ( #17773, #2511 ) ),
 .UNSPECIFIED., .F., .F., .F. ) 
 B_SPLINE_SURFACE_WITH_KNOTS ( ( 4, 4 ),
 ( 2, 2 ),
 ( 0.000000000000000000, 1.000000000000000000 ),
 ( 0.000000000000000000, 1.000000000000000000 ),
 .UNSPECIFIED. ) 
 GEOMETRIC_REPRESENTATION_ITEM ( )  RATIONAL_B_SPLINE_SURFACE ( (
 ( 1.000000000000000000, 1.000000000000000000),
 ( 0.6386103224230302855, 0.9954351624131538845),
 ( 0.6386103224230302855, 0.9954351624131538845),
 ( 1.000000000000000000, 1.000000000000000000) ) ) 
 REPRESENTATION_ITEM ( '' )  SURFACE ( )  );
#6813 = ADVANCED_FACE ( 'NONE', ( #6229 ), #16571, .F. ) ;
#6814 = EDGE_LOOP ( 'NONE', ( #10293, #5444, #4234, #3928 ) ) ;
#6815 = CARTESIAN_POINT ( 'NONE',  ( 25.65782528836482257, 11.22838748007616338, 112.3587790429870950 ) ) ;
#6816 = CARTESIAN_POINT ( 'NONE',  ( -1.045287976400383290, 28.14015102489806708, -36.12803364096618708 ) ) ;
#6817 =( BOUNDED_SURFACE ( )  B_SPLINE_SURFACE ( 3, 1, ( 
 ( #21282, #3868 ),
 ( #1563, #1825 ),
 ( #19130, #8196 ),
 ( #21698, #25750 ) ),
 .UNSPECIFIED., .F., .F., .F. ) 
 B_SPLINE_SURFACE_WITH_KNOTS ( ( 4, 4 ),
 ( 2, 2 ),
 ( 0.000000000000000000, 1.000000000000000000 ),
 ( 0.000000000000000000, 1.000000000000000000 ),
 .UNSPECIFIED. ) 
 GEOMETRIC_REPRESENTATION_ITEM ( )  RATIONAL_B_SPLINE_SURFACE ( (
 ( 1.000000000000000000, 1.000000000000000000),
 ( 0.6386103224230302855, 0.9954351624131538845),
 ( 0.6386103224230302855, 0.9954351624131538845),
 ( 1.000000000000000000, 1.000000000000000000) ) ) 
 REPRESENTATION_ITEM ( '' )  SURFACE ( )  );
#6818 = CARTESIAN_POINT ( 'NONE',  ( 1.833206310202321720, 44.13245377365817035, -138.2356391007178331 ) ) ;
#6819 = CARTESIAN_POINT ( 'NONE',  ( -25.21435515916025594, 1.749597353048488237E-16, -4.373993382621220594E-17 ) ) ;
#6820 = CARTESIAN_POINT ( 'NONE',  ( 10.93730112725978287, -136.0306644680987915, 65.95960219663069779 ) ) ;
#6821 = LINE ( 'NONE', #10853, #11188 ) ;
#6822 = CARTESIAN_POINT ( 'NONE',  ( -2.265401668238147259, -43.82493763960398070, -17.02144111536863136 ) ) ;
#6823 = CARTESIAN_POINT ( 'NONE',  ( -25.21435515916043713, -31.17620025257598471, -15.02493970636134613 ) ) ;
#6824 = AXIS2_PLACEMENT_3D ( 'NONE', #4875, #27016, #3011 ) ;
#6825 = CARTESIAN_POINT ( 'NONE',  ( 1.833603222531971388, -117.6571262511684068, 84.93295186324824897 ) ) ;
#6826 = ORIENTED_EDGE ( 'NONE', *, *, #26191, .T. ) ;
#6828 = CARTESIAN_POINT ( 'NONE',  ( 109.1778270068192853, -0.006489198140358675912, 0.006682187084639293860 ) ) ;
#6827 = DIRECTION ( 'NONE',  ( -0.5946245182733607137, 0.7655593692109006199, 0.2456431038754836038 ) ) ;
#6829 = CARTESIAN_POINT ( 'NONE',  ( -1.056502255334264895, -0.5104472526223093887, -45.80535052436396626 ) ) ;
#6830 = CARTESIAN_POINT ( 'NONE',  ( -25.21435515916025594, 1.749597353048488237E-16, -4.373993382621220594E-17 ) ) ;
#6831 = CARTESIAN_POINT ( 'NONE',  ( 25.73574536432415982, 110.3312765349293159, 24.27578079247199128 ) ) ;
#6832 = CARTESIAN_POINT ( 'NONE',  ( 16.05277956358206026, -92.36732600443268382, 109.5668455727256969 ) ) ;
#6833 = ORIENTED_EDGE ( 'NONE', *, *, #21088, .F. ) ;
#6834 = CARTESIAN_POINT ( 'NONE',  ( -1.019300379054419725, -16.06793277092022976, -42.90269154183422984 ) ) ;
#6835 = ORIENTED_EDGE ( 'NONE', *, *, #14180, .F. ) ;
#6836 = CARTESIAN_POINT ( 'NONE',  ( -25.21435515916025594, 1.749597353048488237E-16, -4.373993382621220594E-17 ) ) ;
#6837 = CARTESIAN_POINT ( 'NONE',  ( 25.98107933586717166, -12.91054317625193448, 112.3948402207513766 ) ) ;
#6838 = ORIENTED_EDGE ( 'NONE', *, *, #4532, .F. ) ;
#6839 = ORIENTED_EDGE ( 'NONE', *, *, #24229, .F. ) ;
#6840 = EDGE_CURVE ( 'NONE', #9703, #19171, #5572, .T. ) ;
#6841 = CARTESIAN_POINT ( 'NONE',  ( 1.832998868059890096, 0.5339089137747921043, 145.1092030902949830 ) ) ;
#6842 = VERTEX_POINT ( 'NONE', #16743 ) ;
#6843 = CARTESIAN_POINT ( 'NONE',  ( 1.833485406944043827, -96.69979900902094982, -108.1939177044935860 ) ) ;
#6844 = ORIENTED_EDGE ( 'NONE', *, *, #1767, .F. ) ;
#6845 = EDGE_CURVE ( 'NONE', #7588, #22237, #26508, .T. ) ;
#6846 = CARTESIAN_POINT ( 'NONE',  ( -20.20700224038492721, -28.44216453106531617, 8.199606986804630182 ) ) ;
#6847 = CIRCLE ( 'NONE', #14647, 20.00000000000000000 ) ;
#6848 = B_SPLINE_CURVE_WITH_KNOTS ( 'NONE', 3,
 ( #20260, #13644, #553, #9350, #17536, #26182, #13084 ),
 .UNSPECIFIED., .F., .F.,
 ( 4, 3, 4 ),
 ( 5.601733421463777940E-16, 0.02816610861753245099, 0.04000277880656276375 ),
 .UNSPECIFIED. ) ;
#6849 = CARTESIAN_POINT ( 'NONE',  ( -1.031422197589711987, 25.67058493451442658, -37.93675465142480618 ) ) ;
#6850 =( BOUNDED_SURFACE ( )  B_SPLINE_SURFACE ( 3, 1, ( 
 ( #21207, #3638 ),
 ( #25688, #3218 ),
 ( #3501, #18912 ),
 ( #20630, #12152 ) ),
 .UNSPECIFIED., .F., .F., .F. ) 
 B_SPLINE_SURFACE_WITH_KNOTS ( ( 4, 4 ),
 ( 2, 2 ),
 ( 0.000000000000000000, 1.000000000000000000 ),
 ( 0.000000000000000000, 1.000000000000000000 ),
 .UNSPECIFIED. ) 
 GEOMETRIC_REPRESENTATION_ITEM ( )  RATIONAL_B_SPLINE_SURFACE ( (
 ( 1.000000000000000000, 1.000000000000000000),
 ( 0.9956975270656955868, 0.8568959468854907557),
 ( 0.9956975270656955868, 0.8568959468854907557),
 ( 1.000000000000000000, 1.000000000000000000) ) ) 
 REPRESENTATION_ITEM ( '' )  SURFACE ( )  );
#6851 = CARTESIAN_POINT ( 'NONE',  ( -20.57838717382308147, -28.96176188950213870, 7.715628353033985753 ) ) ;
#6852 = CARTESIAN_POINT ( 'NONE',  ( -55.24728320129491266, -0.005114031043468280843, 0.01362040845703383143 ) ) ;
#6853 = FACE_OUTER_BOUND ( 'NONE', #18916, .T. ) ;
#6854 = CARTESIAN_POINT ( 'NONE',  ( -20.57838717382308147, -23.26537097894118133, -18.89542499756491978 ) ) ;
#6855 = CARTESIAN_POINT ( 'NONE',  ( 25.98552792386800192, -33.93357582585569787, 107.9280603639525538 ) ) ;
#6856 = CARTESIAN_POINT ( 'NONE',  ( 25.87036335909428786, -112.3329723497411123, 12.80197335559923388 ) ) ;
#6857 = FACE_OUTER_BOUND ( 'NONE', #21120, .T. ) ;
#6858 = CARTESIAN_POINT ( 'NONE',  ( -20.21097721650785672, -29.61001326827676294, 0.3305964462500739498 ) ) ;
#6859 = CARTESIAN_POINT ( 'NONE',  ( -7.733045908741323693, -52.15131830128827062, -5.980865481987962085 ) ) ;
#6860 = CARTESIAN_POINT ( 'NONE',  ( 26.11404676487257603, 110.5078194225161070, 24.64483677384886917 ) ) ;
#6861 = ADVANCED_FACE ( 'NONE', ( #27942 ), #8658, .F. ) ;
#6862 = ORIENTED_EDGE ( 'NONE', *, *, #19991, .F. ) ;
#6863 = CARTESIAN_POINT ( 'NONE',  ( -1.463510566862830986, 16.57250862017420090, -43.13857742234511505 ) ) ;
#6864 = EDGE_CURVE ( 'NONE', #174, #1609, #14851, .T. ) ;
#6865 = CARTESIAN_POINT ( 'NONE',  ( 26.11404676487257603, 110.9778746459749641, -22.43340081644658213 ) ) ;
#6866 = CARTESIAN_POINT ( 'NONE',  ( 25.64703792032471696, 112.3081285890370111, 11.65444440562218276 ) ) ;
#6867 = FACE_OUTER_BOUND ( 'NONE', #5407, .T. ) ;
#6869 = ORIENTED_EDGE ( 'NONE', *, *, #8376, .F. ) ;
#6868 = EDGE_CURVE ( 'NONE', #8671, #15588, #15109, .T. ) ;
#6870 = FACE_OUTER_BOUND ( 'NONE', #873, .T. ) ;
#6871 = CARTESIAN_POINT ( 'NONE',  ( -1.323439229708142983, -35.86372896917450959, 28.92147054731879408 ) ) ;
#6872 = EDGE_LOOP ( 'NONE', ( #145, #10101, #13017, #1009 ) ) ;
#6873 = CARTESIAN_POINT ( 'NONE',  ( -28.41354790283022069, 22.41474081378008876, 5.969609727607788408 ) ) ;
#6874 = CARTESIAN_POINT ( 'NONE',  ( 32.73300124599740002, 97.37344512919945316, -66.00340565729239017 ) ) ;
#6875 = CARTESIAN_POINT ( 'NONE',  ( -20.57838717382308147, -23.26537097894090778, 18.89542499756525729 ) ) ;
#6876 = B_SPLINE_CURVE_WITH_KNOTS ( 'NONE', 3,
 ( #24604, #2545, #22728, #13630, #2991, #11622, #822, #7459, #20394, #15628 ),
 .UNSPECIFIED., .F., .F.,
 ( 4, 3, 3, 4 ),
 ( 5.003707553108401214E-17, 0.0002669559177086285799, 0.0005339118354151193300, 0.001067817517169137144 ),
 .UNSPECIFIED. ) ;
#6877 = ORIENTED_EDGE ( 'NONE', *, *, #22325, .F. ) ;
#6878 = CARTESIAN_POINT ( 'NONE',  ( 0.000000000000000000, 0.000000000000000000, 0.000000000000000000 ) ) ;
#6879 = CARTESIAN_POINT ( 'NONE',  ( -20.57838717382308502, 28.96176188950218844, -7.715628353033780584 ) ) ;
#6880 = DIRECTION ( 'NONE',  ( 1.000000000000000000, -6.938893903907226837E-18, 1.734723475976806709E-18 ) ) ;
#6881 = CARTESIAN_POINT ( 'NONE',  ( 25.64708228042118776, -34.92896069507359869, 107.3728320282187951 ) ) ;
#6882 = FACE_OUTER_BOUND ( 'NONE', #27682, .T. ) ;
#6883 = CARTESIAN_POINT ( 'NONE',  ( 10.93730112725977932, -104.7670965581018123, 108.9902118373738062 ) ) ;
#6884 = CARTESIAN_POINT ( 'NONE',  ( 109.1586059443104944, 0.003294606663354653162, -0.006260042619943061680 ) ) ;
#6885 = ORIENTED_EDGE ( 'NONE', *, *, #8610, .F. ) ;
#6886 = CARTESIAN_POINT ( 'NONE',  ( 30.59138290137888916, -95.58039132682486638, -66.10404757334158887 ) ) ;
#6887 = FACE_OUTER_BOUND ( 'NONE', #27848, .T. ) ;
#6888 = CARTESIAN_POINT ( 'NONE',  ( -25.21435515916025594, 1.749597353048488237E-16, -4.373993382621220594E-17 ) ) ;
#6889 = CARTESIAN_POINT ( 'NONE',  ( 55.49584447822657296, 7.317474139115629939, 72.18163437663943682 ) ) ;
#6890 = ORIENTED_EDGE ( 'NONE', *, *, #10926, .F. ) ;
#6891 = EDGE_CURVE ( 'NONE', #5205, #5134, #21374, .T. ) ;
#6892 = ORIENTED_EDGE ( 'NONE', *, *, #6252, .T. ) ;
#6893 = ORIENTED_EDGE ( 'NONE', *, *, #1278, .T. ) ;
#6894 = DIRECTION ( 'NONE',  ( -1.000000000000000000, -0.000000000000000000, -0.000000000000000000 ) ) ;
#6895 = B_SPLINE_CURVE_WITH_KNOTS ( 'NONE', 3,
 ( #23359, #741, #25216, #3054, #18876, #3334, #10110, #9972 ),
 .UNSPECIFIED., .F., .F.,
 ( 4, 2, 2, 4 ),
 ( 3.469446951953614189E-18, 0.0002429592666046710139, 0.0004859185332093385584, 0.0009718370664186956566 ),
 .UNSPECIFIED. ) ;
#6896 = CARTESIAN_POINT ( 'NONE',  ( 28.37603512858441590, 45.02094145483519583, -105.5302493666422379 ) ) ;
#6897 = CARTESIAN_POINT ( 'NONE',  ( -20.20700224038492010, -18.19058640100240254, -23.35150625415651859 ) ) ;
#6898 = CARTESIAN_POINT ( 'NONE',  ( -25.21435515916025594, 1.749597353048488237E-16, -4.373993382621220594E-17 ) ) ;
#6899 = DIRECTION ( 'NONE',  ( 0.5946245182733607137, 0.7870422510449666120, -0.1642747008466166614 ) ) ;
#6900 = CARTESIAN_POINT ( 'NONE',  ( 5.340103556456712752, 128.8311297043957495, -71.72120378849476197 ) ) ;
#6901 =( BOUNDED_SURFACE ( )  B_SPLINE_SURFACE ( 3, 1, ( 
 ( #26646, #22646 ),
 ( #2918, #24518 ),
 ( #4786, #4925 ),
 ( #23611, #16842 ) ),
 .UNSPECIFIED., .F., .F., .F. ) 
 B_SPLINE_SURFACE_WITH_KNOTS ( ( 4, 4 ),
 ( 2, 2 ),
 ( 0.000000000000000000, 1.000000000000000000 ),
 ( 0.000000000000000000, 1.000000000000000000 ),
 .UNSPECIFIED. ) 
 GEOMETRIC_REPRESENTATION_ITEM ( )  RATIONAL_B_SPLINE_SURFACE ( (
 ( 1.000000000000000000, 1.000000000000000000),
 ( 0.6386103224230302855, 0.9954351624131538845),
 ( 0.6386103224230302855, 0.9954351624131538845),
 ( 1.000000000000000000, 1.000000000000000000) ) ) 
 REPRESENTATION_ITEM ( '' )  SURFACE ( )  );
#6902 = CARTESIAN_POINT ( 'NONE',  ( 26.11404676487257603, -112.7148551500681037, 10.71016160607530310 ) ) ;
#6903 = EDGE_CURVE ( 'NONE', #17826, #26336, #2813, .T. ) ;
#6904 = ORIENTED_EDGE ( 'NONE', *, *, #14456, .T. ) ;
#6905 = CARTESIAN_POINT ( 'NONE',  ( 26.11404676487257603, -33.91085499298301897, -108.0249973236470993 ) ) ;
#6906 = CARTESIAN_POINT ( 'NONE',  ( -9.156249394959713683, -53.90509764945124971, 8.027840202794504165 ) ) ;
#6907 = CARTESIAN_POINT ( 'NONE',  ( -20.57838717382308147, 23.26537097894132344, 18.89542499756474569 ) ) ;
#6908 = CARTESIAN_POINT ( 'NONE',  ( 1.832998868059858122, -73.01698022778447239, 125.4013017422228558 ) ) ;
#6909 = EDGE_CURVE ( 'NONE', #4019, #20724, #13668, .T. ) ;
#6910 = CARTESIAN_POINT ( 'NONE',  ( 109.1624594426973118, 0.009754804742280794722, 0.01263706729759561664 ) ) ;
#6911 = VERTEX_POINT ( 'NONE', #17977 ) ;
#6913 = CARTESIAN_POINT ( 'NONE',  ( 109.1586059443104944, -0.003930911098393256690, -0.005881369279875392833 ) ) ;
#6912 = B_SPLINE_CURVE_WITH_KNOTS ( 'NONE', 3,
 ( #25995, #1663, #3543, #3971, #10465, #1385 ),
 .UNSPECIFIED., .F., .F.,
 ( 4, 2, 4 ),
 ( 2.168404344971008868E-19, 0.0006311571484586053554, 0.001262314296917210494 ),
 .UNSPECIFIED. ) ;
#6914 = B_SPLINE_CURVE_WITH_KNOTS ( 'NONE', 3,
 ( #5549, #9881, #14035, #25278, #11748, #11884, #22847, #18343, #18647, #13745 ),
 .UNSPECIFIED., .F., .F.,
 ( 4, 2, 2, 2, 4 ),
 ( 2.947001115474787729E-16, 0.0003346187017559134843, 0.0006692374035115322825, 0.001003856105267151135, 0.001338474807022769879 ),
 .UNSPECIFIED. ) ;
#6915 = CARTESIAN_POINT ( 'NONE',  ( 55.49584447822657296, 0.2676470673966822589, -72.55110015779771970 ) ) ;
#6916 = CARTESIAN_POINT ( 'NONE',  ( -55.24198130335446422, 0.004276389980776598189, 0.008252882783650057619 ) ) ;
#6917 = EDGE_LOOP ( 'NONE', ( #18003, #18477, #22789, #19958 ) ) ;
#6918 = VERTEX_POINT ( 'NONE', #6502 ) ;
#6919 = ORIENTED_EDGE ( 'NONE', *, *, #9809, .F. ) ;
#6920 = CARTESIAN_POINT ( 'NONE',  ( 109.1592201516379674, -0.002134489919768192863, 0.007566779963325561721 ) ) ;
#6921 = LINE ( 'NONE', #9642, #27139 ) ;
#6922 = CARTESIAN_POINT ( 'NONE',  ( 25.81918753295381208, 57.31966094783204113, 97.41320410180104261 ) ) ;
#6923 = VECTOR ( 'NONE', #22149, 1000.000000000000114 ) ;
#6924 = VERTEX_POINT ( 'NONE', #4462 ) ;
#6925 = CARTESIAN_POINT ( 'NONE',  ( -55.25719721206881729, 0.0006290797159209853082, -0.01115102788683027674 ) ) ;
#6926 = CARTESIAN_POINT ( 'NONE',  ( -4.780792508754329262, 45.80716263181262349, 18.84172549606824987 ) ) ;
#6927 = VERTEX_POINT ( 'NONE', #3 ) ;
#6928 = EDGE_CURVE ( 'NONE', #21439, #20282, #17837, .T. ) ;
#6929 = DIRECTION ( 'NONE',  ( -1.000000000000000000, 6.938893903907226837E-18, -1.734723475976806709E-18 ) ) ;
#6930 = ORIENTED_EDGE ( 'NONE', *, *, #18094, .T. ) ;
#6931 = DIRECTION ( 'NONE',  ( 0.000000000000000000, 0.000000000000000000, 1.000000000000000000 ) ) ;
#6932 = EDGE_CURVE ( 'NONE', #9180, #10634, #27904, .T. ) ;
#6933 = CARTESIAN_POINT ( 'NONE',  ( -1.323439229708146536, 43.04565903621286083, -16.42345129173351381 ) ) ;
#6934 = CARTESIAN_POINT ( 'NONE',  ( -4.780792508754322157, 49.38761389561003767, 3.764354093953751423 ) ) ;
#6935 = CARTESIAN_POINT ( 'NONE',  ( -55.25719721206881729, -0.01115102788683311301, 0.0006290797159230496292 ) ) ;
#6936 = CARTESIAN_POINT ( 'NONE',  ( 109.1589550718174877, 0.006445391216542572903, 0.003980125429499906282 ) ) ;
#6937 = CARTESIAN_POINT ( 'NONE',  ( 16.05277956358206382, -75.66118899150433208, -121.7045645913025282 ) ) ;
#6938 = CARTESIAN_POINT ( 'NONE',  ( 2.430230287190592531, -46.34481016236730255, -137.9371479820467243 ) ) ;
#6939 = CARTESIAN_POINT ( 'NONE',  ( 25.64681081121879203, 110.5293738517611501, -23.06870491922213873 ) ) ;
#6940 = CARTESIAN_POINT ( 'NONE',  ( -55.24390624410018802, 0.009209468562452933355, 0.004896917417131438528 ) ) ;
#6941 =( BOUNDED_SURFACE ( )  B_SPLINE_SURFACE ( 3, 1, ( 
 ( #5342, #3051 ),
 ( #18434, #11682 ),
 ( #7522, #13975 ),
 ( #11828, #7233 ) ),
 .UNSPECIFIED., .F., .F., .F. ) 
 B_SPLINE_SURFACE_WITH_KNOTS ( ( 4, 4 ),
 ( 2, 2 ),
 ( 0.000000000000000000, 1.000000000000000000 ),
 ( 0.000000000000000000, 1.000000000000000000 ),
 .UNSPECIFIED. ) 
 GEOMETRIC_REPRESENTATION_ITEM ( )  RATIONAL_B_SPLINE_SURFACE ( (
 ( 1.000000000000000000, 1.000000000000000000),
 ( 0.6386103224230302855, 0.9954351624131538845),
 ( 0.6386103224230302855, 0.9954351624131538845),
 ( 1.000000000000000000, 1.000000000000000000) ) ) 
 REPRESENTATION_ITEM ( '' )  SURFACE ( )  );
#6942 = ADVANCED_FACE ( 'NONE', ( #17558 ), #19501, .F. ) ;
#6943 = CARTESIAN_POINT ( 'NONE',  ( -8.786685647604890903, -48.22796981442753150, 23.24040270374441874 ) ) ;
#6944 = B_SPLINE_CURVE_WITH_KNOTS ( 'NONE', 3,
 ( #13427, #6981, #13011, #22227 ),
 .UNSPECIFIED., .F., .F.,
 ( 4, 4 ),
 ( 0.000000000000000000, 0.01077107196513893764 ),
 .UNSPECIFIED. ) ;
#6945 = CARTESIAN_POINT ( 'NONE',  ( -1.031422197589716205, -1.530725436377144755, 45.78027046666445443 ) ) ;
#6946 = DIRECTION ( 'NONE',  ( 0.000000000000000000, 5.223019709708233256E-21, -1.000000000000000000 ) ) ;
#6947 = CARTESIAN_POINT ( 'NONE',  ( -40.00000000000000000, 0.000000000000000000, -80.00000000000000000 ) ) ;
#6948 = EDGE_CURVE ( 'NONE', #21998, #18571, #16220, .T. ) ;
#6949 = VERTEX_POINT ( 'NONE', #4606 ) ;
#6950 = ORIENTED_EDGE ( 'NONE', *, *, #24485, .T. ) ;
#6951 = CARTESIAN_POINT ( 'NONE',  ( -24.53237795827026346, 24.99972053297905461, -22.94498492516348520 ) ) ;
#6952 = VECTOR ( 'NONE', #21345, 1000.000000000000000 ) ;
#6953 = CARTESIAN_POINT ( 'NONE',  ( -55.25297051322618813, 0.01093108995495213273, 0.01019003092403696770 ) ) ;
#6954 = ORIENTED_EDGE ( 'NONE', *, *, #24378, .T. ) ;
#6955 = VECTOR ( 'NONE', #18957, 1000.000000000000114 ) ;
#6956 = ORIENTED_EDGE ( 'NONE', *, *, #1604, .F. ) ;
#6957 = ORIENTED_EDGE ( 'NONE', *, *, #22788, .T. ) ;
#6958 = VECTOR ( 'NONE', #2840, 1000.000000000000227 ) ;
#6959 = CARTESIAN_POINT ( 'NONE',  ( -20.20612092514785019, 29.57813644637190365, -1.137292630518160097 ) ) ;
#6960 = CARTESIAN_POINT ( 'NONE',  ( 109.1587776205901861, 0.003592288931003351140, -0.006388631651935905084 ) ) ;
#6961 = EDGE_LOOP ( 'NONE', ( #8878, #22559, #3854, #26484 ) ) ;
#6962 = CARTESIAN_POINT ( 'NONE',  ( 26.11404676487257603, -98.61392875273325842, -55.62948129436350087 ) ) ;
#6963 = CARTESIAN_POINT ( 'NONE',  ( 25.98107933586751273, -107.2544904356366402, -35.99661810150961827 ) ) ;
#6964 = CARTESIAN_POINT ( 'NONE',  ( -20.47566262905009893, -28.85746289809572218, 7.708089517695493775 ) ) ;
#6965 = CARTESIAN_POINT ( 'NONE',  ( 25.64681081121880624, 66.03065707438935306, 91.59071981940594753 ) ) ;
#6966 = VECTOR ( 'NONE', #15039, 999.9999999999998863 ) ;
#6967 = CARTESIAN_POINT ( 'NONE',  ( 28.37644542392844471, 4.054996728115944471, -124.2737818798214136 ) ) ;
#6968 = EDGE_CURVE ( 'NONE', #5199, #26221, #26941, .T. ) ;
#6969 = CONICAL_SURFACE ( 'NONE', #10644, 117.6351876552689504, 0.9945805576725580410 ) ;
#6970 = CARTESIAN_POINT ( 'NONE',  ( -1.539760825549692180, 11.93465943778514315, -44.72358953107736568 ) ) ;
#6971 = CARTESIAN_POINT ( 'NONE',  ( 109.1778270068192853, -0.001322180554001336399, -0.009220257877180839182 ) ) ;
#6972 = FACE_OUTER_BOUND ( 'NONE', #22679, .T. ) ;
#6973 = CONICAL_SURFACE ( 'NONE', #8814, 117.6351876552689504, 0.9945805576725580410 ) ;
#6975 = ORIENTED_EDGE ( 'NONE', *, *, #20765, .F. ) ;
#6974 = EDGE_CURVE ( 'NONE', #12695, #22316, #7386, .T. ) ;
#6977 = CARTESIAN_POINT ( 'NONE',  ( -8.259864102781671491, -52.06232470801718648, -9.986657004933428894 ) ) ;
#6976 = CARTESIAN_POINT ( 'NONE',  ( -1.031422197589711764, 1.530725436377463389, -45.78027046666443312 ) ) ;
#6978 = CARTESIAN_POINT ( 'NONE',  ( 32.73300124599732186, 0.000000000000000000, 0.000000000000000000 ) ) ;
#6979 = CARTESIAN_POINT ( 'NONE',  ( 30.59141879584286627, -79.74795589902086590, 84.53180090073648500 ) ) ;
#6980 = CARTESIAN_POINT ( 'NONE',  ( 109.1586900883932856, -0.005236795036860577776, 0.004851151255037344269 ) ) ;
#6981 = CARTESIAN_POINT ( 'NONE',  ( 8.186469829614468452, 148.8557359502364932, -12.15801983495463467 ) ) ;
#6982 = ORIENTED_EDGE ( 'NONE', *, *, #5325, .F. ) ;
#6983 = CARTESIAN_POINT ( 'NONE',  ( -28.13707043255157103, -18.96624908365855688, -12.83104814250447134 ) ) ;
#6984 = ORIENTED_EDGE ( 'NONE', *, *, #4913, .F. ) ;
#6985 = CARTESIAN_POINT ( 'NONE',  ( 25.65782528836482612, 103.3897864210302373, -45.39960327191509037 ) ) ;
#6986 = DIRECTION ( 'NONE',  ( 0.000000000000000000, 0.000000000000000000, 1.000000000000000000 ) ) ;
#6987 = ORIENTED_EDGE ( 'NONE', *, *, #2518, .T. ) ;
#6988 = ORIENTED_EDGE ( 'NONE', *, *, #17276, .T. ) ;
#6989 = B_SPLINE_CURVE_WITH_KNOTS ( 'NONE', 3,
 ( #10290, #27533, #27386, #27677 ),
 .UNSPECIFIED., .F., .F.,
 ( 4, 4 ),
 ( 2.619375006920453660E-16, 0.008383748772659739903 ),
 .UNSPECIFIED. ) ;
#6990 = CARTESIAN_POINT ( 'NONE',  ( 0.000000000000000000, 0.000000000000000000, 0.000000000000000000 ) ) ;
#6991 = VERTEX_POINT ( 'NONE', #2442 ) ;
#6992 = CARTESIAN_POINT ( 'NONE',  ( 1.833603222531958954, -96.76619886578252761, -108.1346772638456457 ) ) ;
#6993 = VERTEX_POINT ( 'NONE', #13375 ) ;
#6994 =( BOUNDED_SURFACE ( )  B_SPLINE_SURFACE ( 3, 1, ( 
 ( #1174, #9822 ),
 ( #18590, #16430 ),
 ( #25214, #14248 ),
 ( #23070, #14406 ) ),
 .UNSPECIFIED., .F., .F., .F. ) 
 B_SPLINE_SURFACE_WITH_KNOTS ( ( 4, 4 ),
 ( 2, 2 ),
 ( 0.000000000000000000, 1.000000000000000000 ),
 ( 0.000000000000000000, 1.000000000000000000 ),
 .UNSPECIFIED. ) 
 GEOMETRIC_REPRESENTATION_ITEM ( )  RATIONAL_B_SPLINE_SURFACE ( (
 ( 1.000000000000000000, 1.000000000000000000),
 ( 0.9956975270656954757, 0.8568959468854893125),
 ( 0.9956975270656954757, 0.8568959468854893125),
 ( 1.000000000000000000, 1.000000000000000000) ) ) 
 REPRESENTATION_ITEM ( '' )  SURFACE ( )  );
#6995 = CARTESIAN_POINT ( 'NONE',  ( 2.430230287190581429, -138.8342928068223046, 43.58368230469343985 ) ) ;
#6996 = AXIS2_PLACEMENT_3D ( 'NONE', #22031, #15254, #6931 ) ;
#6997 = CARTESIAN_POINT ( 'NONE',  ( -21.81686047589426281, -18.24499610240063419, -33.92779429964196680 ) ) ;
#6998 = CARTESIAN_POINT ( 'NONE',  ( -55.24390624410018802, -0.01032895241566962087, 0.001451500391950532459 ) ) ;
#6999 = CARTESIAN_POINT ( 'NONE',  ( -2.911734481061388102, 46.11606034418780098, 12.03743348210733011 ) ) ;
#7000 = CARTESIAN_POINT ( 'NONE',  ( -20.57838717382308147, 1.611677988432361097, -29.92853265176831812 ) ) ;
#7001 = CARTESIAN_POINT ( 'NONE',  ( -1.031422197589711764, -25.67058493451469303, -37.93675465142463565 ) ) ;
#7002 = ADVANCED_FACE ( 'NONE', ( #22326 ), #22459, .F. ) ;
#7003 = CARTESIAN_POINT ( 'NONE',  ( 55.49584447822657296, -62.96491934286019188, 36.04376091928521220 ) ) ;
#7004 = CARTESIAN_POINT ( 'NONE',  ( 2.430230287190592531, -28.83279105684524168, 142.6294793592097108 ) ) ;
#7005 = CARTESIAN_POINT ( 'NONE',  ( -1.464342487929859660, -2.431462367721655138, -46.14921266389555399 ) ) ;
#7006 = EDGE_CURVE ( 'NONE', #12820, #20942, #7220, .T. ) ;
#7007 = VERTEX_POINT ( 'NONE', #18132 ) ;
#7008 = CARTESIAN_POINT ( 'NONE',  ( 2.063896406836605024, 144.6078654718903636, -13.84738934186042059 ) ) ;
#7009 = CARTESIAN_POINT ( 'NONE',  ( 2.433796855181219243, -144.5536872373193376, 16.65276281464516828 ) ) ;
#7010 = EDGE_CURVE ( 'NONE', #18831, #5021, #18381, .T. ) ;
#7011 = CARTESIAN_POINT ( 'NONE',  ( -8.786685647604890903, -53.04920435127188938, -7.199674155858766689 ) ) ;
#7012 = CARTESIAN_POINT ( 'NONE',  ( -20.20700224038492010, -8.199606986804138131, 28.44216453106544762 ) ) ;
#7013 = VECTOR ( 'NONE', #26766, 1000.000000000000114 ) ;
#7014 = CARTESIAN_POINT ( 'NONE',  ( -20.57838717382308147, -28.96176188950213870, 7.715628353033985753 ) ) ;
#7015 = VECTOR ( 'NONE', #4429, 1000.000000000000000 ) ;
#7016 = CARTESIAN_POINT ( 'NONE',  ( -1.259920593601974392, 45.95412615877143026, 2.243284667987943681 ) ) ;
#7017 = CARTESIAN_POINT ( 'NONE',  ( 26.11404676487257603, 112.4785329405482059, 12.95861723607491456 ) ) ;
#7018 = ORIENTED_EDGE ( 'NONE', *, *, #17194, .F. ) ;
#7019 = CARTESIAN_POINT ( 'NONE',  ( -24.53237795827023859, -33.71192251888856362, 3.868415699416008380 ) ) ;
#7020 = ORIENTED_EDGE ( 'NONE', *, *, #13131, .F. ) ;
#7022 = ADVANCED_FACE ( 'NONE', ( #3172 ), #7587, .F. ) ;
#7021 = CARTESIAN_POINT ( 'NONE',  ( -4.473127245936434626, -12.17046501147483895, 47.80062405537812964 ) ) ;
#7023 =( BOUNDED_SURFACE ( )  B_SPLINE_SURFACE ( 3, 1, ( 
 ( #770, #27091 ),
 ( #27240, #14004 ),
 ( #14138, #26820 ),
 ( #16021, #20342 ) ),
 .UNSPECIFIED., .F., .F., .F. ) 
 B_SPLINE_SURFACE_WITH_KNOTS ( ( 4, 4 ),
 ( 2, 2 ),
 ( 0.000000000000000000, 1.000000000000000000 ),
 ( 0.000000000000000000, 1.000000000000000000 ),
 .UNSPECIFIED. ) 
 GEOMETRIC_REPRESENTATION_ITEM ( )  RATIONAL_B_SPLINE_SURFACE ( (
 ( 1.000000000000000000, 1.000000000000000000),
 ( 0.9934239774497837239, 0.8357310067453919133),
 ( 0.9934239774497837239, 0.8357310067453919133),
 ( 1.000000000000000000, 1.000000000000000000) ) ) 
 REPRESENTATION_ITEM ( '' )  SURFACE ( )  );
#7024 = VERTEX_POINT ( 'NONE', #7656 ) ;
#7025 = CARTESIAN_POINT ( 'NONE',  ( 2.433796855181219243, 133.5135467655526043, -57.85512797797757401 ) ) ;
#7026 = B_SPLINE_CURVE_WITH_KNOTS ( 'NONE', 3,
 ( #28415, #19785, #6567, #8716, #26413, #28142 ),
 .UNSPECIFIED., .F., .F.,
 ( 4, 2, 4 ),
 ( 6.952433221959954168E-18, 0.0006311571484586013438, 0.001262314296917195749 ),
 .UNSPECIFIED. ) ;
#7027 = ORIENTED_EDGE ( 'NONE', *, *, #5570, .F. ) ;
#7028 = B_SPLINE_CURVE_WITH_KNOTS ( 'NONE', 3,
 ( #22548, #8420, #12579, #10022, #28117, #3810, #5702, #27851, #8017, #14742 ),
 .UNSPECIFIED., .F., .F.,
 ( 4, 2, 2, 2, 4 ),
 ( 0.000000000000000000, 0.0003346267210630921333, 0.0006692534421261842666, 0.001003880163189276292, 0.001338506884252368533 ),
 .UNSPECIFIED. ) ;
#7029 = AXIS2_PLACEMENT_3D ( 'NONE', #7622, #5438, #3285 ) ;
#7030 = EDGE_CURVE ( 'NONE', #27786, #1490, #4979, .T. ) ;
#7031 = LINE ( 'NONE', #26576, #21643 ) ;
#7032 = CARTESIAN_POINT ( 'NONE',  ( -20.20700224038492010, -0.9908225410476447781, 29.58392382092673500 ) ) ;
#7033 = AXIS2_PLACEMENT_3D ( 'NONE', #22265, #7294, #16058 ) ;
#7034 = CARTESIAN_POINT ( 'NONE',  ( 25.64708010899964208, 107.3680906278376881, -34.94352788466177628 ) ) ;
#7035 = CARTESIAN_POINT ( 'NONE',  ( 25.98552792386799837, 107.9280603639527101, 33.93357582585531418 ) ) ;
#7036 = CARTESIAN_POINT ( 'NONE',  ( -1.239374126674604337, -25.08410696974215170, 38.61989855450968179 ) ) ;
#7037 = CARTESIAN_POINT ( 'NONE',  ( -20.57838717382308147, -1.611677988432568709, -29.92853265176830746 ) ) ;
#7038 = EDGE_CURVE ( 'NONE', #7707, #22719, #13958, .T. ) ;
#7039 = VERTEX_POINT ( 'NONE', #14390 ) ;
#7040 = CARTESIAN_POINT ( 'NONE',  ( -20.57838717382308147, 1.611677988432361097, -29.92853265176831812 ) ) ;
#7041 = CARTESIAN_POINT ( 'NONE',  ( -1.019300379054419947, -44.15350047934390432, 12.21833869579511500 ) ) ;
#7042 = CARTESIAN_POINT ( 'NONE',  ( -1.031422197589716205, -44.01264471863839134, 12.69107518035547955 ) ) ;
#7043 = ORIENTED_EDGE ( 'NONE', *, *, #428, .F. ) ;
#7044 = B_SPLINE_CURVE_WITH_KNOTS ( 'NONE', 3,
 ( #24051, #2130, #11212, #17813 ),
 .UNSPECIFIED., .F., .F.,
 ( 4, 4 ),
 ( 7.152448122690996019E-18, 0.008383560773332731156 ),
 .UNSPECIFIED. ) ;
#7045 = ORIENTED_EDGE ( 'NONE', *, *, #13372, .F. ) ;
#7046 = CARTESIAN_POINT ( 'NONE',  ( 1.833485406944043827, 73.01664920992966756, 125.4007332306548221 ) ) ;
#7047 = CARTESIAN_POINT ( 'NONE',  ( -1.583189561560252701, -38.94740041318275559, 25.21827308671274182 ) ) ;
#7048 = CARTESIAN_POINT ( 'NONE',  ( 55.49584447822657296, -36.50733923851154117, -62.69727227546439963 ) ) ;
#7049 = DIRECTION ( 'NONE',  ( 0.000000000000000000, 5.223019709707975211E-21, -1.000000000000000000 ) ) ;
#7050 = DIRECTION ( 'NONE',  ( 0.7563875759206388771, 0.6104009704506959677, 0.2351350468682803785 ) ) ;
#7051 = CARTESIAN_POINT ( 'NONE',  ( -4.162674018437154899, -48.79210541969629844, -3.424137510344775759 ) ) ;
#7052 = CARTESIAN_POINT ( 'NONE',  ( -22.34422965417124374, 26.20925041532892763, 27.39717383755251490 ) ) ;
#7053 = AXIS2_PLACEMENT_3D ( 'NONE', #12977, #21768, #19185 ) ;
#7054 = VERTEX_POINT ( 'NONE', #5472 ) ;
#7055 = CARTESIAN_POINT ( 'NONE',  ( 5.340103579038239623, -144.6887562507422729, -28.39990973304617583 ) ) ;
#7056 = CARTESIAN_POINT ( 'NONE',  ( 109.1587776205901577, -0.007297420966928602065, 0.0006832286435102221311 ) ) ;
#7057 = CARTESIAN_POINT ( 'NONE',  ( 25.64700659047694487, -0.2275682798794833872, 112.9110011064639565 ) ) ;
#7058 = CARTESIAN_POINT ( 'NONE',  ( -55.24271866751342941, 0.004256484107793641683, 0.008488649505346114801 ) ) ;
#7059 = CARTESIAN_POINT ( 'NONE',  ( 6.224689322667630975, 76.23997225729445404, -126.9212313063836461 ) ) ;
#7060 = ORIENTED_EDGE ( 'NONE', *, *, #27, .T. ) ;
#7061 = CARTESIAN_POINT ( 'NONE',  ( 109.1586900883932856, -0.004113747440992365084, 0.005833932871491302741 ) ) ;
#7062 = VECTOR ( 'NONE', #9796, 1000.000000000000227 ) ;
#7063 = CIRCLE ( 'NONE', #1975, 117.6351876552689504 ) ;
#7064 = CARTESIAN_POINT ( 'NONE',  ( 32.73300124599732186, 0.000000000000000000, 0.000000000000000000 ) ) ;
#7065 = CARTESIAN_POINT ( 'NONE',  ( 1.833691583653551227, -117.1866391460179813, -85.58103979054610022 ) ) ;
#7066 = VERTEX_POINT ( 'NONE', #15975 ) ;
#7067 = ORIENTED_EDGE ( 'NONE', *, *, #28102, .T. ) ;
#7068 = VERTEX_POINT ( 'NONE', #23054 ) ;
#7069 = CARTESIAN_POINT ( 'NONE',  ( -1.031422197589716205, 45.78027046666444733, -1.530725436377611715 ) ) ;
#7070 = DIRECTION ( 'NONE',  ( 0.000000000000000000, -5.223019709708233256E-21, 1.000000000000000000 ) ) ;
#7071 = EDGE_CURVE ( 'NONE', #25105, #8696, #25025, .T. ) ;
#7072 = CARTESIAN_POINT ( 'NONE',  ( 25.98552792386800903, 57.50018541500425329, 97.43552975939633143 ) ) ;
#7073 = EDGE_CURVE ( 'NONE', #27143, #17730, #28319, .T. ) ;
#7074 = CARTESIAN_POINT ( 'NONE',  ( 2.433796855181205476, 126.7346379669265843, -71.49415740224942795 ) ) ;
#7075 = ORIENTED_EDGE ( 'NONE', *, *, #5496, .F. ) ;
#7076 = CARTESIAN_POINT ( 'NONE',  ( 28.43349137099832902, 105.5221910860626764, -65.60227321965477643 ) ) ;
#7077 = CARTESIAN_POINT ( 'NONE',  ( 25.81918753295377655, 45.11728622333284733, -103.6306245682010712 ) ) ;
#7078 =( BOUNDED_SURFACE ( )  B_SPLINE_SURFACE ( 3, 1, ( 
 ( #8859, #25486 ),
 ( #26403, #18989 ),
 ( #7931, #68 ),
 ( #8565, #11012 ) ),
 .UNSPECIFIED., .F., .F., .F. ) 
 B_SPLINE_SURFACE_WITH_KNOTS ( ( 4, 4 ),
 ( 2, 2 ),
 ( 0.000000000000000000, 1.000000000000000000 ),
 ( 0.000000000000000000, 1.000000000000000000 ),
 .UNSPECIFIED. ) 
 GEOMETRIC_REPRESENTATION_ITEM ( )  RATIONAL_B_SPLINE_SURFACE ( (
 ( 1.000000000000000000, 1.000000000000000000),
 ( 0.6386103224230316178, 0.9954351624131538845),
 ( 0.6386103224230316178, 0.9954351624131538845),
 ( 1.000000000000000000, 1.000000000000000000) ) ) 
 REPRESENTATION_ITEM ( '' )  SURFACE ( )  );
#7079 = CARTESIAN_POINT ( 'NONE',  ( -1.050230347699842692, 1.897926697972695375E-16, 45.79907861674080749 ) ) ;
#7080 = ORIENTED_EDGE ( 'NONE', *, *, #6671, .F. ) ;
#7081 = CARTESIAN_POINT ( 'NONE',  ( -8.786685647604885574, 6.096987947571466530E-17, -1.524246986892866633E-17 ) ) ;
#7082 = ORIENTED_EDGE ( 'NONE', *, *, #26677, .F. ) ;
#7083 = CARTESIAN_POINT ( 'NONE',  ( 1.833206308920082073, 30.89799439741820564, -141.7818018507499289 ) ) ;
#7084 = CARTESIAN_POINT ( 'NONE',  ( 25.64681081121879203, -112.3352186517029878, -11.38886654529789233 ) ) ;
#7085 = CARTESIAN_POINT ( 'NONE',  ( -20.57838717382308147, 28.96176188950229502, 7.715628353033378239 ) ) ;
#7086 = CARTESIAN_POINT ( 'NONE',  ( -1.048996300304495310, 14.87787369922229708, 43.31387123529964356 ) ) ;
#7087 = CARTESIAN_POINT ( 'NONE',  ( 30.59138290137918403, 105.0379801549016463, -49.72302320601711756 ) ) ;
#7088 = CARTESIAN_POINT ( 'NONE',  ( -18.41936578851712625, -30.66520733838672186, -29.33493038358061966 ) ) ;
#7089 = B_SPLINE_CURVE_WITH_KNOTS ( 'NONE', 3,
 ( #18138, #9228, #17986, #7086, #15846, #24653, #3747, #3891, #1167, #16421, #3597, #27493, #12107 ),
 .UNSPECIFIED., .F., .F.,
 ( 4, 3, 3, 3, 4 ),
 ( 1.868354362588067661E-17, 0.0007657099931970537312, 0.001531419946797914168, 0.002296279302920151665, 0.003061450627205758099 ),
 .UNSPECIFIED. ) ;
#7090 = B_SPLINE_CURVE_WITH_KNOTS ( 'NONE', 3,
 ( #16180, #11726, #3230, #7142, #18631, #7274, #15902 ),
 .UNSPECIFIED., .F., .F.,
 ( 4, 3, 4 ),
 ( 0.000000000000000000, 0.02398743853561347006, 0.04000277880656215312 ),
 .UNSPECIFIED. ) ;
#7091 = CARTESIAN_POINT ( 'NONE',  ( 5.340103556456526235, 17.70136535450102500, -146.3832391989194548 ) ) ;
#7092 = CARTESIAN_POINT ( 'NONE',  ( 1.832998868059858122, 107.4798986104860177, 97.49378069860833307 ) ) ;
#7093 = EDGE_CURVE ( 'NONE', #27430, #16711, #19064, .T. ) ;
#7094 = CARTESIAN_POINT ( 'NONE',  ( 2.433796855181233454, 125.2830755159764777, -74.00833731765430912 ) ) ;
#7095 = DIRECTION ( 'NONE',  ( 1.000000000000000000, -6.938893903907226837E-18, 1.734723475976806709E-18 ) ) ;
#7096 = EDGE_LOOP ( 'NONE', ( #1395, #6405, #18046, #26539 ) ) ;
#7097 = ORIENTED_EDGE ( 'NONE', *, *, #348, .F. ) ;
#7098 = CARTESIAN_POINT ( 'NONE',  ( 2.263178113027020544, -126.6115605262343422, 71.48082833565020167 ) ) ;
#7099 = CARTESIAN_POINT ( 'NONE',  ( 5.340103556456450740, 71.72120378849609779, 128.8311297043948116 ) ) ;
#7100 = ORIENTED_EDGE ( 'NONE', *, *, #25818, .F. ) ;
#7101 = EDGE_LOOP ( 'NONE', ( #8786, #20057, #11537, #14137 ) ) ;
#7102 = ORIENTED_EDGE ( 'NONE', *, *, #18486, .T. ) ;
#7103 = EDGE_CURVE ( 'NONE', #4802, #22173, #18063, .T. ) ;
#7104 = B_SPLINE_CURVE_WITH_KNOTS ( 'NONE', 3,
 ( #27382, #9546, #5509, #18752, #16304, #13995, #27233, #7547, #22663, #14131 ),
 .UNSPECIFIED., .F., .F.,
 ( 4, 2, 2, 2, 4 ),
 ( 8.673617379884035472E-19, 0.0003346267210630925128, 0.0006692534421261841582, 0.001003880163189275858, 0.001338506884252367449 ),
 .UNSPECIFIED. ) ;
#7105 = EDGE_CURVE ( 'NONE', #3326, #17470, #11666, .T. ) ;
#7106 = CARTESIAN_POINT ( 'NONE',  ( 109.1592201516379674, -0.007856029051018016685, -0.0003082430541935813001 ) ) ;
#7107 = CARTESIAN_POINT ( 'NONE',  ( 8.186469777910737378, 34.43598809570138997, 145.3272523831804790 ) ) ;
#7108 = EDGE_CURVE ( 'NONE', #2726, #21682, #24943, .T. ) ;
#7109 = CARTESIAN_POINT ( 'NONE',  ( 9.884929003653626367, -109.0134320167740043, 103.8128997986854074 ) ) ;
#7110 = EDGE_CURVE ( 'NONE', #19505, #21234, #9483, .T. ) ;
#7111 =( BOUNDED_SURFACE ( )  B_SPLINE_SURFACE ( 3, 1, ( 
 ( #1140, #18985 ),
 ( #18395, #14080 ),
 ( #27764, #8065 ),
 ( #9630, #27175 ) ),
 .UNSPECIFIED., .F., .F., .F. ) 
 B_SPLINE_SURFACE_WITH_KNOTS ( ( 4, 4 ),
 ( 2, 2 ),
 ( 0.000000000000000000, 1.000000000000000000 ),
 ( 0.000000000000000000, 1.000000000000000000 ),
 .UNSPECIFIED. ) 
 GEOMETRIC_REPRESENTATION_ITEM ( )  RATIONAL_B_SPLINE_SURFACE ( (
 ( 1.000000000000000000, 1.000000000000000000),
 ( 0.7789835883360578528, 0.9689951854195403280),
 ( 0.7789835883360578528, 0.9689951854195403280),
 ( 1.000000000000000000, 1.000000000000000000) ) ) 
 REPRESENTATION_ITEM ( '' )  SURFACE ( )  );
#7112 = CARTESIAN_POINT ( 'NONE',  ( -55.24271866751342941, -0.004256484107792932181, -0.008488649505346277865 ) ) ;
#7113 = CARTESIAN_POINT ( 'NONE',  ( -22.34422965417123663, -6.759368364654068095, 37.30738373203626423 ) ) ;
#7114 = CARTESIAN_POINT ( 'NONE',  ( 10.93730112725932635, 0.000000000000000000, 0.000000000000000000 ) ) ;
#7115 = CARTESIAN_POINT ( 'NONE',  ( 26.28373643307409324, 4.159810388346418364, 127.4927519498666726 ) ) ;
#7116 = CARTESIAN_POINT ( 'NONE',  ( 25.73574536432413495, 34.14219540448133472, 107.6875787074508537 ) ) ;
#7117 = DIRECTION ( 'NONE',  ( -0.5914120900931443270, 0.5335794202785305584, -0.6045864222316656988 ) ) ;
#7118 = DIRECTION ( 'NONE',  ( 0.8320502949607718746, 6.793118186493350437E-17, 0.5547001952908368061 ) ) ;
#7119 = CARTESIAN_POINT ( 'NONE',  ( -55.24728320129491266, -0.01402509393918509838, 0.003868537197316900683 ) ) ;
#7120 = CARTESIAN_POINT ( 'NONE',  ( -1.031422197589711764, 25.67058493451497725, 37.93675465142443670 ) ) ;
#7121 = ORIENTED_EDGE ( 'NONE', *, *, #17887, .F. ) ;
#7122 = CARTESIAN_POINT ( 'NONE',  ( -1.619063947482197729, -44.80407745103793360, -11.94059994246142331 ) ) ;
#7123 = CARTESIAN_POINT ( 'NONE',  ( 6.224689322667647851, -129.4863684118282379, -71.79702446228439783 ) ) ;
#7124 = LINE ( 'NONE', #5079, #13481 ) ;
#7125 = CARTESIAN_POINT ( 'NONE',  ( 109.1592201516379674, 0.006174480289199407029, -0.004867031887019566266 ) ) ;
#7126 = CARTESIAN_POINT ( 'NONE',  ( -4.162674018437137136, -11.82104147411594752, -47.46216648493552981 ) ) ;
#7127 = EDGE_LOOP ( 'NONE', ( #3740, #2675, #16315, #27134 ) ) ;
#7128 = FACE_OUTER_BOUND ( 'NONE', #24340, .T. ) ;
#7129 = ORIENTED_EDGE ( 'NONE', *, *, #16291, .T. ) ;
#7130 = DIRECTION ( 'NONE',  ( 0.000000000000000000, 5.223019709708233256E-21, -1.000000000000000000 ) ) ;
#7131 = CARTESIAN_POINT ( 'NONE',  ( 1.833838848569441238, -29.99593366454849175, 141.9757689770220281 ) ) ;
#7132 = ORIENTED_EDGE ( 'NONE', *, *, #18065, .T. ) ;
#7133 = CARTESIAN_POINT ( 'NONE',  ( 16.75465622695631751, 125.4242432475205220, -67.05928661304241700 ) ) ;
#7134 = ORIENTED_EDGE ( 'NONE', *, *, #21843, .F. ) ;
#7135 = CARTESIAN_POINT ( 'NONE',  ( 28.37603512858453669, 91.75440368550030712, -68.88140609180105400 ) ) ;
#7136 = ORIENTED_EDGE ( 'NONE', *, *, #10926, .T. ) ;
#7137 = EDGE_CURVE ( 'NONE', #27834, #9239, #12238, .T. ) ;
#7138 = EDGE_CURVE ( 'NONE', #27364, #24182, #6729, .T. ) ;
#7139 = ORIENTED_EDGE ( 'NONE', *, *, #18379, .F. ) ;
#7140 = CARTESIAN_POINT ( 'NONE',  ( 109.1592201516379674, 0.003476928926125392744, -0.007051465909551727154 ) ) ;
#7141 = EDGE_CURVE ( 'NONE', #13619, #28480, #17363, .T. ) ;
#7142 = CARTESIAN_POINT ( 'NONE',  ( 19.66333377628707169, -136.4524620437342719, -18.85786579350090619 ) ) ;
#7143 = B_SPLINE_CURVE_WITH_KNOTS ( 'NONE', 3,
 ( #23871, #3982, #24007, #23440, #21404, #12478, #17221, #21539 ),
 .UNSPECIFIED., .F., .F.,
 ( 4, 2, 2, 4 ),
 ( 0.000000000000000000, 0.0002429588503611217285, 0.0004859177007222434570, 0.0009718354014444869141 ),
 .UNSPECIFIED. ) ;
#7144 = DIRECTION ( 'NONE',  ( -1.000000000000000000, -0.000000000000000000, -0.000000000000000000 ) ) ;
#7145 = CARTESIAN_POINT ( 'NONE',  ( -2.911734481061406754, 44.38410240830302911, -17.36785190845994720 ) ) ;
#7146 = CARTESIAN_POINT ( 'NONE',  ( -5.986830583229477476, 11.27873876172141365, -49.46736940480261779 ) ) ;
#7147 = CARTESIAN_POINT ( 'NONE',  ( -1.019300379054419947, -25.26451264419671361, -38.21680004809154241 ) ) ;
#7148 = CARTESIAN_POINT ( 'NONE',  ( -1.045287976400383290, 12.68782741917383738, 44.00138577190627842 ) ) ;
#7149 = CARTESIAN_POINT ( 'NONE',  ( -1.045287976400362417, 25.66401692419989899, -37.92705037016767733 ) ) ;
#7150 = CARTESIAN_POINT ( 'NONE',  ( -25.21435515916043357, 31.17620025257608418, 15.02493970636113474 ) ) ;
#7151 = ORIENTED_EDGE ( 'NONE', *, *, #27690, .F. ) ;
#7152 = CARTESIAN_POINT ( 'NONE',  ( 25.64681081121879203, 23.88203588908081443, 110.3564950173082480 ) ) ;
#7153 = CARTESIAN_POINT ( 'NONE',  ( 26.11404676487257603, -84.89295829319543429, 74.91683232330944975 ) ) ;
#7154 = CARTESIAN_POINT ( 'NONE',  ( -22.34422965417125795, -37.57019010019543970, 5.100074259622997097 ) ) ;
#7155 = EDGE_LOOP ( 'NONE', ( #24596, #11197, #5459, #27394 ) ) ;
#7156 = CARTESIAN_POINT ( 'NONE',  ( -16.86833981943423311, 31.95666732167563850, -30.57013526701928186 ) ) ;
#7157 = CARTESIAN_POINT ( 'NONE',  ( -28.13707043255157103, 22.00298671236748760, 6.342158660426773231 ) ) ;
#7158 = CARTESIAN_POINT ( 'NONE',  ( 26.28373643307435614, 78.30371666786363960, 100.6987277884683323 ) ) ;
#7159 = ORIENTED_EDGE ( 'NONE', *, *, #8933, .F. ) ;
#7160 = CARTESIAN_POINT ( 'NONE',  ( 1.831572820252008738, -117.9752562883672482, 84.49389457294098804 ) ) ;
#7161 = ORIENTED_EDGE ( 'NONE', *, *, #27918, .T. ) ;
#7162 = B_SPLINE_CURVE_WITH_KNOTS ( 'NONE', 3,
 ( #11883, #14034, #2973, #4972 ),
 .UNSPECIFIED., .F., .F.,
 ( 4, 4 ),
 ( 2.212843619328882373E-16, 0.008383748772659684392 ),
 .UNSPECIFIED. ) ;
#7163 = CARTESIAN_POINT ( 'NONE',  ( 10.93730112725986281, -149.7554878793150408, 20.69552240458288850 ) ) ;
#7164 = CARTESIAN_POINT ( 'NONE',  ( -55.24728320129491266, -0.009072670231974808847, -0.01137345571546840607 ) ) ;
#7165 = EDGE_CURVE ( 'NONE', #19774, #2342, #11867, .T. ) ;
#7166 = ORIENTED_EDGE ( 'NONE', *, *, #20627, .F. ) ;
#7167 = CARTESIAN_POINT ( 'NONE',  ( 109.1721716018069515, -0.005466227998627365414, 0.01616973485710003489 ) ) ;
#7168 = ORIENTED_EDGE ( 'NONE', *, *, #20345, .F. ) ;
#7169 = EDGE_CURVE ( 'NONE', #19892, #28095, #5775, .T. ) ;
#7170 = CARTESIAN_POINT ( 'NONE',  ( 2.433796855181219243, -71.49415740225165905, 126.7346379669253622 ) ) ;
#7171 = ORIENTED_EDGE ( 'NONE', *, *, #8590, .T. ) ;
#7172 = EDGE_CURVE ( 'NONE', #26061, #24558, #16710, .T. ) ;
#7173 = CARTESIAN_POINT ( 'NONE',  ( 60.46576798286869803, 12.50000000000000000, 1.596046867330078713E-15 ) ) ;
#7174 = B_SPLINE_CURVE_WITH_KNOTS ( 'NONE', 3,
 ( #24650, #8950, #12965, #6790, #21760, #2024 ),
 .UNSPECIFIED., .F., .F.,
 ( 4, 2, 4 ),
 ( 0.000000000000000000, 0.003570751334075638293, 0.007141502668151268780 ),
 .UNSPECIFIED. ) ;
#7175 = CARTESIAN_POINT ( 'NONE',  ( 32.73300124599740002, -89.94078864464006529, -75.82012867748569818 ) ) ;
#7176 = CARTESIAN_POINT ( 'NONE',  ( 25.64692872815574631, -35.19724814977989524, 107.2850779876533238 ) ) ;
#7177 = DIRECTION ( 'NONE',  ( -0.5914120900931443270, -0.6476200150380216902, 0.4804373588864745970 ) ) ;
#7178 = CARTESIAN_POINT ( 'NONE',  ( -1.259920593601984162, 16.33409644610551581, -43.01175804832013938 ) ) ;
#7179 = CARTESIAN_POINT ( 'NONE',  ( -4.473127245936434626, 18.25038884639934977, 45.82513704981523972 ) ) ;
#7180 = ORIENTED_EDGE ( 'NONE', *, *, #23044, .F. ) ;
#7181 = CARTESIAN_POINT ( 'NONE',  ( 8.186469829614360094, -134.9918587494109659, -63.89871393833158919 ) ) ;
#7182 = CARTESIAN_POINT ( 'NONE',  ( 25.64681081121879203, 34.49579773461926635, -107.5125461021399218 ) ) ;
#7183 = CARTESIAN_POINT ( 'NONE',  ( 1.832998868059890096, 142.0492247521726199, -29.64765804469936583 ) ) ;
#7184 = EDGE_LOOP ( 'NONE', ( #1388, #3594, #16106, #7027 ) ) ;
#7185 = EDGE_LOOP ( 'NONE', ( #26847, #5542, #4546, #13344 ) ) ;
#7186 = ORIENTED_EDGE ( 'NONE', *, *, #3299, .T. ) ;
#7187 = CARTESIAN_POINT ( 'NONE',  ( -9.156249394959713683, -53.74753343182709386, -9.022661520477562647 ) ) ;
#7188 = CARTESIAN_POINT ( 'NONE',  ( 109.1586900883932856, 0.006231977675084991036, 0.003481399864218453783 ) ) ;
#7189 = CARTESIAN_POINT ( 'NONE',  ( -55.24728320129491266, -0.01214321324517104832, 0.008013189884951824049 ) ) ;
#7190 = CARTESIAN_POINT ( 'NONE',  ( -5.986830583229376224, -38.20088153919473939, 33.39046620690945844 ) ) ;
#7191 = CARTESIAN_POINT ( 'NONE',  ( -8.786685647604887350, 53.04920435127183254, -7.199674155859138835 ) ) ;
#7192 = CARTESIAN_POINT ( 'NONE',  ( 25.64699802086725811, -83.75009658924048495, 75.72889180797095321 ) ) ;
#7193 = CARTESIAN_POINT ( 'NONE',  ( 55.79472521941428198, 59.28412330436302113, 42.17269936297659427 ) ) ;
#7194 = ORIENTED_EDGE ( 'NONE', *, *, #2731, .F. ) ;
#7195 = CARTESIAN_POINT ( 'NONE',  ( -24.53237795827029899, -24.99972053297889119, 22.94498492516371613 ) ) ;
#7196 = CARTESIAN_POINT ( 'NONE',  ( -1.045287976400351981, -15.59869763335126436, -43.05558670614231431 ) ) ;
#7197 = CARTESIAN_POINT ( 'NONE',  ( 109.1589550718174877, -0.006826119083824097253, -0.003284595046925634348 ) ) ;
#7198 = CARTESIAN_POINT ( 'NONE',  ( -10.86508079875781974, 22.20099862734820562, -46.07061504567093380 ) ) ;
#7199 = CARTESIAN_POINT ( 'NONE',  ( 109.1586059443104944, -0.005555961672773799230, 0.004378796245589994425 ) ) ;
#7200 = LINE ( 'NONE', #2569, #13707 ) ;
#7201 = ORIENTED_EDGE ( 'NONE', *, *, #7415, .T. ) ;
#7202 = DIRECTION ( 'NONE',  ( -0.5914120900931443270, -0.7870418015781058818, 0.1754905759872819881 ) ) ;
#7203 = B_SPLINE_CURVE_WITH_KNOTS ( 'NONE', 3,
 ( #27910, #3737, #1433, #23199, #3883, #12099, #12650, #21296 ),
 .UNSPECIFIED., .F., .F.,
 ( 4, 2, 2, 4 ),
 ( 0.000000000000000000, 0.002761524886576646742, 0.005523049773153293485, 0.01104609954630660605 ),
 .UNSPECIFIED. ) ;
#7204 = PRODUCT_DEFINITION_SHAPE ( 'NONE', 'NONE',  #28484 ) ;
#7205 = VERTEX_POINT ( 'NONE', #23340 ) ;
#7206 = CARTESIAN_POINT ( 'NONE',  ( -20.20612092514784663, 18.30568145913877132, 23.26073121129616439 ) ) ;
#7207 = CARTESIAN_POINT ( 'NONE',  ( 16.05277956358233027, 62.52511797226105728, 128.9466020665973076 ) ) ;
#7208 = ORIENTED_EDGE ( 'NONE', *, *, #16415, .F. ) ;
#7209 = EDGE_CURVE ( 'NONE', #20165, #21162, #1291, .T. ) ;
#7210 = ORIENTED_EDGE ( 'NONE', *, *, #9532, .F. ) ;
#7211 = VERTEX_POINT ( 'NONE', #12508 ) ;
#7212 = B_SPLINE_CURVE_WITH_KNOTS ( 'NONE', 3,
 ( #19773, #10874, #17619, #25987, #6703, #15450, #24259 ),
 .UNSPECIFIED., .F., .F.,
 ( 4, 3, 4 ),
 ( 0.000000000000000000, 0.006568092053401781462, 0.02506242213020847681 ),
 .UNSPECIFIED. ) ;
#7213 = CARTESIAN_POINT ( 'NONE',  ( -55.25297051322618813, -0.01306918787467559705, 0.007247191603131494450 ) ) ;
#7214 = CARTESIAN_POINT ( 'NONE',  ( 2.063896406836605024, 96.20114399516394599, 108.8509294491468182 ) ) ;
#7215 = CARTESIAN_POINT ( 'NONE',  ( -20.90916690077959927, 17.17795951644708907, 35.64494649500667833 ) ) ;
#7216 = CARTESIAN_POINT ( 'NONE',  ( 1.833838850855474600, 125.7132320915358719, -72.47782099564513203 ) ) ;
#7217 = VERTEX_POINT ( 'NONE', #15079 ) ;
#7218 = CARTESIAN_POINT ( 'NONE',  ( 2.433796855181205476, -138.8296532063090751, 43.58222566461595449 ) ) ;
#7219 = CARTESIAN_POINT ( 'NONE',  ( 1.833750490713697223, 45.09517546033827529, -137.9248034078892999 ) ) ;
#7220 = LINE ( 'NONE', #13814, #25002 ) ;
#7221 = ORIENTED_EDGE ( 'NONE', *, *, #9105, .T. ) ;
#7222 = ORIENTED_EDGE ( 'NONE', *, *, #24229, .T. ) ;
#7223 = CARTESIAN_POINT ( 'NONE',  ( -8.786685647604887350, -38.68584556812326980, -37.00619870957918778 ) ) ;
#7224 = CARTESIAN_POINT ( 'NONE',  ( 16.05277956358199631, 139.1285124304124565, -34.34928806929293188 ) ) ;
#7225 = CARTESIAN_POINT ( 'NONE',  ( -1.056502255334264895, 43.72121397317241787, 13.66916755949804951 ) ) ;
#7226 = DIRECTION ( 'NONE',  ( -0.5946245182733608248, -0.7858154137795730909, 0.1700465163848173811 ) ) ;
#7227 = CARTESIAN_POINT ( 'NONE',  ( 26.11404676487259024, 102.9690087468808031, -47.08215554553414961 ) ) ;
#7228 = DIRECTION ( 'NONE',  ( 0.000000000000000000, 0.000000000000000000, 1.000000000000000000 ) ) ;
#7229 = VERTEX_POINT ( 'NONE', #23899 ) ;
#7230 = CARTESIAN_POINT ( 'NONE',  ( -55.24271866751342941, 0.001545935011627245191, 0.009369360294294363373 ) ) ;
#7231 = CARTESIAN_POINT ( 'NONE',  ( -8.786685647604887350, -38.68584556812326980, -37.00619870957918778 ) ) ;
#7232 = CARTESIAN_POINT ( 'NONE',  ( -1.045287976400379737, 44.00138577190644185, -12.68782741917337198 ) ) ;
#7233 = CARTESIAN_POINT ( 'NONE',  ( 13.36082413113061307, 151.2941478187907478, 22.28175172543611637 ) ) ;
#7234 = FACE_OUTER_BOUND ( 'NONE', #22087, .T. ) ;
#7235 = EDGE_CURVE ( 'NONE', #5719, #5626, #10090, .T. ) ;
#7236 = EDGE_CURVE ( 'NONE', #26082, #26014, #10151, .T. ) ;
#7237 = ORIENTED_EDGE ( 'NONE', *, *, #13321, .F. ) ;
#7238 = CARTESIAN_POINT ( 'NONE',  ( 25.98552792386796995, 24.57669147553985312, 110.4352299692910435 ) ) ;
#7239 = ORIENTED_EDGE ( 'NONE', *, *, #17893, .T. ) ;
#7240 = ADVANCED_FACE ( 'NONE', ( #9047 ), #25409, .F. ) ;
#7241 = ORIENTED_EDGE ( 'NONE', *, *, #6235, .F. ) ;
#7242 = ORIENTED_EDGE ( 'NONE', *, *, #8529, .F. ) ;
#7243 = FACE_OUTER_BOUND ( 'NONE', #895, .T. ) ;
#7244 =( BOUNDED_SURFACE ( )  B_SPLINE_SURFACE ( 3, 1, ( 
 ( #28361, #27951 ),
 ( #19592, #12971 ),
 ( #19457, #21764 ),
 ( #8659, #23803 ) ),
 .UNSPECIFIED., .F., .F., .F. ) 
 B_SPLINE_SURFACE_WITH_KNOTS ( ( 4, 4 ),
 ( 2, 2 ),
 ( 0.000000000000000000, 1.000000000000000000 ),
 ( 0.000000000000000000, 1.000000000000000000 ),
 .UNSPECIFIED. ) 
 GEOMETRIC_REPRESENTATION_ITEM ( )  RATIONAL_B_SPLINE_SURFACE ( (
 ( 1.000000000000000000, 1.000000000000000000),
 ( 0.9593753223639863714, 0.9995975284513187731),
 ( 0.9593753223639863714, 0.9995975284513187731),
 ( 1.000000000000000000, 1.000000000000000000) ) ) 
 REPRESENTATION_ITEM ( '' )  SURFACE ( )  );
#7245 = CARTESIAN_POINT ( 'NONE',  ( 16.05277956358202829, 53.98852998724762386, -132.7473359121860028 ) ) ;
#7246 = CARTESIAN_POINT ( 'NONE',  ( 10.93730112725990011, -150.7858122213662000, -10.89264110825150489 ) ) ;
#7247 = B_SPLINE_CURVE_WITH_KNOTS ( 'NONE', 3,
 ( #25898, #6189, #14934, #23757, #13192, #13624, #21983, #9325, #247, #26864 ),
 .UNSPECIFIED., .F., .F.,
 ( 4, 3, 3, 4 ),
 ( 1.962615573354718958E-17, 0.0002669560319015750198, 0.0005492286108966149992, 0.0008315040496093386094 ),
 .UNSPECIFIED. ) ;
#7248 = CARTESIAN_POINT ( 'NONE',  ( -7.733045908741342345, 25.81515396910926086, 45.70676731105690749 ) ) ;
#7249 = B_SPLINE_CURVE_WITH_KNOTS ( 'NONE', 3,
 ( #11423, #24694, #22816, #20487, #9553, #18473, #5083 ),
 .UNSPECIFIED., .F., .F.,
 ( 4, 3, 4 ),
 ( 4.037696989527316386E-16, 0.02816610861753247180, 0.04000277880656257640 ),
 .UNSPECIFIED. ) ;
#7250 = CARTESIAN_POINT ( 'NONE',  ( 30.59138290137886429, -107.2355347544030479, -44.78723476287411387 ) ) ;
#7251 = LINE ( 'NONE', #16850, #16216 ) ;
#7252 = CARTESIAN_POINT ( 'NONE',  ( 26.11404676487257603, 113.2169081140373947, 1.130420376097532653 ) ) ;
#7253 = CARTESIAN_POINT ( 'NONE',  ( 10.93730112725971715, 4.928439153520177030, 151.0983828010091372 ) ) ;
#7254 = CARTESIAN_POINT ( 'NONE',  ( -1.619063947482197729, -43.26576862488445130, -16.67502769180545386 ) ) ;
#7255 = CARTESIAN_POINT ( 'NONE',  ( -25.21435515916043713, 16.39063784838786475, 30.48034229288620622 ) ) ;
#7256 = DIRECTION ( 'NONE',  ( 0.5914120900931444380, -0.7398809652418049110, 0.3206367055789364762 ) ) ;
#7257 = EDGE_CURVE ( 'NONE', #17694, #1086, #21147, .T. ) ;
#7258 = CARTESIAN_POINT ( 'NONE',  ( -1.619063947482201282, -11.94059994246191359, -44.80407745103779860 ) ) ;
#7259 = CARTESIAN_POINT ( 'NONE',  ( 10.93730112725936898, 142.1801301103782578, 51.37919228020297879 ) ) ;
#7260 = CARTESIAN_POINT ( 'NONE',  ( 26.11404676487257603, 33.91085499298377925, 108.0249973236468577 ) ) ;
#7261 = CARTESIAN_POINT ( 'NONE',  ( 32.73300124599732186, 0.000000000000000000, 0.000000000000000000 ) ) ;
#7262 = ORIENTED_EDGE ( 'NONE', *, *, #3484, .F. ) ;
#7263 = CARTESIAN_POINT ( 'NONE',  ( 55.49584447822657296, -72.18163437663946524, 7.317474139115394571 ) ) ;
#7264 = ADVANCED_FACE ( 'NONE', ( #6752 ), #20429, .F. ) ;
#7265 = VERTEX_POINT ( 'NONE', #24038 ) ;
#7266 = CARTESIAN_POINT ( 'NONE',  ( -4.178947244162639407, -18.28784278438482858, -45.38689110596713050 ) ) ;
#7267 = CARTESIAN_POINT ( 'NONE',  ( 1.833838850093465034, -30.17001281793454126, 141.9387673160884447 ) ) ;
#7268 = VERTEX_POINT ( 'NONE', #13494 ) ;
#7269 = B_SPLINE_CURVE_WITH_KNOTS ( 'NONE', 3,
 ( #5281, #3272, #16506, #22866 ),
 .UNSPECIFIED., .F., .F.,
 ( 4, 4 ),
 ( 5.928593550334433897E-17, 0.008383748772659517859 ),
 .UNSPECIFIED. ) ;
#7271 = ORIENTED_EDGE ( 'NONE', *, *, #27628, .T. ) ;
#7270 = B_SPLINE_CURVE_WITH_KNOTS ( 'NONE', 3,
 ( #20013, #22333, #24788, #27047, #6934, #11819, #9384, #22777 ),
 .UNSPECIFIED., .F., .F.,
 ( 4, 2, 2, 4 ),
 ( 2.324173423859648542E-16, 0.002761568181852869838, 0.005523136363705506355, 0.01104627272741078026 ),
 .UNSPECIFIED. ) ;
#7272 = EDGE_LOOP ( 'NONE', ( #9874, #16611, #2153, #21456 ) ) ;
#7273 = VERTEX_POINT ( 'NONE', #259 ) ;
#7274 = CARTESIAN_POINT ( 'NONE',  ( 13.84597867724977505, -145.3211459389823403, -20.08297016719535222 ) ) ;
#7275 = CARTESIAN_POINT ( 'NONE',  ( 10.93730112726003156, 125.1380233598492140, -84.82621002473311478 ) ) ;
#7276 = CARTESIAN_POINT ( 'NONE',  ( 109.1586900883932856, -0.004277182003227263107, -0.005715190711481709686 ) ) ;
#7277 = CARTESIAN_POINT ( 'NONE',  ( -20.24419206586952313, -16.36655224501349437, 24.70913649113847299 ) ) ;
#7278 = CARTESIAN_POINT ( 'NONE',  ( 26.11404676487257603, -76.59696442953135431, -83.38016054979861735 ) ) ;
#7279 = CARTESIAN_POINT ( 'NONE',  ( -1.049819078601898381, 0.5100232645225435402, 45.79653735114490587 ) ) ;
#7280 = EDGE_CURVE ( 'NONE', #10634, #3225, #5348, .T. ) ;
#7281 = VERTEX_POINT ( 'NONE', #2404 ) ;
#7282 = ORIENTED_EDGE ( 'NONE', *, *, #24125, .F. ) ;
#7283 = CARTESIAN_POINT ( 'NONE',  ( -1.045287976400362417, -1.530335034933495653, 45.76855895860946788 ) ) ;
#7284 = EDGE_CURVE ( 'NONE', #25711, #5567, #26312, .T. ) ;
#7286 = CARTESIAN_POINT ( 'NONE',  ( -28.13707043255157103, -12.83104814250440029, 18.96624908365860662 ) ) ;
#7285 = CARTESIAN_POINT ( 'NONE',  ( 1.833603222531955401, 84.93295186324861845, 117.6571262511681653 ) ) ;
#7287 = CARTESIAN_POINT ( 'NONE',  ( 2.433796855181233454, 1.451562450949631211, 145.5024947199069913 ) ) ;
#7288 = CARTESIAN_POINT ( 'NONE',  ( 2.108393763691193801, 138.5721856399489695, -43.67806918958995510 ) ) ;
#7289 = ORIENTED_EDGE ( 'NONE', *, *, #26954, .T. ) ;
#7290 = ORIENTED_EDGE ( 'NONE', *, *, #19177, .F. ) ;
#7291 = CARTESIAN_POINT ( 'NONE',  ( -8.786685647604890903, 38.68584556812300690, -37.00619870957947910 ) ) ;
#7292 = EDGE_CURVE ( 'NONE', #6704, #13141, #1577, .T. ) ;
#7293 = CARTESIAN_POINT ( 'NONE',  ( 28.43349137099832546, -115.0977416143053205, -46.80919715693011796 ) ) ;
#7294 = DIRECTION ( 'NONE',  ( -1.000000000000000000, -0.000000000000000000, -0.000000000000000000 ) ) ;
#7295 = ORIENTED_EDGE ( 'NONE', *, *, #4990, .T. ) ;
#7296 = FACE_OUTER_BOUND ( 'NONE', #576, .T. ) ;
#7297 = ORIENTED_EDGE ( 'NONE', *, *, #21591, .F. ) ;
#7298 = CARTESIAN_POINT ( 'NONE',  ( 25.70243777736190438, -112.4037002646848435, 11.07690056740829476 ) ) ;
#7299 = VECTOR ( 'NONE', #23315, 1000.000000000000000 ) ;
#7300 = EDGE_CURVE ( 'NONE', #18479, #8132, #17388, .T. ) ;
#7301 = CARTESIAN_POINT ( 'NONE',  ( -1.113427685307000203, 1.967672929087815881, 45.82016658690749722 ) ) ;
#7302 = DIRECTION ( 'NONE',  ( 1.000000000000000000, -6.938893903907226837E-18, 1.734723475976806709E-18 ) ) ;
#7303 = ORIENTED_EDGE ( 'NONE', *, *, #2099, .T. ) ;
#7304 = FACE_OUTER_BOUND ( 'NONE', #13470, .T. ) ;
#7305 = ORIENTED_EDGE ( 'NONE', *, *, #1604, .T. ) ;
#7306 = B_SPLINE_CURVE_WITH_KNOTS ( 'NONE', 3,
 ( #12747, #6016, #19646, #10468, #23997, #19788, #10753, #4396 ),
 .UNSPECIFIED., .F., .F.,
 ( 4, 2, 2, 4 ),
 ( 0.000000000000000000, 0.0002429592666046805820, 0.0004859185332093611640, 0.0009718370664186841640 ),
 .UNSPECIFIED. ) ;
#7307 = CARTESIAN_POINT ( 'NONE',  ( -1.031422197589711987, -15.60268798220668707, -43.06660437151302290 ) ) ;
#7308 = ORIENTED_EDGE ( 'NONE', *, *, #15984, .T. ) ;
#7309 = B_SPLINE_CURVE_WITH_KNOTS ( 'NONE', 3,
 ( #12792, #2124, #15084, #23773, #28460, #22000 ),
 .UNSPECIFIED., .F., .F.,
 ( 4, 2, 4 ),
 ( 4.982613841084487634E-18, 0.0004335151646191490811, 0.0008670303292382946928 ),
 .UNSPECIFIED. ) ;
#7310 = DIRECTION ( 'NONE',  ( 2.449158383045375968E-16, -0.9997340009326742827, 0.02306355087898700335 ) ) ;
#7311 = CARTESIAN_POINT ( 'NONE',  ( -20.24419206586954090, -10.37009329716784656, -27.76448493191440292 ) ) ;
#7312 = CARTESIAN_POINT ( 'NONE',  ( -28.41354790283022069, 12.60397206714832663, -19.47297445639553715 ) ) ;
#7313 = CARTESIAN_POINT ( 'NONE',  ( 1.833838850093517658, 1.769966374633376447E-14, 145.1097630783160923 ) ) ;
#7314 = VERTEX_POINT ( 'NONE', #6611 ) ;
#7315 = CARTESIAN_POINT ( 'NONE',  ( 2.430230287190572103, 46.34481016237007367, -137.9371479820457580 ) ) ;
#7316 = FACE_OUTER_BOUND ( 'NONE', #22815, .T. ) ;
#7317 = CARTESIAN_POINT ( 'NONE',  ( -20.90916690077961704, -27.35210456531395451, -28.59207721780137135 ) ) ;
#7318 = ORIENTED_EDGE ( 'NONE', *, *, #4676, .T. ) ;
#7319 = ORIENTED_EDGE ( 'NONE', *, *, #12036, .F. ) ;
#7320 = ORIENTED_EDGE ( 'NONE', *, *, #2514, .F. ) ;
#7321 = CARTESIAN_POINT ( 'NONE',  ( 26.11404676487257603, -90.92995828888153653, -67.46175819463459788 ) ) ;
#7322 = DIRECTION ( 'NONE',  ( -0.7637818620346801257, 0.1788995134688785849, -0.6201872550346672064 ) ) ;
#7323 = ADVANCED_FACE ( 'NONE', ( #398 ), #14151, .T. ) ;
#7324 = CARTESIAN_POINT ( 'NONE',  ( 109.1586900883932856, 0.0006456433529069069291, -0.007109207791180753924 ) ) ;
#7325 = CARTESIAN_POINT ( 'NONE',  ( 32.73300124599738581, -115.8010721414081985, -20.69176323058746902 ) ) ;
#7326 = CARTESIAN_POINT ( 'NONE',  ( -23.77929240705205771, -26.20227034809537514, 25.06639637888449457 ) ) ;
#7327 = CARTESIAN_POINT ( 'NONE',  ( 25.64708010899967050, 45.87517365398623781, -103.1718249732469985 ) ) ;
#7328 = ORIENTED_EDGE ( 'NONE', *, *, #746, .T. ) ;
#7329 = CARTESIAN_POINT ( 'NONE',  ( 2.108985857320918367, 145.2876352664462729, -1.281428372376275382 ) ) ;
#7330 = CARTESIAN_POINT ( 'NONE',  ( 109.1586900883932856, -0.003481399864227415798, -0.006231977675082095783 ) ) ;
#7331 = CARTESIAN_POINT ( 'NONE',  ( -40.00000000000000000, 9.797174393178826052E-15, 80.00000000000000000 ) ) ;
#7332 = FACE_BOUND ( 'NONE', #8262, .T. ) ;
#7333 = EDGE_CURVE ( 'NONE', #13658, #17914, #14617, .T. ) ;
#7334 = LINE ( 'NONE', #2163, #21193 ) ;
#7335 = B_SPLINE_CURVE_WITH_KNOTS ( 'NONE', 3,
 ( #6879, #9036, #9602, #532, #15931, #22282 ),
 .UNSPECIFIED., .F., .F.,
 ( 4, 2, 4 ),
 ( 4.982613841084487634E-18, 0.0004335151646191476174, 0.0008670303292382917654 ),
 .UNSPECIFIED. ) ;
#7336 = CARTESIAN_POINT ( 'NONE',  ( 5.340103556456532452, -28.39990973639961069, -144.6887562347052665 ) ) ;
#7337 = CARTESIAN_POINT ( 'NONE',  ( 1.832998868059890096, 59.50898020732687144, -132.3466930259788228 ) ) ;
#7338 = CARTESIAN_POINT ( 'NONE',  ( 25.81918753295376945, 110.3582118788980750, -24.41190151229150374 ) ) ;
#7339 = CARTESIAN_POINT ( 'NONE',  ( 109.1721716018069515, 0.01467989464938422063, 0.008708654716135796198 ) ) ;
#7340 = ORIENTED_EDGE ( 'NONE', *, *, #28413, .F. ) ;
#7341 = B_SPLINE_CURVE_WITH_KNOTS ( 'NONE', 3,
 ( #5447, #9782, #27318, #12078, #6831, #23833, #15436, #4089 ),
 .UNSPECIFIED., .F., .F.,
 ( 4, 2, 2, 4 ),
 ( 3.469446951953614189E-18, 0.0002429588503611278543, 0.0004859177007222522391, 0.0009718354014444975392 ),
 .UNSPECIFIED. ) ;
#7342 = EDGE_LOOP ( 'NONE', ( #22878, #8894, #22257, #17790 ) ) ;
#7343 = CIRCLE ( 'NONE', #23433, 53.53553390275978785 ) ;
#7344 = EDGE_LOOP ( 'NONE', ( #22078, #16345, #14629, #493 ) ) ;
#7345 = B_SPLINE_CURVE_WITH_KNOTS ( 'NONE', 3,
 ( #997, #27324, #7639, #5455, #16395, #14214 ),
 .UNSPECIFIED., .F., .F.,
 ( 4, 2, 4 ),
 ( 1.041737195591640451E-17, 0.0006311571484585964649, 0.001262314296917183172 ),
 .UNSPECIFIED. ) ;
#7346 = DIRECTION ( 'NONE',  ( 0.000000000000000000, 0.000000000000000000, 1.000000000000000000 ) ) ;
#7347 = CARTESIAN_POINT ( 'NONE',  ( -16.86833981943423311, 19.19877306373907189, 39.83928801320569590 ) ) ;
#7348 = CARTESIAN_POINT ( 'NONE',  ( 32.73300124599732186, 0.000000000000000000, 0.000000000000000000 ) ) ;
#7349 = ORIENTED_EDGE ( 'NONE', *, *, #11244, .F. ) ;
#7350 = CARTESIAN_POINT ( 'NONE',  ( -20.20700224038492721, -24.51628800869035274, 16.58740185276737122 ) ) ;
#7351 = CARTESIAN_POINT ( 'NONE',  ( 25.64681081121879203, -103.3177883989782657, 45.54494737132187510 ) ) ;
#7352 = CARTESIAN_POINT ( 'NONE',  ( -1.113548883309553927, -45.82026503946952545, -1.968251867498708174 ) ) ;
#7353 = ORIENTED_EDGE ( 'NONE', *, *, #11400, .F. ) ;
#7354 = ORIENTED_EDGE ( 'NONE', *, *, #417, .T. ) ;
#7355 = CARTESIAN_POINT ( 'NONE',  ( -55.24390624410018802, 0.007245494385991800047, -0.007503127514277958821 ) ) ;
#7356 = CARTESIAN_POINT ( 'NONE',  ( -22.23226125620929139, 30.68305173820436593, 7.677408153693709991 ) ) ;
#7357 = EDGE_CURVE ( 'NONE', #18716, #11755, #22533, .T. ) ;
#7358 = CARTESIAN_POINT ( 'NONE',  ( -55.24198130335446422, -0.009190321388308575826, -0.001391250620105316613 ) ) ;
#7359 = CARTESIAN_POINT ( 'NONE',  ( 26.11404676487259024, -24.64483677384768967, -110.5078194225163912 ) ) ;
#7360 = CARTESIAN_POINT ( 'NONE',  ( 109.1586900883932856, -0.007088091345232584196, -0.0008465529156545617030 ) ) ;
#7361 = CARTESIAN_POINT ( 'NONE',  ( -1.113548883309547710, 1.968251867498868934, -45.82026503946952545 ) ) ;
#7362 = VERTEX_POINT ( 'NONE', #9764 ) ;
#7363 = CARTESIAN_POINT ( 'NONE',  ( 1.833838850855488145, 58.94016894581469757, 132.6005571022081142 ) ) ;
#7364 = CARTESIAN_POINT ( 'NONE',  ( 2.108393763691193357, 16.46048390411989004, -144.3574619851890475 ) ) ;
#7365 = EDGE_CURVE ( 'NONE', #9181, #11289, #2207, .T. ) ;
#7366 = EDGE_CURVE ( 'NONE', #8780, #26877, #2952, .T. ) ;
#7367 = B_SPLINE_CURVE_WITH_KNOTS ( 'NONE', 3,
 ( #13052, #6441, #10619, #21838, #28298, #8888 ),
 .UNSPECIFIED., .F., .F.,
 ( 4, 2, 4 ),
 ( 0.000000000000000000, 0.003570751334075635691, 0.007141502668151271382 ),
 .UNSPECIFIED. ) ;
#7368 = CARTESIAN_POINT ( 'NONE',  ( 25.98107933586719653, -76.50887835172591167, 83.34070894055847134 ) ) ;
#7369 = CARTESIAN_POINT ( 'NONE',  ( 25.98552792386800903, -107.9280603639524543, -33.93357582585603183 ) ) ;
#7370 = VERTEX_POINT ( 'NONE', #18097 ) ;
#7371 = CARTESIAN_POINT ( 'NONE',  ( 25.98107933586701890, 22.45325949158483780, 110.8834224379717881 ) ) ;
#7372 = VERTEX_POINT ( 'NONE', #973 ) ;
#7373 = ORIENTED_EDGE ( 'NONE', *, *, #26238, .F. ) ;
#7374 = ORIENTED_EDGE ( 'NONE', *, *, #7006, .F. ) ;
#7375 = CARTESIAN_POINT ( 'NONE',  ( -1.048172774974299282, 36.44231470008717366, -27.73787987941021171 ) ) ;
#7376 = VECTOR ( 'NONE', #12825, 999.9999999999998863 ) ;
#7377 = CIRCLE ( 'NONE', #9676, 117.6351876552689504 ) ;
#7378 = CARTESIAN_POINT ( 'NONE',  ( 10.93730112725971360, 36.23586118136525158, 146.7718404940643211 ) ) ;
#7379 = CARTESIAN_POINT ( 'NONE',  ( -12.94347594948475333, -48.30328466416771960, -6.555928820869143969 ) ) ;
#7380 = CARTESIAN_POINT ( 'NONE',  ( -22.23226125620943705, -24.24619897613461461, 20.31044300692198945 ) ) ;
#7381 = EDGE_CURVE ( 'NONE', #4903, #15441, #18018, .T. ) ;
#7382 = CARTESIAN_POINT ( 'NONE',  ( -20.20700224038492721, 18.19058640100257662, 23.35150625415638714 ) ) ;
#7383 = VERTEX_POINT ( 'NONE', #22434 ) ;
#7384 = CARTESIAN_POINT ( 'NONE',  ( 25.81918753295379076, -74.93271318951781268, 84.61657260023618221 ) ) ;
#7385 = CARTESIAN_POINT ( 'NONE',  ( -28.41354790283022069, -23.16239616762932130, -1.249099604786995332 ) ) ;
#7386 = B_SPLINE_CURVE_WITH_KNOTS ( 'NONE', 3,
 ( #10955, #21893, #4331, #6643 ),
 .UNSPECIFIED., .F., .F.,
 ( 4, 4 ),
 ( 0.000000000000000000, 0.01077107196513857335 ),
 .UNSPECIFIED. ) ;
#7387 = CARTESIAN_POINT ( 'NONE',  ( 2.108393763691183143, 108.8265195087761867, -96.26428731761880897 ) ) ;
#7388 = EDGE_CURVE ( 'NONE', #6927, #19163, #14253, .T. ) ;
#7389 = ADVANCED_FACE ( 'NONE', ( #20250 ), #16040, .F. ) ;
#7390 = CARTESIAN_POINT ( 'NONE',  ( -20.47566338032516597, -27.87687989047309145, 10.72601609985058957 ) ) ;
#7391 = LINE ( 'NONE', #16451, #22947 ) ;
#7392 = CIRCLE ( 'NONE', #11060, 117.6351876552689504 ) ;
#7393 = CARTESIAN_POINT ( 'NONE',  ( 109.1592201516379674, 0.004867031887010210903, -0.006174480289200333372 ) ) ;
#7394 = VECTOR ( 'NONE', #22123, 1000.000000000000000 ) ;
#7395 = CARTESIAN_POINT ( 'NONE',  ( 2.433796855181233454, 16.65276281464563723, 144.5536872373192807 ) ) ;
#7396 = CARTESIAN_POINT ( 'NONE',  ( -1.045287976400379737, -37.92705037016725100, 25.66401692420055269 ) ) ;
#7397 = CARTESIAN_POINT ( 'NONE',  ( -1.583189561560253589, 11.94859433442901597, -44.83405390829675952 ) ) ;
#7398 = CARTESIAN_POINT ( 'NONE',  ( 25.64700659047693776, 84.06149911284546761, -75.38309044531806080 ) ) ;
#7399 = ORIENTED_EDGE ( 'NONE', *, *, #20269, .F. ) ;
#7400 = DIRECTION ( 'NONE',  ( -0.7637818620346800147, 0.5345501402766299481, 0.3617919495470734992 ) ) ;
#7401 = VECTOR ( 'NONE', #12641, 1000.000000000000000 ) ;
#7402 = ORIENTED_EDGE ( 'NONE', *, *, #11335, .T. ) ;
#7403 = CARTESIAN_POINT ( 'NONE',  ( 109.1587776205901577, -0.007280006032833112421, -0.0008489206734409592177 ) ) ;
#7404 = CARTESIAN_POINT ( 'NONE',  ( 25.64660436782551756, 12.37913844083040793, 112.2303901742707950 ) ) ;
#7405 = ORIENTED_EDGE ( 'NONE', *, *, #11738, .T. ) ;
#7406 =( BOUNDED_SURFACE ( )  B_SPLINE_SURFACE ( 3, 1, ( 
 ( #2597, #442 ),
 ( #26627, #4080 ),
 ( #15539, #13385 ),
 ( #20016, #22033 ) ),
 .UNSPECIFIED., .F., .F., .F. ) 
 B_SPLINE_SURFACE_WITH_KNOTS ( ( 4, 4 ),
 ( 2, 2 ),
 ( 0.000000000000000000, 1.000000000000000000 ),
 ( 0.000000000000000000, 1.000000000000000000 ),
 .UNSPECIFIED. ) 
 GEOMETRIC_REPRESENTATION_ITEM ( )  RATIONAL_B_SPLINE_SURFACE ( (
 ( 1.000000000000000000, 1.000000000000000000),
 ( 0.9956975270656954757, 0.8568959468854893125),
 ( 0.9956975270656954757, 0.8568959468854893125),
 ( 1.000000000000000000, 1.000000000000000000) ) ) 
 REPRESENTATION_ITEM ( '' )  SURFACE ( )  );
#7407 = ORIENTED_EDGE ( 'NONE', *, *, #626, .T. ) ;
#7408 = VERTEX_POINT ( 'NONE', #3136 ) ;
#7409 = CARTESIAN_POINT ( 'NONE',  ( 10.93730112726003156, 115.5857507957718440, -97.44200844886164248 ) ) ;
#7410 = EDGE_CURVE ( 'NONE', #7268, #12091, #10504, .T. ) ;
#7411 = CARTESIAN_POINT ( 'NONE',  ( 55.79472521941426777, 15.83764557006368534, -71.00924468211141516 ) ) ;
#7412 = AXIS2_PLACEMENT_3D ( 'NONE', #19663, #4408, #6305 ) ;
#7413 = AXIS2_PLACEMENT_3D ( 'NONE', #10756, #15178, #17215 ) ;
#7414 = CARTESIAN_POINT ( 'NONE',  ( 26.11404676487259024, -1.130420376096339385, -113.2169081140374232 ) ) ;
#7415 = EDGE_CURVE ( 'NONE', #24730, #15769, #12533, .T. ) ;
#7416 = CARTESIAN_POINT ( 'NONE',  ( 1.833603222531969834, 144.3605362014090474, -14.72553080638845913 ) ) ;
#7417 = CARTESIAN_POINT ( 'NONE',  ( 1.833485406944043827, 29.64752363041542083, 142.0485807715646729 ) ) ;
#7418 = VECTOR ( 'NONE', #13034, 1000.000000000000000 ) ;
#7419 = EDGE_CURVE ( 'NONE', #11485, #5381, #15938, .T. ) ;
#7420 = CARTESIAN_POINT ( 'NONE',  ( -6.574463467970643293, 11.01561683920051848, -50.12924290857540655 ) ) ;
#7421 = FACE_OUTER_BOUND ( 'NONE', #20355, .T. ) ;
#7422 = CARTESIAN_POINT ( 'NONE',  ( -55.24340739397742794, 0.009842732675349290250, 0.002421372372456403153 ) ) ;
#7423 = CARTESIAN_POINT ( 'NONE',  ( 109.1586059443104944, -0.002447596125914214184, -0.006637156007970144468 ) ) ;
#7424 = CARTESIAN_POINT ( 'NONE',  ( -1.049819825607592794, -14.63675055554412374, -43.39756533277876827 ) ) ;
#7425 = CARTESIAN_POINT ( 'NONE',  ( 1.834118845439484335, -96.96525081349928143, -107.9567937753803193 ) ) ;
#7426 = ORIENTED_EDGE ( 'NONE', *, *, #9267, .F. ) ;
#7427 = VERTEX_POINT ( 'NONE', #13774 ) ;
#7428 = CARTESIAN_POINT ( 'NONE',  ( 10.93730112725990367, -133.3192575531795399, -71.28103789255078482 ) ) ;
#7430 = CARTESIAN_POINT ( 'NONE',  ( 26.11404676487257603, 76.59696442953305962, -83.38016054979703995 ) ) ;
#7429 = CARTESIAN_POINT ( 'NONE',  ( 1.833809397773885630, 85.14934054436471911, 117.5007887865410936 ) ) ;
#7431 = CARTESIAN_POINT ( 'NONE',  ( -10.86508079875782684, -9.118642906269649018, -50.32133009257454859 ) ) ;
#7432 = CARTESIAN_POINT ( 'NONE',  ( 32.73300124599738581, 28.19767303745763698, -114.2056417606545153 ) ) ;
#7433 = CARTESIAN_POINT ( 'NONE',  ( -12.82751273423877869, -48.43568301531143305, 6.573887447703340214 ) ) ;
#7434 = CARTESIAN_POINT ( 'NONE',  ( 25.64681081121879203, -112.9102952884414606, 0.4157506337723927414 ) ) ;
#7435 = EDGE_LOOP ( 'NONE', ( #28099, #8912 ) ) ;
#7436 = CARTESIAN_POINT ( 'NONE',  ( 109.1587776205901861, -0.004842060007769426189, 0.005502145856762287804 ) ) ;
#7437 = VECTOR ( 'NONE', #11772, 1000.000000000000000 ) ;
#7438 = CARTESIAN_POINT ( 'NONE',  ( 13.84597867724974840, -55.26821062125468842, -135.8932891738222963 ) ) ;
#7439 = B_SPLINE_CURVE_WITH_KNOTS ( 'NONE', 3,
 ( #18720, #5479, #12376, #5630, #14396, #8090, #1586, #27920, #3463, #21159 ),
 .UNSPECIFIED., .F., .F.,
 ( 4, 2, 2, 2, 4 ),
 ( 4.336808689942017255E-19, 0.0003346267210630946812, 0.0006692534421261889287, 0.001003880163189283230, 0.001338506884252377424 ),
 .UNSPECIFIED. ) ;
#7440 = CARTESIAN_POINT ( 'NONE',  ( 21.16825799904903249, -97.63815233965115681, 93.85612807858974804 ) ) ;
#7441 = VERTEX_POINT ( 'NONE', #2847 ) ;
#7442 = B_SPLINE_CURVE_WITH_KNOTS ( 'NONE', 3,
 ( #1003, #3449, #23047, #18997, #9798, #27778 ),
 .UNSPECIFIED., .F., .F.,
 ( 4, 2, 4 ),
 ( 2.289900696569189619E-17, 0.0006311636237756888855, 0.001262327247551354786 ),
 .UNSPECIFIED. ) ;
#7443 = CARTESIAN_POINT ( 'NONE',  ( -55.25297051322618813, -0.01354497706059863693, -0.006313402748433391727 ) ) ;
#7444 = CARTESIAN_POINT ( 'NONE',  ( -1.619063947482201282, -16.67502769180592992, -43.26576862488428077 ) ) ;
#7445 = EDGE_CURVE ( 'NONE', #3333, #16927, #6366, .T. ) ;
#7446 =( BOUNDED_SURFACE ( )  B_SPLINE_SURFACE ( 3, 1, ( 
 ( #5329, #22918 ),
 ( #27347, #18579 ),
 ( #7660, #14394 ),
 ( #23204, #2262 ) ),
 .UNSPECIFIED., .F., .F., .F. ) 
 B_SPLINE_SURFACE_WITH_KNOTS ( ( 4, 4 ),
 ( 2, 2 ),
 ( 0.000000000000000000, 1.000000000000000000 ),
 ( 0.000000000000000000, 1.000000000000000000 ),
 .UNSPECIFIED. ) 
 GEOMETRIC_REPRESENTATION_ITEM ( )  RATIONAL_B_SPLINE_SURFACE ( (
 ( 1.000000000000000000, 1.000000000000000000),
 ( 0.7789835883360578528, 0.9689951854195403280),
 ( 0.7789835883360578528, 0.9689951854195403280),
 ( 1.000000000000000000, 1.000000000000000000) ) ) 
 REPRESENTATION_ITEM ( '' )  SURFACE ( )  );
#7447 = CARTESIAN_POINT ( 'NONE',  ( -1.044556982611280160, 1.643392503293353180, 45.76404732357876526 ) ) ;
#7448 = ORIENTED_EDGE ( 'NONE', *, *, #23450, .T. ) ;
#7449 = CARTESIAN_POINT ( 'NONE',  ( -55.24728320129491266, -0.009072670231974808847, -0.01137345571546840607 ) ) ;
#7450 = EDGE_CURVE ( 'NONE', #26082, #10457, #1539, .T. ) ;
#7451 = VERTEX_POINT ( 'NONE', #23586 ) ;
#7452 = CARTESIAN_POINT ( 'NONE',  ( 55.49584447822657296, 14.82242356767935654, 71.02133150427260944 ) ) ;
#7453 = EDGE_CURVE ( 'NONE', #18004, #24730, #10503, .T. ) ;
#7454 = EDGE_LOOP ( 'NONE', ( #19689, #5268 ) ) ;
#7455 = DIRECTION ( 'NONE',  ( 0.000000000000000000, 0.000000000000000000, 1.000000000000000000 ) ) ;
#7456 = CARTESIAN_POINT ( 'NONE',  ( 0.000000000000000000, 0.000000000000000000, -80.00000000000000000 ) ) ;
#7457 = EDGE_CURVE ( 'NONE', #16092, #3709, #18320, .T. ) ;
#7458 = FACE_OUTER_BOUND ( 'NONE', #27140, .T. ) ;
#7459 = CARTESIAN_POINT ( 'NONE',  ( 1.833838848569414592, -125.5797553397075035, 72.70900949568731164 ) ) ;
#7460 = ORIENTED_EDGE ( 'NONE', *, *, #17862, .F. ) ;
#7461 = ADVANCED_FACE ( 'NONE', ( #8449 ), #16394, .F. ) ;
#7462 = CARTESIAN_POINT ( 'NONE',  ( 6.224689322667630975, 48.18553814190214979, -139.9988794244327437 ) ) ;
#7463 = CARTESIAN_POINT ( 'NONE',  ( -1.056502255334264895, 26.51074901220504643, -37.35734037467642565 ) ) ;
#7464 = CARTESIAN_POINT ( 'NONE',  ( 19.66333377628726353, -18.85786579350040526, 136.4524620437341298 ) ) ;
#7465 = ORIENTED_EDGE ( 'NONE', *, *, #24384, .T. ) ;
#7466 = AXIS2_PLACEMENT_3D ( 'NONE', #23896, #26037, #15359 ) ;
#7467 = ORIENTED_EDGE ( 'NONE', *, *, #5666, .F. ) ;
#7468 = EDGE_LOOP ( 'NONE', ( #22644, #11388, #17350, #9395 ) ) ;
#7469 = CARTESIAN_POINT ( 'NONE',  ( -1.045287976400383290, 36.12803364096649972, 28.14015102489766917 ) ) ;
#7470 = DIRECTION ( 'NONE',  ( 0.000000000000000000, 0.000000000000000000, 1.000000000000000000 ) ) ;
#7472 = CARTESIAN_POINT ( 'NONE',  ( 32.73300124599737160, -108.9684813982492244, 44.31599526637918274 ) ) ;
#7471 = CARTESIAN_POINT ( 'NONE',  ( 1.833603222531957400, 108.1346772638459441, -96.76619886578220076 ) ) ;
#7473 = CARTESIAN_POINT ( 'NONE',  ( 55.49584447822657296, 29.75369869230953768, 66.16986612640785381 ) ) ;
#7474 = CARTESIAN_POINT ( 'NONE',  ( 109.1592201516379674, 0.003661068210037295243, 0.006957642258146931775 ) ) ;
#7475 = CARTESIAN_POINT ( 'NONE',  ( -22.34422965417126861, 34.15536449444089584, -16.46028608106120572 ) ) ;
#7476 = DIRECTION ( 'NONE',  ( -1.000000000000000000, -0.000000000000000000, -0.000000000000000000 ) ) ;
#7477 = ORIENTED_EDGE ( 'NONE', *, *, #15000, .T. ) ;
#7478 = CARTESIAN_POINT ( 'NONE',  ( -20.20700224038492721, -29.58392382092672790, 0.9908225410481621420 ) ) ;
#7479 = CARTESIAN_POINT ( 'NONE',  ( -55.24300891470650754, 0.003362556190412917256, 0.009225237711101274066 ) ) ;
#7480 = CARTESIAN_POINT ( 'NONE',  ( 26.11404676487257603, -67.46175819463425682, 90.92995828888176391 ) ) ;
#7481 = DIRECTION ( 'NONE',  ( -0.000000000000000000, 0.000000000000000000, 1.000000000000000000 ) ) ;
#7482 = DIRECTION ( 'NONE',  ( 0.000000000000000000, -1.000000000000000000, 0.000000000000000000 ) ) ;
#7483 = CARTESIAN_POINT ( 'NONE',  ( -90.83090735639699176, 0.000000000000000000, -20.00000000000000000 ) ) ;
#7484 = ORIENTED_EDGE ( 'NONE', *, *, #8972, .F. ) ;
#7485 = B_SPLINE_CURVE_WITH_KNOTS ( 'NONE', 3,
 ( #22289, #20542, #26724, #9339, #11625, #825, #15633, #7182 ),
 .UNSPECIFIED., .F., .F.,
 ( 4, 2, 2, 4 ),
 ( 6.938893903907228378E-18, 0.0002429592666046657284, 0.0004859185332093245179, 0.0009718370664186789598 ),
 .UNSPECIFIED. ) ;
#7486 = CARTESIAN_POINT ( 'NONE',  ( 109.1586059443104944, -0.003294606663354695663, 0.006260042619943039129 ) ) ;
#7487 = CARTESIAN_POINT ( 'NONE',  ( -20.47566262905010248, 16.24827521404687403, 25.06314747784817243 ) ) ;
#7488 = CARTESIAN_POINT ( 'NONE',  ( 109.1778270068192853, 0.004349865064712402606, 0.008236503545664826745 ) ) ;
#7489 = AXIS2_PLACEMENT_3D ( 'NONE', #18635, #3652, #23117 ) ;
#7490 = ORIENTED_EDGE ( 'NONE', *, *, #28235, .F. ) ;
#7491 = EDGE_CURVE ( 'NONE', #16414, #27068, #3258, .T. ) ;
#7492 = VERTEX_POINT ( 'NONE', #12472 ) ;
#7493 = AXIS2_PLACEMENT_3D ( 'NONE', #6888, #19974, #4996 ) ;
#7494 = ADVANCED_FACE ( 'NONE', ( #8175 ), #14760, .T. ) ;
#7495 = CARTESIAN_POINT ( 'NONE',  ( -8.786685647604887350, -25.35688121747534751, -47.14957014837345639 ) ) ;
#7496 =( BOUNDED_SURFACE ( )  B_SPLINE_SURFACE ( 3, 1, ( 
 ( #19407, #17519 ),
 ( #2110, #6458 ),
 ( #15070, #13193 ),
 ( #26303, #8902 ) ),
 .UNSPECIFIED., .F., .F., .F. ) 
 B_SPLINE_SURFACE_WITH_KNOTS ( ( 4, 4 ),
 ( 2, 2 ),
 ( 0.000000000000000000, 1.000000000000000000 ),
 ( 0.000000000000000000, 1.000000000000000000 ),
 .UNSPECIFIED. ) 
 GEOMETRIC_REPRESENTATION_ITEM ( )  RATIONAL_B_SPLINE_SURFACE ( (
 ( 1.000000000000000000, 1.000000000000000000),
 ( 0.9934239774497838349, 0.8357310067453913582),
 ( 0.9934239774497838349, 0.8357310067453913582),
 ( 1.000000000000000000, 1.000000000000000000) ) ) 
 REPRESENTATION_ITEM ( '' )  SURFACE ( )  );
#7497 = CARTESIAN_POINT ( 'NONE',  ( -7.078251931573406708, -34.59014398252944034, -38.93060825814217196 ) ) ;
#7498 = DIRECTION ( 'NONE',  ( -1.000000000000000000, 0.000000000000000000, 0.000000000000000000 ) ) ;
#7499 = EDGE_CURVE ( 'NONE', #711, #9163, #25731, .T. ) ;
#7500 = B_SPLINE_CURVE_WITH_KNOTS ( 'NONE', 3,
 ( #14765, #10039, #25447, #14179 ),
 .UNSPECIFIED., .F., .F.,
 ( 4, 4 ),
 ( 2.302416593912983762E-16, 0.008383748772659694801 ),
 .UNSPECIFIED. ) ;
#7501 = DIRECTION ( 'NONE',  ( 1.000000000000000000, -6.938893903907226837E-18, 1.734723475976806709E-18 ) ) ;
#7502 = CARTESIAN_POINT ( 'NONE',  ( -7.733045908741333463, 51.44704017882777691, -10.42750254442556290 ) ) ;
#7503 = ORIENTED_EDGE ( 'NONE', *, *, #20827, .F. ) ;
#7504 = CARTESIAN_POINT ( 'NONE',  ( -20.20700224038492721, -28.44216453106542986, -8.199606986804219844 ) ) ;
#7505 = CARTESIAN_POINT ( 'NONE',  ( 25.64681081121879203, 83.63051021306002042, -75.86069728268907397 ) ) ;
#7506 = CARTESIAN_POINT ( 'NONE',  ( 26.11404676487259024, -33.91085499298451822, 108.0249973236466445 ) ) ;
#7507 = CARTESIAN_POINT ( 'NONE',  ( 1.831572820252009626, -132.9644823688591373, -58.11906524360610860 ) ) ;
#7508 = VERTEX_POINT ( 'NONE', #1670 ) ;
#7509 = VERTEX_POINT ( 'NONE', #20965 ) ;
#7510 = CARTESIAN_POINT ( 'NONE',  ( -1.045287976400362417, -43.05558670614257721, -15.59869763335051651 ) ) ;
#7511 = CARTESIAN_POINT ( 'NONE',  ( 8.186469777910748036, 3.468244369821841477, 149.3111477498017621 ) ) ;
#7512 = CARTESIAN_POINT ( 'NONE',  ( 16.05277956358205316, -19.61822947415880591, -141.9568301782831554 ) ) ;
#7513 = CARTESIAN_POINT ( 'NONE',  ( 55.49584447822657296, -70.91003759562325115, 15.34602024131264386 ) ) ;
#7514 = CARTESIAN_POINT ( 'NONE',  ( 1.833206310202332823, 107.3376456496894065, -97.64934828276996370 ) ) ;
#7515 = CIRCLE ( 'NONE', #9792, 53.53553390275978785 ) ;
#7516 = CARTESIAN_POINT ( 'NONE',  ( 1.832998868059858122, 142.0492247521722788, 29.64765804470121324 ) ) ;
#7517 = ORIENTED_EDGE ( 'NONE', *, *, #15453, .T. ) ;
#7518 = CARTESIAN_POINT ( 'NONE',  ( 26.11404676487257603, 84.89295829319590325, -74.91683232330889552 ) ) ;
#7519 = FACE_OUTER_BOUND ( 'NONE', #6774, .T. ) ;
#7520 = VECTOR ( 'NONE', #7322, 1000.000000000000000 ) ;
#7521 = CARTESIAN_POINT ( 'NONE',  ( 109.1587776205901577, 0.0006832286435102477183, 0.007297420966928598596 ) ) ;
#7522 = CARTESIAN_POINT ( 'NONE',  ( 109.1721716018069657, 0.0002019688922675414973, 0.01706748904932341160 ) ) ;
#7523 = CARTESIAN_POINT ( 'NONE',  ( 25.64660436782554953, -0.5800540083543996861, -112.9095526718340636 ) ) ;
#7524 = VERTEX_POINT ( 'NONE', #10471 ) ;
#7525 = CARTESIAN_POINT ( 'NONE',  ( 25.64703792032469565, -75.44170528134947062, 84.00887408969030901 ) ) ;
#7526 = ORIENTED_EDGE ( 'NONE', *, *, #6283, .F. ) ;
#7527 = B_SPLINE_CURVE_WITH_KNOTS ( 'NONE', 3,
 ( #985, #14072, #25174, #5298, #9776, #27312 ),
 .UNSPECIFIED., .F., .F.,
 ( 4, 2, 4 ),
 ( 0.000000000000000000, 0.0004335184443140231063, 0.0008670368886280462126 ),
 .UNSPECIFIED. ) ;
#7528 = VERTEX_POINT ( 'NONE', #16815 ) ;
#7529 = ORIENTED_EDGE ( 'NONE', *, *, #2628, .F. ) ;
#7530 = EDGE_CURVE ( 'NONE', #8780, #28137, #9245, .T. ) ;
#7531 = AXIS2_PLACEMENT_3D ( 'NONE', #12296, #18492, #21068 ) ;
#7532 = CARTESIAN_POINT ( 'NONE',  ( 2.063896406836605024, -108.8509294491471593, 96.20114399516360493 ) ) ;
#7533 = CARTESIAN_POINT ( 'NONE',  ( -55.25719721206881729, -0.002847566758682281655, 0.01079965405819869988 ) ) ;
#7534 = VECTOR ( 'NONE', #25877, 1000.000000000000114 ) ;
#7535 = EDGE_CURVE ( 'NONE', #20165, #10583, #16142, .T. ) ;
#7536 = CARTESIAN_POINT ( 'NONE',  ( 13.36082413113063083, -109.3026516754239736, 106.9547846563632021 ) ) ;
#7537 = EDGE_CURVE ( 'NONE', #9976, #20677, #25596, .T. ) ;
#7538 = B_SPLINE_CURVE_WITH_KNOTS ( 'NONE', 3,
 ( #16855, #25640, #5919, #8359 ),
 .UNSPECIFIED., .F., .F.,
 ( 4, 4 ),
 ( 8.355534721610419059E-17, 0.008383748772659540410 ),
 .UNSPECIFIED. ) ;
#7539 = CARTESIAN_POINT ( 'NONE',  ( 2.433796855181233454, -126.7346379669250780, -71.49415740225209959 ) ) ;
#7540 = CARTESIAN_POINT ( 'NONE',  ( -20.37983603106074426, -1.508851015062371292, 29.73529213200292531 ) ) ;
#7541 = DIRECTION ( 'NONE',  ( -1.000000000000000000, -0.000000000000000000, -0.000000000000000000 ) ) ;
#7542 = CARTESIAN_POINT ( 'NONE',  ( 25.64681081121879203, -97.99105938547964456, 56.09509703373309719 ) ) ;
#7543 = CARTESIAN_POINT ( 'NONE',  ( 1.831572820252009626, 137.7011124121623311, -45.77972211429671745 ) ) ;
#7544 = CARTESIAN_POINT ( 'NONE',  ( 2.108393763691203571, -31.45977531353388201, 141.8460676169243015 ) ) ;
#7545 = CARTESIAN_POINT ( 'NONE',  ( 10.93730112726006176, 146.7718404940648611, -36.23586118136403655 ) ) ;
#7546 = CARTESIAN_POINT ( 'NONE',  ( -20.57838717382308147, -10.78122205916981358, 27.96569011373096814 ) ) ;
#7547 = CARTESIAN_POINT ( 'NONE',  ( -1.058473599757816963, -25.48501014712370960, 38.06357893967457784 ) ) ;
#7548 = CARTESIAN_POINT ( 'NONE',  ( -8.786685647604890903, 7.199674155858966529, -53.04920435127184675 ) ) ;
#7549 = CARTESIAN_POINT ( 'NONE',  ( -1.259920593601994376, 35.85909937955963755, 28.82601305773611600 ) ) ;
#7550 = CARTESIAN_POINT ( 'NONE',  ( 25.73574536432415272, 112.2643803187785494, 12.61003673871928399 ) ) ;
#7551 = FACE_OUTER_BOUND ( 'NONE', #7344, .T. ) ;
#7552 = CARTESIAN_POINT ( 'NONE',  ( 16.05277956358202118, -139.1285124304122007, 34.34928806929384137 ) ) ;
#7553 = EDGE_CURVE ( 'NONE', #2725, #10615, #5736, .T. ) ;
#7554 = ORIENTED_EDGE ( 'NONE', *, *, #20710, .T. ) ;
#7555 = CARTESIAN_POINT ( 'NONE',  ( 2.433796855181233454, -96.28145139437756939, 109.1007109081222666 ) ) ;
#7556 = ORIENTED_EDGE ( 'NONE', *, *, #1050, .F. ) ;
#7557 = CARTESIAN_POINT ( 'NONE',  ( 1.833485406944057594, -15.69895494453287021, -144.2578170162064737 ) ) ;
#7558 = CARTESIAN_POINT ( 'NONE',  ( 55.49584447822657296, -69.08290406177594889, 22.16497542184382397 ) ) ;
#7559 = B_SPLINE_CURVE_WITH_KNOTS ( 'NONE', 3,
 ( #12648, #19140, #25764, #6056 ),
 .UNSPECIFIED., .F., .F.,
 ( 4, 4 ),
 ( 0.000000000000000000, 0.01077107196513847794 ),
 .UNSPECIFIED. ) ;
#7560 = VERTEX_POINT ( 'NONE', #3976 ) ;
#7561 = EDGE_CURVE ( 'NONE', #26729, #10772, #2521, .T. ) ;
#7562 = ORIENTED_EDGE ( 'NONE', *, *, #20303, .F. ) ;
#7563 = ORIENTED_EDGE ( 'NONE', *, *, #5165, .T. ) ;
#7564 = ADVANCED_FACE ( 'NONE', ( #3550 ), #12190, .F. ) ;
#7565 = ORIENTED_EDGE ( 'NONE', *, *, #7641, .F. ) ;
#7566 = CARTESIAN_POINT ( 'NONE',  ( 2.430230287190592531, 86.70145658344658557, 116.8646894862415166 ) ) ;
#7567 = CARTESIAN_POINT ( 'NONE',  ( 26.11404676487257603, 92.25884714080498838, -65.63269960453146723 ) ) ;
#7568 = DIRECTION ( 'NONE',  ( 1.000000000000000000, -6.938893903907226837E-18, 1.734723475976806709E-18 ) ) ;
#7569 = CARTESIAN_POINT ( 'NONE',  ( 25.64681081121879203, -66.70335573067929147, 91.10197563707923507 ) ) ;
#7570 = CARTESIAN_POINT ( 'NONE',  ( -1.539760825549688628, -2.469813586483410539, -46.22267384399379608 ) ) ;
#7571 = SHAPE_REPRESENTATION ( 'bevel straight', ( #27263 ), #16248 ) ;
#7572 = CARTESIAN_POINT ( 'NONE',  ( 2.263178607246672858, 71.48082837426177605, -126.6115608827429782 ) ) ;
#7573 = CARTESIAN_POINT ( 'NONE',  ( 1.832998868059858122, 14.63705790014008379, 144.3700883710217795 ) ) ;
#7574 = CARTESIAN_POINT ( 'NONE',  ( 109.1587776205901861, 0.004375189885423106176, 0.005880209827414138897 ) ) ;
#7575 = CARTESIAN_POINT ( 'NONE',  ( -20.20700224038492721, 16.58740185276746359, 24.51628800869029234 ) ) ;
#7577 = FACE_OUTER_BOUND ( 'NONE', #14116, .T. ) ;
#7576 = CARTESIAN_POINT ( 'NONE',  ( 2.433796855181205476, 60.50726454508082952, -132.3327394885224919 ) ) ;
#7578 = CARTESIAN_POINT ( 'NONE',  ( -20.57838717382308147, 10.78122205917039977, 27.96569011373074076 ) ) ;
#7579 = ORIENTED_EDGE ( 'NONE', *, *, #26542, .T. ) ;
#7580 = ORIENTED_EDGE ( 'NONE', *, *, #1051, .T. ) ;
#7581 = CARTESIAN_POINT ( 'NONE',  ( -55.24300891470648622, -0.005486913146696059326, -0.008142823778062177609 ) ) ;
#7583 = CARTESIAN_POINT ( 'NONE',  ( 25.70243777736189728, 57.10783651465103361, -97.44734253939026303 ) ) ;
#7582 = DIRECTION ( 'NONE',  ( -1.000000000000000000, -0.000000000000000000, -0.000000000000000000 ) ) ;
#7584 = CARTESIAN_POINT ( 'NONE',  ( 1.833809397773816574, -85.43729755723236963, 117.2915757704554949 ) ) ;
#7585 = DIRECTION ( 'NONE',  ( -0.000000000000000000, 1.000000000000000000, -0.000000000000000000 ) ) ;
#7586 = CARTESIAN_POINT ( 'NONE',  ( -1.583189561560252701, 16.68617981233703063, -43.29471907393747898 ) ) ;
#7587 =( BOUNDED_SURFACE ( )  B_SPLINE_SURFACE ( 3, 1, ( 
 ( #27192, #20874 ),
 ( #22913, #9953 ),
 ( #18263, #7507 ),
 ( #24921, #25066 ) ),
 .UNSPECIFIED., .F., .F., .F. ) 
 B_SPLINE_SURFACE_WITH_KNOTS ( ( 4, 4 ),
 ( 2, 2 ),
 ( 0.000000000000000000, 1.000000000000000000 ),
 ( 0.000000000000000000, 1.000000000000000000 ),
 .UNSPECIFIED. ) 
 GEOMETRIC_REPRESENTATION_ITEM ( )  RATIONAL_B_SPLINE_SURFACE ( (
 ( 1.000000000000000000, 1.000000000000000000),
 ( 0.9956975270656954757, 0.8568959468854893125),
 ( 0.9956975270656954757, 0.8568959468854893125),
 ( 1.000000000000000000, 1.000000000000000000) ) ) 
 REPRESENTATION_ITEM ( '' )  SURFACE ( )  );
#7588 = VERTEX_POINT ( 'NONE', #23865 ) ;
#7589 = CARTESIAN_POINT ( 'NONE',  ( 1.833485406944043827, 44.33323125129927433, 138.1714136985309835 ) ) ;
#7590 = CARTESIAN_POINT ( 'NONE',  ( 109.1778270068192853, -0.005186985107090082321, 0.007736698406808958234 ) ) ;
#7591 = CARTESIAN_POINT ( 'NONE',  ( 1.833809397773858541, -15.34508223002545968, 144.2961330457379461 ) ) ;
#7592 = ORIENTED_EDGE ( 'NONE', *, *, #21932, .T. ) ;
#7593 = CARTESIAN_POINT ( 'NONE',  ( -20.21097721712959583, 17.67178718142858429, -23.76068428613687189 ) ) ;
#7594 = CARTESIAN_POINT ( 'NONE',  ( 2.108985857320907709, 116.7869613039531771, -86.43462668039018126 ) ) ;
#7595 = ADVANCED_FACE ( 'NONE', ( #84 ), #5095, .T. ) ;
#7596 = EDGE_CURVE ( 'NONE', #27156, #14400, #1432, .T. ) ;
#7597 = EDGE_CURVE ( 'NONE', #246, #15408, #20064, .T. ) ;
#7598 = ORIENTED_EDGE ( 'NONE', *, *, #27973, .F. ) ;
#7599 = CARTESIAN_POINT ( 'NONE',  ( -55.24390624410018802, -0.01027195578987978239, -0.001811362924362686826 ) ) ;
#7600 = VECTOR ( 'NONE', #16846, 1000.000000000000227 ) ;
#7601 = EDGE_LOOP ( 'NONE', ( #10857, #3947, #23968, #26900 ) ) ;
#7602 = CARTESIAN_POINT ( 'NONE',  ( -1.155001620486252101, -42.97366440495923001, -16.13799328198405902 ) ) ;
#7603 = CARTESIAN_POINT ( 'NONE',  ( 8.186469829614463123, 137.8131829164344708, -57.56191610809234760 ) ) ;
#7604 = ORIENTED_EDGE ( 'NONE', *, *, #1562, .F. ) ;
#7605 =( LENGTH_UNIT ( ) NAMED_UNIT ( * ) SI_UNIT ( .MILLI., .METRE. ) );
#7606 = FACE_OUTER_BOUND ( 'NONE', #11780, .T. ) ;
#7607 = CARTESIAN_POINT ( 'NONE',  ( -1.046936909428682894, 15.35929614323726256, 43.14407378092978718 ) ) ;
#7608 = DIRECTION ( 'NONE',  ( 0.000000000000000000, -6.938893903907228378E-16, -1.000000000000000000 ) ) ;
#7609 = CARTESIAN_POINT ( 'NONE',  ( -23.79248802219728987, 22.01156985585204851, 24.83956736572385893 ) ) ;
#7610 = EDGE_LOOP ( 'NONE', ( #4, #14931 ) ) ;
#7611 = B_SPLINE_CURVE_WITH_KNOTS ( 'NONE', 3,
 ( #12147, #1201, #26817, #4942, #22517, #2783, #11563, #632, #26951, #768 ),
 .UNSPECIFIED., .F., .F.,
 ( 4, 2, 2, 2, 4 ),
 ( 1.301042606982605128E-18, 0.0003346267210630945186, 0.0006692534421261877361, 0.001003880163189281062, 0.001338506884252374171 ),
 .UNSPECIFIED. ) ;
#7612 = ADVANCED_FACE ( 'NONE', ( #12886 ), #19790, .F. ) ;
#7613 = LINE ( 'NONE', #16812, #13456 ) ;
#7615 = CARTESIAN_POINT ( 'NONE',  ( -1.048994561756795729, 43.78680886990941445, -13.42228657661138058 ) ) ;
#7614 = CARTESIAN_POINT ( 'NONE',  ( -20.20700224038492721, 10.08426345511588984, -27.82980252387822517 ) ) ;
#7616 = CARTESIAN_POINT ( 'NONE',  ( -21.41427618760458529, 25.94789270595506991, -16.60878262545428541 ) ) ;
#7617 = VERTEX_POINT ( 'NONE', #28284 ) ;
#7618 = ORIENTED_EDGE ( 'NONE', *, *, #3005, .F. ) ;
#7619 = ORIENTED_EDGE ( 'NONE', *, *, #22055, .T. ) ;
#7620 = CARTESIAN_POINT ( 'NONE',  ( 25.73574536432415272, -90.91878692681981988, -67.05280231777601330 ) ) ;
#7621 = DIRECTION ( 'NONE',  ( -0.5946245182733608248, -0.3297108033645170799, -0.7332888028688958615 ) ) ;
#7623 = CARTESIAN_POINT ( 'NONE',  ( 1.832998868059858122, -141.8272129421606564, -30.69214149074159792 ) ) ;
#7622 = CARTESIAN_POINT ( 'NONE',  ( 32.73300124599732186, 0.000000000000000000, 0.000000000000000000 ) ) ;
#7624 = CARTESIAN_POINT ( 'NONE',  ( -20.20700224038492010, -8.199606986804138131, 28.44216453106544762 ) ) ;
#7625 = CARTESIAN_POINT ( 'NONE',  ( -21.81686047589429123, 26.62923599424970433, -27.83628745321458453 ) ) ;
#7626 = CARTESIAN_POINT ( 'NONE',  ( 1.833691583653522361, 107.5990239011827043, 97.36155720551511195 ) ) ;
#7627 = CARTESIAN_POINT ( 'NONE',  ( -22.34422965417126505, -33.39267070835835227, -17.95715691811035342 ) ) ;
#7628 = VERTEX_POINT ( 'NONE', #2367 ) ;
#7629 = CARTESIAN_POINT ( 'NONE',  ( 9.884929003653626367, 135.7578851563895057, -65.04493172071342144 ) ) ;
#7630 = CARTESIAN_POINT ( 'NONE',  ( -1.045287976400362417, -43.05558670614257721, -15.59869763335051651 ) ) ;
#7631 =( BOUNDED_SURFACE ( )  B_SPLINE_SURFACE ( 3, 1, ( 
 ( #16276, #5785 ),
 ( #14543, #23348 ),
 ( #28332, #8219 ),
 ( #21871, #19425 ) ),
 .UNSPECIFIED., .F., .F., .F. ) 
 B_SPLINE_SURFACE_WITH_KNOTS ( ( 4, 4 ),
 ( 2, 2 ),
 ( 0.000000000000000000, 1.000000000000000000 ),
 ( 0.000000000000000000, 1.000000000000000000 ),
 .UNSPECIFIED. ) 
 GEOMETRIC_REPRESENTATION_ITEM ( )  RATIONAL_B_SPLINE_SURFACE ( (
 ( 1.000000000000000000, 1.000000000000000000),
 ( 0.7789835883360576307, 0.9689951854195403280),
 ( 0.7789835883360576307, 0.9689951854195403280),
 ( 1.000000000000000000, 1.000000000000000000) ) ) 
 REPRESENTATION_ITEM ( '' )  SURFACE ( )  );
#7632 = CARTESIAN_POINT ( 'NONE',  ( 119.2224693531408803, 90.00000000000005684, 19.99999999999997513 ) ) ;
#7633 = EDGE_CURVE ( 'NONE', #16816, #9521, #22118, .T. ) ;
#7634 = CARTESIAN_POINT ( 'NONE',  ( 25.64660436782550335, -66.83584345385848735, -91.00479974714311027 ) ) ;
#7635 = CARTESIAN_POINT ( 'NONE',  ( 25.65782528836479415, 75.12678957786506828, 84.30028114518196958 ) ) ;
#7636 = CARTESIAN_POINT ( 'NONE',  ( -20.20700224038492721, 16.58740185276746359, 24.51628800869029234 ) ) ;
#7637 = CARTESIAN_POINT ( 'NONE',  ( -20.57838717382308502, 28.96176188950218844, -7.715628353033780584 ) ) ;
#7638 = ORIENTED_EDGE ( 'NONE', *, *, #2483, .F. ) ;
#7639 = CARTESIAN_POINT ( 'NONE',  ( 1.894214914920992365, 29.24491455759132208, -142.1734439042093925 ) ) ;
#7641 = EDGE_CURVE ( 'NONE', #5555, #8700, #6673, .T. ) ;
#7640 = CARTESIAN_POINT ( 'NONE',  ( 32.73300124599732186, 0.000000000000000000, 0.000000000000000000 ) ) ;
#7642 = CARTESIAN_POINT ( 'NONE',  ( 109.1624594426973260, 0.01582142368018301520, 0.002129375066970686133 ) ) ;
#7643 = ADVANCED_FACE ( 'NONE', ( #26417 ), #2424, .F. ) ;
#7644 = ORIENTED_EDGE ( 'NONE', *, *, #24913, .T. ) ;
#7645 = B_SPLINE_CURVE_WITH_KNOTS ( 'NONE', 3,
 ( #12493, #19390, #3992, #28026, #21695, #6182 ),
 .UNSPECIFIED., .F., .F.,
 ( 4, 2, 4 ),
 ( 6.505213034913026604E-19, 0.0004335151646191473464, 0.0008670303292382940423 ),
 .UNSPECIFIED. ) ;
#7646 = VERTEX_POINT ( 'NONE', #4688 ) ;
#7647 = CARTESIAN_POINT ( 'NONE',  ( 13.36082413113061307, 129.1512766091121307, 81.89226687792132964 ) ) ;
#7648 = CARTESIAN_POINT ( 'NONE',  ( 109.1624594426973260, -0.01216903288310115100, 0.01033277910988593222 ) ) ;
#7649 = CARTESIAN_POINT ( 'NONE',  ( 109.1586900883932856, -0.004277182003227263107, -0.005715190711481709686 ) ) ;
#7650 = VECTOR ( 'NONE', #15834, 1000.000000000000000 ) ;
#7651 = CARTESIAN_POINT ( 'NONE',  ( 32.73300124599740002, 72.21147546950675178, -92.86301839379947864 ) ) ;
#7652 = CARTESIAN_POINT ( 'NONE',  ( 1.833838850093451933, 125.6687394363107728, -72.55488452980732461 ) ) ;
#7653 = VERTEX_POINT ( 'NONE', #17491 ) ;
#7654 = CARTESIAN_POINT ( 'NONE',  ( 10.93730112725932635, 149.7554878793145576, 20.69552240458357062 ) ) ;
#7655 = CARTESIAN_POINT ( 'NONE',  ( 25.64692872815575697, 34.58541472378651349, 107.4838747185722383 ) ) ;
#7656 = CARTESIAN_POINT ( 'NONE',  ( 10.93730112725971004, 51.37919228020272300, 142.1801301103785420 ) ) ;
#7657 = ORIENTED_EDGE ( 'NONE', *, *, #12407, .F. ) ;
#7658 = VERTEX_POINT ( 'NONE', #13459 ) ;
#7659 = CARTESIAN_POINT ( 'NONE',  ( -8.786685647604890903, -48.22796981442785835, -23.24040270374372952 ) ) ;
#7660 = CARTESIAN_POINT ( 'NONE',  ( -55.24728320129491266, 0.01362040845703093098, -0.005114031043466513160 ) ) ;
#7661 = CARTESIAN_POINT ( 'NONE',  ( 1.894214914920965276, 84.54370816135735822, -117.9869255019023768 ) ) ;
#7662 = CARTESIAN_POINT ( 'NONE',  ( 25.64681081121879203, -75.86069728269045243, 83.63051021305875565 ) ) ;
#7663 = CARTESIAN_POINT ( 'NONE',  ( 1.833206308920057870, -84.68961866582925779, -117.8322276971144902 ) ) ;
#7664 = CARTESIAN_POINT ( 'NONE',  ( -1.044557008772713402, 1.643388457097889166, -45.76404748504490527 ) ) ;
#7665 = CARTESIAN_POINT ( 'NONE',  ( 109.1587776205901577, -0.006305329297952444977, -0.003736572840486921884 ) ) ;
#7666 = ORIENTED_EDGE ( 'NONE', *, *, #1731, .T. ) ;
#7667 = CARTESIAN_POINT ( 'NONE',  ( 25.64670758986457955, 84.24158725144721416, -75.18147256661973188 ) ) ;
#7668 = CARTESIAN_POINT ( 'NONE',  ( 1.833485406944043827, 29.64752363041542083, 142.0485807715646729 ) ) ;
#7669 = CARTESIAN_POINT ( 'NONE',  ( 1.832998868059858122, -96.70023740551195601, 108.1944082009154329 ) ) ;
#7670 = ADVANCED_FACE ( 'NONE', ( #20078 ), #983, .T. ) ;
#7671 = EDGE_CURVE ( 'NONE', #9135, #5379, #24880, .T. ) ;
#7672 = CARTESIAN_POINT ( 'NONE',  ( 26.11404676487257603, -76.59696442953247697, 83.38016054979757996 ) ) ;
#7673 = CARTESIAN_POINT ( 'NONE',  ( 19.66333377628723156, -135.6014041990441399, 24.23123354948793207 ) ) ;
#7675 = EDGE_CURVE ( 'NONE', #9661, #1788, #143, .T. ) ;
#7674 = CARTESIAN_POINT ( 'NONE',  ( 16.05277956358201763, -118.6216415718956085, -80.40847413522669740 ) ) ;
#7676 = CARTESIAN_POINT ( 'NONE',  ( -1.044556982611268170, -28.22896456560694034, -36.05793013899088351 ) ) ;
#7677 = ORIENTED_EDGE ( 'NONE', *, *, #2483, .T. ) ;
#7678 =( BOUNDED_SURFACE ( )  B_SPLINE_SURFACE ( 3, 1, ( 
 ( #5729, #5868 ),
 ( #10340, #968 ),
 ( #12194, #16660 ),
 ( #5425, #14188 ) ),
 .UNSPECIFIED., .F., .F., .F. ) 
 B_SPLINE_SURFACE_WITH_KNOTS ( ( 4, 4 ),
 ( 2, 2 ),
 ( 0.000000000000000000, 1.000000000000000000 ),
 ( 0.000000000000000000, 1.000000000000000000 ),
 .UNSPECIFIED. ) 
 GEOMETRIC_REPRESENTATION_ITEM ( )  RATIONAL_B_SPLINE_SURFACE ( (
 ( 1.000000000000000000, 1.000000000000000000),
 ( 0.9956975270656955868, 0.8568959468854907557),
 ( 0.9956975270656955868, 0.8568959468854907557),
 ( 1.000000000000000000, 1.000000000000000000) ) ) 
 REPRESENTATION_ITEM ( '' )  SURFACE ( )  );
#7679 = EDGE_CURVE ( 'NONE', #6523, #1292, #14569, .T. ) ;
#7680 = VERTEX_POINT ( 'NONE', #18058 ) ;
#7681 = EDGE_LOOP ( 'NONE', ( #15101, #19007, #28071, #20572 ) ) ;
#7682 = CARTESIAN_POINT ( 'NONE',  ( 25.64708228042120908, -110.4357030047556236, -23.51409906510326309 ) ) ;
#7683 = DIRECTION ( 'NONE',  ( 1.000000000000000000, -6.938893903907226837E-18, 1.734723475976806709E-18 ) ) ;
#7684 = B_SPLINE_CURVE_WITH_KNOTS ( 'NONE', 3,
 ( #27839, #19067, #16772, #25555, #12427, #1497 ),
 .UNSPECIFIED., .F., .F.,
 ( 4, 2, 4 ),
 ( 0.000000000000000000, 0.0004335184443140195285, 0.0008670368886280390569 ),
 .UNSPECIFIED. ) ;
#7685 = CARTESIAN_POINT ( 'NONE',  ( 13.36082413113063083, 135.4964217943307290, 70.90215303572172445 ) ) ;
#7686 = CARTESIAN_POINT ( 'NONE',  ( -20.20700224038492721, -23.35150625415645820, 18.19058640100249491 ) ) ;
#7687 = CARTESIAN_POINT ( 'NONE',  ( 109.1589550718175161, -0.005994046294305938397, 0.004632048724982886813 ) ) ;
#7688 = CARTESIAN_POINT ( 'NONE',  ( -55.24300891470650754, -0.008142823778061761275, -0.005486913146700541852 ) ) ;
#7689 = CARTESIAN_POINT ( 'NONE',  ( 8.186469829614447136, 90.56875932797750295, -118.7566730983339909 ) ) ;
#7690 = LINE ( 'NONE', #20181, #475 ) ;
#7691 = CARTESIAN_POINT ( 'NONE',  ( -12.82751273423881777, 23.15139349681311387, -43.04932478553539710 ) ) ;
#7692 = CARTESIAN_POINT ( 'NONE',  ( 55.49584447822657296, 0.2676470673956655166, 72.55110015779771970 ) ) ;
#7693 = CARTESIAN_POINT ( 'NONE',  ( 16.05277956358201763, -126.3767940428296725, -67.56865019683978346 ) ) ;
#7694 = CARTESIAN_POINT ( 'NONE',  ( 9.884929003653626367, -11.54837932063133188, 150.0922431698404580 ) ) ;
#7695 = EDGE_CURVE ( 'NONE', #25484, #16069, #19710, .T. ) ;
#7696 = CARTESIAN_POINT ( 'NONE',  ( 1.894214914920974602, 16.12044375672287799, 144.2521558665607699 ) ) ;
#7697 = CARTESIAN_POINT ( 'NONE',  ( 32.73300124599736449, -117.3295799645430435, 8.473903470905730373 ) ) ;
#7698 = CARTESIAN_POINT ( 'NONE',  ( 1.831572820252009626, 132.9644823688595352, 58.11906524360522752 ) ) ;
#7699 = CARTESIAN_POINT ( 'NONE',  ( 109.1778270068192853, -0.009293669915260191483, -0.0006237116683871008664 ) ) ;
#7700 = CARTESIAN_POINT ( 'NONE',  ( -1.113427685307011084, 35.91272432484659305, -28.52429901637181686 ) ) ;
#7701 = ORIENTED_EDGE ( 'NONE', *, *, #6845, .F. ) ;
#7702 = CARTESIAN_POINT ( 'NONE',  ( -1.044556982611269502, 25.56989963842203650, -37.98985389331818396 ) ) ;
#7703 = ORIENTED_EDGE ( 'NONE', *, *, #11438, .T. ) ;
#7705 = EDGE_CURVE ( 'NONE', #14322, #10817, #1890, .T. ) ;
#7704 = CARTESIAN_POINT ( 'NONE',  ( 109.1586900883932856, -0.007137750914550312215, 0.0001010081143975802818 ) ) ;
#7706 = LINE ( 'NONE', #7558, #21711 ) ;
#7707 = VERTEX_POINT ( 'NONE', #16332 ) ;
#7708 = ADVANCED_FACE ( 'NONE', ( #4831 ), #1345, .F. ) ;
#7709 = B_SPLINE_CURVE_WITH_KNOTS ( 'NONE', 3,
 ( #18681, #27308, #23019, #981, #16674, #9772, #12068 ),
 .UNSPECIFIED., .F., .F.,
 ( 4, 3, 4 ),
 ( 0.000000000000000000, 0.02398743853561371986, 0.04000277880656209067 ),
 .UNSPECIFIED. ) ;
#7710 = VERTEX_POINT ( 'NONE', #7150 ) ;
#7711 =( BOUNDED_SURFACE ( )  B_SPLINE_SURFACE ( 3, 1, ( 
 ( #13281, #2635 ),
 ( #10998, #9266 ),
 ( #197, #4501 ),
 ( #22067, #17453 ) ),
 .UNSPECIFIED., .F., .F., .F. ) 
 B_SPLINE_SURFACE_WITH_KNOTS ( ( 4, 4 ),
 ( 2, 2 ),
 ( 0.000000000000000000, 1.000000000000000000 ),
 ( 0.000000000000000000, 1.000000000000000000 ),
 .UNSPECIFIED. ) 
 GEOMETRIC_REPRESENTATION_ITEM ( )  RATIONAL_B_SPLINE_SURFACE ( (
 ( 1.000000000000000000, 1.000000000000000000),
 ( 0.7789835883360578528, 0.9689951854195403280),
 ( 0.7789835883360578528, 0.9689951854195403280),
 ( 1.000000000000000000, 1.000000000000000000) ) ) 
 REPRESENTATION_ITEM ( '' )  SURFACE ( )  );
#7712 = ORIENTED_EDGE ( 'NONE', *, *, #22642, .F. ) ;
#7713 = DIRECTION ( 'NONE',  ( 0.5946245182733608248, -0.3243201896541589302, -0.7356888587241646738 ) ) ;
#7714 = DIRECTION ( 'NONE',  ( 0.000000000000000000, 0.000000000000000000, 1.000000000000000000 ) ) ;
#7715 = B_SPLINE_CURVE_WITH_KNOTS ( 'NONE', 3,
 ( #737, #27358, #9525, #5197, #5050, #24797, #7368, #7672 ),
 .UNSPECIFIED., .F., .F.,
 ( 4, 2, 2, 4 ),
 ( 0.000000000000000000, 0.0002429588503611235174, 0.0004859177007222470349, 0.0009718354014444994908 ),
 .UNSPECIFIED. ) ;
#7716 = CARTESIAN_POINT ( 'NONE',  ( -25.21435515916043002, 34.05351380035335040, -6.169479169075572145 ) ) ;
#7717 = CARTESIAN_POINT ( 'NONE',  ( -1.239374126674604337, 44.48112152129347407, -11.92219841463844432 ) ) ;
#7718 = CARTESIAN_POINT ( 'NONE',  ( 25.64660436782536479, 107.5626123667561416, 34.33930645842045948 ) ) ;
#7719 = CARTESIAN_POINT ( 'NONE',  ( -1.058197053496163109, 28.32422455455077781, -36.00048521498961662 ) ) ;
#7720 = CARTESIAN_POINT ( 'NONE',  ( 1.833809397773860539, -58.85883548850502933, -132.6366580004813045 ) ) ;
#7721 = CARTESIAN_POINT ( 'NONE',  ( 109.1624594426973118, -0.007576898892906994316, 0.01405141589344821758 ) ) ;
#7722 = CARTESIAN_POINT ( 'NONE',  ( 1.833485406944043827, 58.53321471326877656, 132.7804117027889674 ) ) ;
#7723 = CARTESIAN_POINT ( 'NONE',  ( -20.20700224038492721, -18.19058640100206503, 23.35150625415678860 ) ) ;
#7724 = ORIENTED_EDGE ( 'NONE', *, *, #3803, .T. ) ;
#7725 = ORIENTED_EDGE ( 'NONE', *, *, #8778, .T. ) ;
#7726 = CARTESIAN_POINT ( 'NONE',  ( -4.780792508754331038, 11.68149851467529210, 48.13366140756546230 ) ) ;
#7728 = CARTESIAN_POINT ( 'NONE',  ( -1.045287976400362417, 25.66401692420069125, 37.92705037016716574 ) ) ;
#7727 = CARTESIAN_POINT ( 'NONE',  ( 1.833691583653570545, 85.00512109099250324, 117.6050685739171797 ) ) ;
#7729 = EDGE_CURVE ( 'NONE', #24769, #12561, #9430, .T. ) ;
#7730 = CARTESIAN_POINT ( 'NONE',  ( 1.833838850855499025, -85.36536653357421756, 117.3439621615260222 ) ) ;
#7731 = CARTESIAN_POINT ( 'NONE',  ( 32.73300124599732186, 0.000000000000000000, 0.000000000000000000 ) ) ;
#7732 = CARTESIAN_POINT ( 'NONE',  ( -28.13707043255157103, 18.96624908365847162, -12.83104814250460990 ) ) ;
#7733 = ORIENTED_EDGE ( 'NONE', *, *, #17158, .F. ) ;
#7734 = CARTESIAN_POINT ( 'NONE',  ( 1.831572820252008738, -45.77972211429909777, 137.7011124121615353 ) ) ;
#7736 = EDGE_CURVE ( 'NONE', #26, #24791, #23960, .T. ) ;
#7735 = CARTESIAN_POINT ( 'NONE',  ( 109.1592201516379674, -0.007051465909552739365, 0.003476928926134781935 ) ) ;
#7737 = CARTESIAN_POINT ( 'NONE',  ( 32.73300124599740002, 116.5274707358857142, -16.10546300444702794 ) ) ;
#7738 = ORIENTED_EDGE ( 'NONE', *, *, #16035, .T. ) ;
#7739 = CARTESIAN_POINT ( 'NONE',  ( -20.21097721650785672, 17.13687097598137399, -24.14932365326959030 ) ) ;
#7740 = EDGE_CURVE ( 'NONE', #26503, #21438, #933, .T. ) ;
#7741 = CARTESIAN_POINT ( 'NONE',  ( -4.178947244162641184, -47.46809051147732106, -11.88256963646720266 ) ) ;
#7742 = ORIENTED_EDGE ( 'NONE', *, *, #16485, .T. ) ;
#7743 = ORIENTED_EDGE ( 'NONE', *, *, #8006, .T. ) ;
#7744 = CARTESIAN_POINT ( 'NONE',  ( 5.340103556456579526, 140.9275371673313657, -43.36842540065345730 ) ) ;
#7745 = ORIENTED_EDGE ( 'NONE', *, *, #15758, .F. ) ;
#7746 = CARTESIAN_POINT ( 'NONE',  ( 21.16825799904893657, -63.85626241912828505, 119.4343305756978708 ) ) ;
#7747 = VERTEX_POINT ( 'NONE', #7578 ) ;
#7748 = PRODUCT_CONTEXT ( 'NONE', #19299, 'mechanical' ) ;
#7749 = CARTESIAN_POINT ( 'NONE',  ( 32.73300124599741423, 115.8010721414085822, -20.69176323058512423 ) ) ;
#7750 = MANIFOLD_SOLID_BREP ( 'Boss-Extrude1', #13255 ) ;
#7751 = CARTESIAN_POINT ( 'NONE',  ( 6.224689322667630975, -89.08920297664293741, 118.2566963816767753 ) ) ;
#7752 = B_SPLINE_CURVE_WITH_KNOTS ( 'NONE', 3,
 ( #5657, #26937, #14421, #7686 ),
 .UNSPECIFIED., .F., .F.,
 ( 4, 4 ),
 ( 1.895855152355442610E-16, 0.001982023823822945917 ),
 .UNSPECIFIED. ) ;
#7753 = CARTESIAN_POINT ( 'NONE',  ( 1.833485406944057594, -141.8265699653869376, 30.69200235378888308 ) ) ;
#7754 = ORIENTED_EDGE ( 'NONE', *, *, #20137, .F. ) ;
#7755 =( BOUNDED_SURFACE ( )  B_SPLINE_SURFACE ( 3, 1, ( 
 ( #13860, #7397 ),
 ( #16165, #3495 ),
 ( #21200, #5819 ),
 ( #5957, #16602 ) ),
 .UNSPECIFIED., .F., .F., .F. ) 
 B_SPLINE_SURFACE_WITH_KNOTS ( ( 4, 4 ),
 ( 2, 2 ),
 ( 0.000000000000000000, 1.000000000000000000 ),
 ( 0.000000000000000000, 1.000000000000000000 ),
 .UNSPECIFIED. ) 
 GEOMETRIC_REPRESENTATION_ITEM ( )  RATIONAL_B_SPLINE_SURFACE ( (
 ( 1.000000000000000000, 1.000000000000000000),
 ( 0.7789835883360576307, 0.9689951854195403280),
 ( 0.7789835883360576307, 0.9689951854195403280),
 ( 1.000000000000000000, 1.000000000000000000) ) ) 
 REPRESENTATION_ITEM ( '' )  SURFACE ( )  );
#7756 = EDGE_CURVE ( 'NONE', #10776, #26564, #5396, .T. ) ;
#7757 = CARTESIAN_POINT ( 'NONE',  ( 28.43349137099830770, -123.9292945876798200, -8.951033805645977282 ) ) ;
#7758 = CARTESIAN_POINT ( 'NONE',  ( -20.20612092514784663, 23.26073121129637045, -18.30568145913851907 ) ) ;
#7759 = ORIENTED_EDGE ( 'NONE', *, *, #27518, .T. ) ;
#7760 = VERTEX_POINT ( 'NONE', #12576 ) ;
#7761 = ORIENTED_EDGE ( 'NONE', *, *, #20345, .T. ) ;
#7762 = FACE_OUTER_BOUND ( 'NONE', #13726, .T. ) ;
#7763 = CARTESIAN_POINT ( 'NONE',  ( -25.21435515916043002, 34.05351380035335040, -6.169479169075572145 ) ) ;
#7765 = CARTESIAN_POINT ( 'NONE',  ( 24.01988960052047162, -121.3896480498354862, 49.36855864442090791 ) ) ;
#7764 = CARTESIAN_POINT ( 'NONE',  ( 1.833750490713671466, 108.0159692407144121, -96.89879583303743971 ) ) ;
#7766 = EDGE_CURVE ( 'NONE', #8983, #27304, #4645, .T. ) ;
#7767 = CARTESIAN_POINT ( 'NONE',  ( -20.57838717382308502, 27.96569011373086866, -10.78122205917010135 ) ) ;
#7768 = CARTESIAN_POINT ( 'NONE',  ( 24.22246935314087324, 90.00000000000005684, -40.00000000000000711 ) ) ;
#7769 = ORIENTED_EDGE ( 'NONE', *, *, #12024, .T. ) ;
#7770 = CARTESIAN_POINT ( 'NONE',  ( 10.93730112725932990, 151.0983828010088530, 4.928439153520527860 ) ) ;
#7771 = VECTOR ( 'NONE', #13523, 1000.000000000000114 ) ;
#7772 = EDGE_CURVE ( 'NONE', #9282, #238, #21364, .T. ) ;
#7773 = CARTESIAN_POINT ( 'NONE',  ( -1.583189561560256253, -36.01941156322767057, 29.24830400313204493 ) ) ;
#7774 = ORIENTED_EDGE ( 'NONE', *, *, #8545, .T. ) ;
#7775 = CARTESIAN_POINT ( 'NONE',  ( 0.000000000000000000, 0.000000000000000000, 0.000000000000000000 ) ) ;
#7776 = DIRECTION ( 'NONE',  ( 0.5914120900931444380, -0.1598001217819363939, -0.7903769105750348967 ) ) ;
#7777 = LINE ( 'NONE', #5890, #20254 ) ;
#7778 = CARTESIAN_POINT ( 'NONE',  ( 25.64681081121879203, -66.70335573067806934, -91.10197563708015878 ) ) ;
#7779 = CARTESIAN_POINT ( 'NONE',  ( -9.156249394959706578, 38.89149400288462033, 38.17928057391947760 ) ) ;
#7780 = CARTESIAN_POINT ( 'NONE',  ( -55.24390624410018802, 0.01027195578987812573, -0.001811362924359468263 ) ) ;
#7781 = CARTESIAN_POINT ( 'NONE',  ( 1.831572820252008738, -144.2101521542829232, -16.14965423926357246 ) ) ;
#7782 = EDGE_LOOP ( 'NONE', ( #2915, #11203, #28083, #3579 ) ) ;
#7783 = CARTESIAN_POINT ( 'NONE',  ( 109.1587776205901577, 0.007328861771496575708, 8.330235397647321066E-05 ) ) ;
#7784 = CARTESIAN_POINT ( 'NONE',  ( 1.833721034905659186, -30.51809396650913442, -141.8643653601973540 ) ) ;
#7785 = CARTESIAN_POINT ( 'NONE',  ( 1.831572820252008738, -86.09108691067849861, 116.8148281295966342 ) ) ;
#7786 = ORIENTED_EDGE ( 'NONE', *, *, #4747, .T. ) ;
#7787 = VERTEX_POINT ( 'NONE', #27845 ) ;
#7788 = CARTESIAN_POINT ( 'NONE',  ( -4.780792508754312387, -18.84172549606840619, 45.80716263181253822 ) ) ;
#7789 = CARTESIAN_POINT ( 'NONE',  ( 25.98552792386798771, -102.9121737515624062, 47.00040718953741248 ) ) ;
#7790 = FILL_AREA_STYLE ('',( #18567 ) ) ;
#7791 = EDGE_CURVE ( 'NONE', #4553, #27587, #14455, .T. ) ;
#7792 = CARTESIAN_POINT ( 'NONE',  ( 109.1586900883932856, -0.007109207791180745251, -0.0006456433529069797875 ) ) ;
#7793 = LINE ( 'NONE', #27781, #7600 ) ;
#7794 = CARTESIAN_POINT ( 'NONE',  ( 26.11404676487259024, 74.91683232331092768, -84.89295829319416953 ) ) ;
#7795 = CARTESIAN_POINT ( 'NONE',  ( -55.25719721206881729, 0.006045473558784871665, -0.009391134844733287426 ) ) ;
#7796 = EDGE_CURVE ( 'NONE', #7039, #12676, #5284, .T. ) ;
#7797 = CARTESIAN_POINT ( 'NONE',  ( -20.47566262905009538, -27.87687924095555658, -10.72601569609885708 ) ) ;
#7798 = VERTEX_POINT ( 'NONE', #14736 ) ;
#7799 =( BOUNDED_SURFACE ( )  B_SPLINE_SURFACE ( 3, 1, ( 
 ( #25431, #14318 ),
 ( #16920, #7734 ),
 ( #25280, #10323 ),
 ( #7878, #14890 ) ),
 .UNSPECIFIED., .F., .F., .F. ) 
 B_SPLINE_SURFACE_WITH_KNOTS ( ( 4, 4 ),
 ( 2, 2 ),
 ( 0.000000000000000000, 1.000000000000000000 ),
 ( 0.000000000000000000, 1.000000000000000000 ),
 .UNSPECIFIED. ) 
 GEOMETRIC_REPRESENTATION_ITEM ( )  RATIONAL_B_SPLINE_SURFACE ( (
 ( 1.000000000000000000, 1.000000000000000000),
 ( 0.9956975270656955868, 0.8568959468854907557),
 ( 0.9956975270656955868, 0.8568959468854907557),
 ( 1.000000000000000000, 1.000000000000000000) ) ) 
 REPRESENTATION_ITEM ( '' )  SURFACE ( )  );
#7800 = EDGE_CURVE ( 'NONE', #21937, #13776, #27967, .T. ) ;
#7801 = ORIENTED_EDGE ( 'NONE', *, *, #21904, .T. ) ;
#7802 = CARTESIAN_POINT ( 'NONE',  ( 109.1721716018069657, -0.01157047143379290842, -0.01254847260354823371 ) ) ;
#7803 = CARTESIAN_POINT ( 'NONE',  ( -1.031422197589711987, -45.78027046666441890, 1.530725436377941673 ) ) ;
#7804 = DIRECTION ( 'NONE',  ( 0.5914120900931444380, -0.2567974902965192152, 0.7643865440136080602 ) ) ;
#7805 = CARTESIAN_POINT ( 'NONE',  ( 28.37599760073043242, 25.60640155549320340, -111.8383885143452687 ) ) ;
#7806 = FACE_OUTER_BOUND ( 'NONE', #18042, .T. ) ;
#7807 = CARTESIAN_POINT ( 'NONE',  ( -1.045287976400365970, -45.76855895860942525, 1.530335034934587002 ) ) ;
#7808 = VERTEX_POINT ( 'NONE', #23542 ) ;
#7809 = CARTESIAN_POINT ( 'NONE',  ( 109.1589550718174877, -0.007270618150629046088, 0.002126635388725444178 ) ) ;
#7810 = DIRECTION ( 'NONE',  ( 0.000000000000000000, 0.000000000000000000, 1.000000000000000000 ) ) ;
#7811 = CARTESIAN_POINT ( 'NONE',  ( 1.831572820252009626, -96.36280042116003131, 108.4969585352551746 ) ) ;
#7812 = CARTESIAN_POINT ( 'NONE',  ( -20.37983603106074071, -16.25728007463423808, -24.94323704205431369 ) ) ;
#7813 = CARTESIAN_POINT ( 'NONE',  ( 2.430230287190589422, 1.451610819317738610, 145.5073573687466819 ) ) ;
#7814 = ORIENTED_EDGE ( 'NONE', *, *, #26289, .F. ) ;
#7815 = CARTESIAN_POINT ( 'NONE',  ( 109.1586900883932856, 0.006960773163856032002, 0.001582822706024274422 ) ) ;
#7817 = CARTESIAN_POINT ( 'NONE',  ( -1.155031165708871654, -28.62780465193337420, -35.88345263711039479 ) ) ;
#7816 = B_SPLINE_CURVE_WITH_KNOTS ( 'NONE', 3,
 ( #22948, #3205, #1052, #18609 ),
 .UNSPECIFIED., .F., .F.,
 ( 4, 4 ),
 ( 0.000000000000000000, 0.01077107196513873814 ),
 .UNSPECIFIED. ) ;
#7818 = ORIENTED_EDGE ( 'NONE', *, *, #17505, .T. ) ;
#7819 = VERTEX_POINT ( 'NONE', #25270 ) ;
#7820 = ORIENTED_EDGE ( 'NONE', *, *, #23817, .T. ) ;
#7821 = CARTESIAN_POINT ( 'NONE',  ( -21.41430102051752016, -16.60879216503617073, 25.94791611261633690 ) ) ;
#7822 = FACE_OUTER_BOUND ( 'NONE', #8539, .T. ) ;
#7823 = EDGE_CURVE ( 'NONE', #1130, #23219, #16299, .T. ) ;
#7824 = EDGE_CURVE ( 'NONE', #25988, #13553, #22108, .T. ) ;
#7825 = CARTESIAN_POINT ( 'NONE',  ( 109.1778270068192853, -0.009307953841262541286, -0.0003511581237570729095 ) ) ;
#7826 = CARTESIAN_POINT ( 'NONE',  ( -28.13707043255157103, 18.06394523322453693, -14.07296284901339334 ) ) ;
#7827 = CARTESIAN_POINT ( 'NONE',  ( -20.21097721650786738, 17.67178726257392896, 23.76068422213738529 ) ) ;
#7828 = ORIENTED_EDGE ( 'NONE', *, *, #8248, .F. ) ;
#7829 = EDGE_CURVE ( 'NONE', #8890, #28211, #4622, .T. ) ;
#7830 = CARTESIAN_POINT ( 'NONE',  ( -25.21435515916025594, 1.749597353048488237E-16, -4.373993382621220594E-17 ) ) ;
#7831 = CARTESIAN_POINT ( 'NONE',  ( 25.64708228042119131, 83.88307475436060656, 75.58165863986067734 ) ) ;
#7832 = B_SPLINE_CURVE_WITH_KNOTS ( 'NONE', 3,
 ( #8837, #17036, #26381, #24103, #4366, #25833, #21793, #6534 ),
 .UNSPECIFIED., .F., .F.,
 ( 4, 2, 2, 4 ),
 ( 6.505213034913026604E-19, 0.0002429592666046762994, 0.0004859185332093519482, 0.0009718370664186838388 ),
 .UNSPECIFIED. ) ;
#7833 = CARTESIAN_POINT ( 'NONE',  ( 1.833485406944043827, 132.3460930279890704, 59.50871042846269177 ) ) ;
#7834 = EDGE_CURVE ( 'NONE', #12622, #11774, #15559, .T. ) ;
#7835 = LINE ( 'NONE', #18299, #19449 ) ;
#7836 = CARTESIAN_POINT ( 'NONE',  ( 10.93730112726002979, 79.81734490846109509, -128.3908183996583432 ) ) ;
#7837 = CARTESIAN_POINT ( 'NONE',  ( 10.93730112725932813, 146.7718404940640085, 36.23586118136551448 ) ) ;
#7838 = CARTESIAN_POINT ( 'NONE',  ( 25.64704443564076186, -66.25951665433227333, -91.42548471394263743 ) ) ;
#7839 = CARTESIAN_POINT ( 'NONE',  ( 25.98552792386800192, 76.50165414343565828, 83.35136888841265090 ) ) ;
#7840 = FACE_OUTER_BOUND ( 'NONE', #20865, .T. ) ;
#7841 = CARTESIAN_POINT ( 'NONE',  ( -28.13707043255157103, -22.88591869784690402, 0.7675454997509406629 ) ) ;
#7842 = CARTESIAN_POINT ( 'NONE',  ( -8.259864102781673267, -25.58601832199047266, 46.42816643551597622 ) ) ;
#7843 =( BOUNDED_SURFACE ( )  B_SPLINE_SURFACE ( 3, 1, ( 
 ( #24448, #26580 ),
 ( #6884, #4717 ),
 ( #13491, #22286 ),
 ( #20107, #12054 ) ),
 .UNSPECIFIED., .F., .F., .F. ) 
 B_SPLINE_SURFACE_WITH_KNOTS ( ( 4, 4 ),
 ( 2, 2 ),
 ( 0.000000000000000000, 1.000000000000000000 ),
 ( 0.000000000000000000, 1.000000000000000000 ),
 .UNSPECIFIED. ) 
 GEOMETRIC_REPRESENTATION_ITEM ( )  RATIONAL_B_SPLINE_SURFACE ( (
 ( 1.000000000000000000, 1.000000000000000000),
 ( 0.9960225298536222738, 0.9999952330161893110),
 ( 0.9960225298536222738, 0.9999952330161893110),
 ( 1.000000000000000000, 1.000000000000000000) ) ) 
 REPRESENTATION_ITEM ( '' )  SURFACE ( )  );
#7844 = ORIENTED_EDGE ( 'NONE', *, *, #27085, .F. ) ;
#7845 = CARTESIAN_POINT ( 'NONE',  ( 55.79472521941428198, -49.22042574086388811, -53.57698701322264867 ) ) ;
#7846 = VERTEX_POINT ( 'NONE', #298 ) ;
#7847 = CARTESIAN_POINT ( 'NONE',  ( 26.11404676487259024, -108.0249973236465308, -33.91085499298486639 ) ) ;
#7848 = DIRECTION ( 'NONE',  ( 0.5946245182733608248, 0.7858154137795708705, 0.1700465163848279837 ) ) ;
#7849 = EDGE_LOOP ( 'NONE', ( #15780, #18437 ) ) ;
#7850 = VECTOR ( 'NONE', #10777, 1000.000000000000114 ) ;
#7851 = ORIENTED_EDGE ( 'NONE', *, *, #21511, .F. ) ;
#7852 = ORIENTED_EDGE ( 'NONE', *, *, #11184, .T. ) ;
#7853 = CARTESIAN_POINT ( 'NONE',  ( 2.433796855181233454, 138.8296532063088193, 43.58222566461690661 ) ) ;
#7854 = EDGE_CURVE ( 'NONE', #9726, #18571, #6259, .T. ) ;
#7855 = CARTESIAN_POINT ( 'NONE',  ( -1.583189561560256253, -43.29471907393730135, 16.68617981233747827 ) ) ;
#7856 = CARTESIAN_POINT ( 'NONE',  ( 32.73300124599737870, -117.5726003567929041, -3.836798148480059734 ) ) ;
#7857 = EDGE_CURVE ( 'NONE', #25030, #1343, #25897, .T. ) ;
#7858 = CARTESIAN_POINT ( 'NONE',  ( 109.1778270068192853, 0.009031542838317254199, 0.002278716897421661797 ) ) ;
#7859 = CIRCLE ( 'NONE', #5533, 37.50000000000001421 ) ;
#7860 = B_SPLINE_CURVE_WITH_KNOTS ( 'NONE', 3,
 ( #13403, #6959, #18005, #26790, #22203, #24673 ),
 .UNSPECIFIED., .F., .F.,
 ( 4, 2, 4 ),
 ( 0.000000000000000000, 0.0004335184443140181732, 0.0008670368886280363464 ),
 .UNSPECIFIED. ) ;
#7861 = CARTESIAN_POINT ( 'NONE',  ( 1.832998868059858122, 85.72499093308256590, -117.0819875546686859 ) ) ;
#7862 = CONICAL_SURFACE ( 'NONE', #10157, 34.60786435723138510, 0.8559913436420825139 ) ;
#7863 = B_SPLINE_CURVE_WITH_KNOTS ( 'NONE', 3,
 ( #283, #26337, #28345, #24336, #21889, #2581 ),
 .UNSPECIFIED., .F., .F.,
 ( 4, 2, 4 ),
 ( 0.000000000000000000, 0.0004335151646191513579, 0.0008670303292383027159 ),
 .UNSPECIFIED. ) ;
#7864 = CARTESIAN_POINT ( 'NONE',  ( 2.433796855181205476, -116.8607839509050734, -86.69855925934092511 ) ) ;
#7866 = DIRECTION ( 'NONE',  ( 1.000000000000000000, -6.938893903907226837E-18, 1.734723475976806709E-18 ) ) ;
#7865 = CARTESIAN_POINT ( 'NONE',  ( -1.044556982611269058, -44.03203163107536966, -12.57890920527759171 ) ) ;
#7867 = CARTESIAN_POINT ( 'NONE',  ( 1.833485406944043827, 132.7804117027896211, -58.53321471326746916 ) ) ;
#7868 = CIRCLE ( 'NONE', #23506, 151.1787379149930359 ) ;
#7869 = ORIENTED_EDGE ( 'NONE', *, *, #5493, .F. ) ;
#7870 = ORIENTED_EDGE ( 'NONE', *, *, #14371, .F. ) ;
#7871 = CARTESIAN_POINT ( 'NONE',  ( 1.833485406944043827, 108.1939177044938560, -96.69979900902059455 ) ) ;
#7873 = CARTESIAN_POINT ( 'NONE',  ( -1.155001620486246994, 25.28075036143276932, 38.31519699443472859 ) ) ;
#7872 = CARTESIAN_POINT ( 'NONE',  ( 1.833206308920110050, 132.8652726225759864, -58.34024961171099477 ) ) ;
#7874 = CARTESIAN_POINT ( 'NONE',  ( -20.47566262905010603, -7.708089517695397852, -28.85746289809576126 ) ) ;
#7875 = CARTESIAN_POINT ( 'NONE',  ( 25.64681081121879203, 75.86069728268988399, 83.63051021305928145 ) ) ;
#7876 = EDGE_LOOP ( 'NONE', ( #260, #11669, #5776, #24977 ) ) ;
#7877 = VERTEX_POINT ( 'NONE', #11243 ) ;
#7878 = CARTESIAN_POINT ( 'NONE',  ( 109.1592201516379674, -0.001934867487021774525, -0.007620268632971101234 ) ) ;
#7879 =( BOUNDED_SURFACE ( )  B_SPLINE_SURFACE ( 3, 1, ( 
 ( #26755, #13104 ),
 ( #19713, #11090 ),
 ( #19860, #147 ),
 ( #8941, #7069 ) ),
 .UNSPECIFIED., .F., .F., .F. ) 
 B_SPLINE_SURFACE_WITH_KNOTS ( ( 4, 4 ),
 ( 2, 2 ),
 ( 0.000000000000000000, 1.000000000000000000 ),
 ( 0.000000000000000000, 1.000000000000000000 ),
 .UNSPECIFIED. ) 
 GEOMETRIC_REPRESENTATION_ITEM ( )  RATIONAL_B_SPLINE_SURFACE ( (
 ( 1.000000000000000000, 1.000000000000000000),
 ( 0.9593753223639863714, 0.9995975284513187731),
 ( 0.9593753223639863714, 0.9995975284513187731),
 ( 1.000000000000000000, 1.000000000000000000) ) ) 
 REPRESENTATION_ITEM ( '' )  SURFACE ( )  );
#7880 = CARTESIAN_POINT ( 'NONE',  ( 13.36082413113061307, 41.18148072373615776, 147.2768864064169350 ) ) ;
#7881 = CARTESIAN_POINT ( 'NONE',  ( 13.84597867724968268, -142.4258194868991723, -35.16314962059988858 ) ) ;
#7882 = ORIENTED_EDGE ( 'NONE', *, *, #14620, .T. ) ;
#7883 = CARTESIAN_POINT ( 'NONE',  ( 109.1592201516379674, 0.005631912476303814301, -0.005485778713202952607 ) ) ;
#7884 = CARTESIAN_POINT ( 'NONE',  ( -1.464342487929844783, -38.76467504336602588, -25.15873223207679743 ) ) ;
#7885 = ORIENTED_EDGE ( 'NONE', *, *, #7381, .F. ) ;
#7886 = ORIENTED_EDGE ( 'NONE', *, *, #15924, .F. ) ;
#7887 = CIRCLE ( 'NONE', #11990, 34.60786435723138510 ) ;
#7888 =( GEOMETRIC_REPRESENTATION_CONTEXT ( 3 ) GLOBAL_UNCERTAINTY_ASSIGNED_CONTEXT ( ( #22940 ) ) GLOBAL_UNIT_ASSIGNED_CONTEXT ( ( #12714, #8142, #12433 ) ) REPRESENTATION_CONTEXT ( 'NONE', 'WORKASPACE' ) );
#7889 = LINE ( 'NONE', #14475, #13324 ) ;
#7890 = VECTOR ( 'NONE', #14877, 1000.000000000000000 ) ;
#7891 = ORIENTED_EDGE ( 'NONE', *, *, #748, .T. ) ;
#7892 = CARTESIAN_POINT ( 'NONE',  ( -1.058197053496171769, -42.99116279335166269, -15.81317659443667445 ) ) ;
#7893 = CARTESIAN_POINT ( 'NONE',  ( -1.019300379054419725, 16.06793277092052818, 42.90269154183410194 ) ) ;
#7894 = EDGE_CURVE ( 'NONE', #5142, #4901, #163, .T. ) ;
#7895 = CARTESIAN_POINT ( 'NONE',  ( 1.831572820252009626, 58.11906524360657755, -132.9644823688589668 ) ) ;
#7896 = EDGE_CURVE ( 'NONE', #5184, #17451, #2451, .T. ) ;
#7897 = FACE_OUTER_BOUND ( 'NONE', #17314, .T. ) ;
#7898 = CARTESIAN_POINT ( 'NONE',  ( 109.1592201516379674, 0.007845213074654433863, -0.0005146241775983094154 ) ) ;
#7899 = CARTESIAN_POINT ( 'NONE',  ( 10.93730112725932990, 151.0983828010088530, 4.928439153520527860 ) ) ;
#7900 = CARTESIAN_POINT ( 'NONE',  ( 109.1587776205901577, 0.0008489206734408877688, -0.007280006032833121095 ) ) ;
#7901 = ADVANCED_FACE ( 'NONE', ( #19873 ), #21936, .F. ) ;
#7902 = ORIENTED_EDGE ( 'NONE', *, *, #24311, .T. ) ;
#7903 = CARTESIAN_POINT ( 'NONE',  ( 16.05277956358206737, -4.672229451526818345, -143.2298391883442150 ) ) ;
#7905 = CARTESIAN_POINT ( 'NONE',  ( 9.884929003653626367, -141.8132360130361178, 50.49804566712076337 ) ) ;
#7904 = CARTESIAN_POINT ( 'NONE',  ( 28.43349137099852086, 94.99961975860237828, 80.08535015163919013 ) ) ;
#7906 = CARTESIAN_POINT ( 'NONE',  ( -20.38016308990357572, -1.509191766064412299, -29.73560196176845238 ) ) ;
#7907 = ORIENTED_EDGE ( 'NONE', *, *, #15140, .T. ) ;
#7908 = AXIS2_PLACEMENT_3D ( 'NONE', #7640, #14370, #18699 ) ;
#7909 = ORIENTED_EDGE ( 'NONE', *, *, #16448, .T. ) ;
#7910 = ORIENTED_EDGE ( 'NONE', *, *, #16347, .F. ) ;
#7911 = CARTESIAN_POINT ( 'NONE',  ( -55.24390624410018802, -0.004572280736701530256, -0.009374879212970928244 ) ) ;
#7912 = DIRECTION ( 'NONE',  ( -1.000000000000000000, -0.000000000000000000, -0.000000000000000000 ) ) ;
#7914 = CARTESIAN_POINT ( 'NONE',  ( -20.20700224038492010, 18.19058640100223556, -23.35150625415664649 ) ) ;
#7913 = CARTESIAN_POINT ( 'NONE',  ( 32.73300124599735028, 8.473903470906103408, 117.3295799645430151 ) ) ;
#7915 = CIRCLE ( 'NONE', #22064, 53.53553390275978785 ) ;
#7916 = CARTESIAN_POINT ( 'NONE',  ( -1.048996300304501972, -43.31387123529967909, 14.87787369922214076 ) ) ;
#7917 = CARTESIAN_POINT ( 'NONE',  ( -1.113548883309547044, -12.28732181966548609, -44.18588492042589166 ) ) ;
#7918 = CARTESIAN_POINT ( 'NONE',  ( 26.11404676487257603, 47.08215554553518700, 102.9690087468803341 ) ) ;
#7919 = CARTESIAN_POINT ( 'NONE',  ( -12.82751273423883553, -43.04932478553545394, -23.15139349681293623 ) ) ;
#7920 = VERTEX_POINT ( 'NONE', #15847 ) ;
#7921 = CARTESIAN_POINT ( 'NONE',  ( 109.1721716018069657, 0.008708654716139420035, 0.01467989464939313364 ) ) ;
#7922 = CARTESIAN_POINT ( 'NONE',  ( -55.24271866751342941, 0.004365563123935787236, 0.008433070970613791573 ) ) ;
#7923 = AXIS2_PLACEMENT_3D ( 'NONE', #5484, #27206, #5194 ) ;
#7924 = CARTESIAN_POINT ( 'NONE',  ( 30.59141879584315760, 38.47120193631630514, -109.6600586137411995 ) ) ;
#7925 = CARTESIAN_POINT ( 'NONE',  ( 26.11404676487257603, 84.89295829319590325, -74.91683232330889552 ) ) ;
#7926 = DIRECTION ( 'NONE',  ( 0.000000000000000000, 0.000000000000000000, 1.000000000000000000 ) ) ;
#7927 = CARTESIAN_POINT ( 'NONE',  ( -18.41936578851709783, -20.09935324538221479, -37.37524689996187277 ) ) ;
#7928 = CARTESIAN_POINT ( 'NONE',  ( 2.430230287190581429, -144.5585181921884725, -16.65331920325886728 ) ) ;
#7929 = ORIENTED_EDGE ( 'NONE', *, *, #19681, .T. ) ;
#7930 = CARTESIAN_POINT ( 'NONE',  ( 19.66333377628711432, 60.10102584214535426, -123.9466021833765268 ) ) ;
#7931 = CARTESIAN_POINT ( 'NONE',  ( 109.1624594426973260, 0.01595733256931100227, 0.0004639210235576350151 ) ) ;
#7932 = CARTESIAN_POINT ( 'NONE',  ( 9.884929003653626367, 119.2676479132386191, -91.84919534721818479 ) ) ;
#7933 = ORIENTED_EDGE ( 'NONE', *, *, #7235, .T. ) ;
#7934 = ADVANCED_FACE ( 'NONE', ( #9387 ), #7406, .F. ) ;
#7935 = CARTESIAN_POINT ( 'NONE',  ( -1.323830074806760848, -2.318057800980394045, 46.01435746200695576 ) ) ;
#7936 = VERTEX_POINT ( 'NONE', #11382 ) ;
#7937 = EDGE_CURVE ( 'NONE', #25105, #15925, #25236, .T. ) ;
#7938 =( BOUNDED_SURFACE ( )  B_SPLINE_SURFACE ( 3, 1, ( 
 ( #98, #6309 ),
 ( #8891, #15343 ),
 ( #15057, #11320 ),
 ( #6445, #13185 ) ),
 .UNSPECIFIED., .F., .F., .F. ) 
 B_SPLINE_SURFACE_WITH_KNOTS ( ( 4, 4 ),
 ( 2, 2 ),
 ( 0.000000000000000000, 1.000000000000000000 ),
 ( 0.000000000000000000, 1.000000000000000000 ),
 .UNSPECIFIED. ) 
 GEOMETRIC_REPRESENTATION_ITEM ( )  RATIONAL_B_SPLINE_SURFACE ( (
 ( 1.000000000000000000, 1.000000000000000000),
 ( 0.9934239774497837239, 0.8357310067453919133),
 ( 0.9934239774497837239, 0.8357310067453919133),
 ( 1.000000000000000000, 1.000000000000000000) ) ) 
 REPRESENTATION_ITEM ( '' )  SURFACE ( )  );
#7939 = DIRECTION ( 'NONE',  ( 0.7637818620346801257, 0.1788995134688915190, 0.6201872550346635427 ) ) ;
#7940 = EDGE_CURVE ( 'NONE', #17492, #1901, #19354, .T. ) ;
#7941 = CARTESIAN_POINT ( 'NONE',  ( -20.57838717382308147, 1.611677988432361097, -29.92853265176831812 ) ) ;
#7942 = CIRCLE ( 'NONE', #27209, 151.1787379149930359 ) ;
#7943 = CARTESIAN_POINT ( 'NONE',  ( 109.1586059443104944, -0.006971743774738792081, 0.001198897580748315740 ) ) ;
#7944 = CARTESIAN_POINT ( 'NONE',  ( 1.832998868059890096, 30.69214149074013420, 141.8272129421609691 ) ) ;
#7945 = CARTESIAN_POINT ( 'NONE',  ( 109.1586900883932856, -0.007002774699553650055, 0.001385221016536923372 ) ) ;
#7946 = DIRECTION ( 'NONE',  ( -0.5946245182733607137, -0.7655593692108988435, -0.2456431038754887941 ) ) ;
#7947 = CARTESIAN_POINT ( 'NONE',  ( -1.045287976400362417, -15.59869763335038506, 43.05558670614261985 ) ) ;
#7948 = DIRECTION ( 'NONE',  ( 0.5914120900931444380, -0.3206367055789438592, -0.7398809652418016913 ) ) ;
#7949 = ORIENTED_EDGE ( 'NONE', *, *, #6840, .F. ) ;
#7950 = ORIENTED_EDGE ( 'NONE', *, *, #28360, .F. ) ;
#7951 = CARTESIAN_POINT ( 'NONE',  ( 2.263178113027037863, 107.1074314657344644, 98.32595894905868761 ) ) ;
#7952 = DIRECTION ( 'NONE',  ( -1.000000000000000000, -0.000000000000000000, -0.000000000000000000 ) ) ;
#7953 = LINE ( 'NONE', #16981, #14258 ) ;
#7954 = B_SPLINE_CURVE_WITH_KNOTS ( 'NONE', 3,
 ( #27872, #8170, #16934, #12879, #8444, #16808, #14904, #18807 ),
 .UNSPECIFIED., .F., .F.,
 ( 4, 2, 2, 4 ),
 ( 3.469446951953614189E-18, 0.0002429592666046796875, 0.0004859185332093559056, 0.0009718370664186904524 ),
 .UNSPECIFIED. ) ;
#7955 = CARTESIAN_POINT ( 'NONE',  ( 2.263178607246671969, 107.1074316126230883, -98.32595927618747567 ) ) ;
#7956 = FACE_OUTER_BOUND ( 'NONE', #6524, .T. ) ;
#7957 = CARTESIAN_POINT ( 'NONE',  ( 55.49584447822657296, -48.34726110740022875, 54.09506550945609149 ) ) ;
#7958 = ORIENTED_EDGE ( 'NONE', *, *, #17862, .T. ) ;
#7959 = CARTESIAN_POINT ( 'NONE',  ( 0.000000000000000000, 0.000000000000000000, 0.000000000000000000 ) ) ;
#7960 = CARTESIAN_POINT ( 'NONE',  ( -1.045287976400365970, -37.92705037016778391, -25.66401692419976399 ) ) ;
#7961 = CARTESIAN_POINT ( 'NONE',  ( 26.11404676487257603, 1.130420376097130086, 113.2169081140374090 ) ) ;
#7962 = AXIS2_PLACEMENT_3D ( 'NONE', #3542, #12464, #25585 ) ;
#7963 = CARTESIAN_POINT ( 'NONE',  ( 1.831572820252009626, 0.9871191512914618826, 145.1082523917587253 ) ) ;
#7964 = AXIS2_PLACEMENT_3D ( 'NONE', #16314, #16461, #25253 ) ;
#7965 = EDGE_LOOP ( 'NONE', ( #14229, #28188, #18318, #4866 ) ) ;
#7966 = CARTESIAN_POINT ( 'NONE',  ( -1.619063947482201282, 38.92136151114908671, -25.20140673341387227 ) ) ;
#7967 = CARTESIAN_POINT ( 'NONE',  ( 28.37644542392836655, 109.6517504963498340, -58.62516076109932328 ) ) ;
#7968 = ORIENTED_EDGE ( 'NONE', *, *, #6932, .T. ) ;
#7969 = VERTEX_POINT ( 'NONE', #8417 ) ;
#7970 = EDGE_CURVE ( 'NONE', #3139, #142, #26916, .T. ) ;
#7971 = ORIENTED_EDGE ( 'NONE', *, *, #6778, .F. ) ;
#7972 = EDGE_CURVE ( 'NONE', #13800, #25441, #15197, .T. ) ;
#7973 = ADVANCED_FACE ( 'NONE', ( #24790 ), #20239, .F. ) ;
#7974 = CARTESIAN_POINT ( 'NONE',  ( 109.1586059443104944, -0.0004635842312796545654, 0.007058870754606100771 ) ) ;
#7975 =( BOUNDED_SURFACE ( )  B_SPLINE_SURFACE ( 3, 1, ( 
 ( #15337, #4129 ),
 ( #12899, #1963 ),
 ( #2097, #10767 ),
 ( #17358, #26149 ) ),
 .UNSPECIFIED., .F., .F., .F. ) 
 B_SPLINE_SURFACE_WITH_KNOTS ( ( 4, 4 ),
 ( 2, 2 ),
 ( 0.000000000000000000, 1.000000000000000000 ),
 ( 0.000000000000000000, 1.000000000000000000 ),
 .UNSPECIFIED. ) 
 GEOMETRIC_REPRESENTATION_ITEM ( )  RATIONAL_B_SPLINE_SURFACE ( (
 ( 1.000000000000000000, 1.000000000000000000),
 ( 0.9934239774497837239, 0.8357310067453919133),
 ( 0.9934239774497837239, 0.8357310067453919133),
 ( 1.000000000000000000, 1.000000000000000000) ) ) 
 REPRESENTATION_ITEM ( '' )  SURFACE ( )  );
#7976 = UNCERTAINTY_MEASURE_WITH_UNIT (LENGTH_MEASURE( 1.000000000000000082E-05 ), #7605, 'distance_accuracy_value', 'NONE');
#7977 = FACE_OUTER_BOUND ( 'NONE', #16191, .T. ) ;
#7978 = VECTOR ( 'NONE', #21538, 1000.000000000000227 ) ;
#7979 = AXIS2_PLACEMENT_3D ( 'NONE', #25617, #14364, #27467 ) ;
#7980 = CARTESIAN_POINT ( 'NONE',  ( 109.1586900883932856, -0.006561743627143347760, 0.002810909342011576936 ) ) ;
#7981 = ORIENTED_EDGE ( 'NONE', *, *, #24702, .T. ) ;
#7982 = DIRECTION ( 'NONE',  ( -1.000000000000000000, -0.000000000000000000, -0.000000000000000000 ) ) ;
#7983 = CARTESIAN_POINT ( 'NONE',  ( 13.36082413113061307, -109.3026516754225099, -106.9547846563646800 ) ) ;
#7984 = B_SPLINE_CURVE_WITH_KNOTS ( 'NONE', 3,
 ( #20760, #27079, #5070, #3488, #11706, #7691, #16592 ),
 .UNSPECIFIED., .F., .F.,
 ( 4, 3, 4 ),
 ( 0.000000000000000000, 0.006568092053401780595, 0.02506242213020846640 ),
 .UNSPECIFIED. ) ;
#7985 = EDGE_CURVE ( 'NONE', #4018, #23277, #10815, .T. ) ;
#7986 = CARTESIAN_POINT ( 'NONE',  ( 1.833750490713684345, -85.07723081767805695, -117.5529286802296411 ) ) ;
#7987 = CARTESIAN_POINT ( 'NONE',  ( 28.43349137099838941, 42.22940898499208373, 116.8557575815928971 ) ) ;
#7988 = CARTESIAN_POINT ( 'NONE',  ( 2.430230287190572103, 126.7388733285354760, -71.49654683843375835 ) ) ;
#7989 = CARTESIAN_POINT ( 'NONE',  ( -1.463510566862832096, 35.90603835816546763, 29.09194585123793786 ) ) ;
#7990 = CARTESIAN_POINT ( 'NONE',  ( 25.64707127832795663, -0.04959866882938956945, -112.9112343549835487 ) ) ;
#7991 = VECTOR ( 'NONE', #12997, 1000.000000000000000 ) ;
#7992 = CARTESIAN_POINT ( 'NONE',  ( 32.73300124599735028, 110.6325518752274206, 39.98094346392350218 ) ) ;
#7993 = CARTESIAN_POINT ( 'NONE',  ( 30.58324630866339433, -119.0579156359857507, -21.27395054437367605 ) ) ;
#7994 = ORIENTED_EDGE ( 'NONE', *, *, #4213, .F. ) ;
#7995 = CARTESIAN_POINT ( 'NONE',  ( -1.323439229708136100, 25.17120723334093313, -38.58845475799776636 ) ) ;
#7996 = EDGE_CURVE ( 'NONE', #24633, #14412, #6318, .T. ) ;
#7997 = ORIENTED_EDGE ( 'NONE', *, *, #12451, .F. ) ;
#7998 = FACE_OUTER_BOUND ( 'NONE', #97, .T. ) ;
#7999 = DIRECTION ( 'NONE',  ( 0.000000000000000000, 5.223019709707975211E-21, -1.000000000000000000 ) ) ;
#8000 = VERTEX_POINT ( 'NONE', #16422 ) ;
#8001 = ADVANCED_FACE ( 'NONE', ( #7806 ), #23975, .F. ) ;
#8002 = ORIENTED_EDGE ( 'NONE', *, *, #23885, .F. ) ;
#8003 = AXIS2_PLACEMENT_3D ( 'NONE', #27161, #16231, #27452 ) ;
#8004 = VERTEX_POINT ( 'NONE', #11821 ) ;
#8005 = EDGE_CURVE ( 'NONE', #19578, #25057, #1869, .T. ) ;
#8006 = EDGE_CURVE ( 'NONE', #12467, #13110, #27494, .T. ) ;
#8007 = B_SPLINE_CURVE_WITH_KNOTS ( 'NONE', 3,
 ( #11647, #20421, #13792, #4737, #18112, #22157 ),
 .UNSPECIFIED., .F., .F.,
 ( 4, 2, 4 ),
 ( 1.389302603484999005E-17, 0.0006311571484586076322, 0.001262314296917201603 ),
 .UNSPECIFIED. ) ;
#8008 = CARTESIAN_POINT ( 'NONE',  ( 1.833750490713684345, -141.9939712933757221, 29.90883416717569787 ) ) ;
#8009 = CARTESIAN_POINT ( 'NONE',  ( -22.23226125620929494, -30.68305173820431619, -7.677408153693907167 ) ) ;
#8010 = CARTESIAN_POINT ( 'NONE',  ( -20.20898968516257810, 0.6607166829023055632, 29.59696826051171925 ) ) ;
#8011 =( BOUNDED_SURFACE ( )  B_SPLINE_SURFACE ( 3, 1, ( 
 ( #13123, #14865 ),
 ( #10425, #25687 ),
 ( #23944, #19315 ),
 ( #21772, #2035 ) ),
 .UNSPECIFIED., .F., .F., .F. ) 
 B_SPLINE_SURFACE_WITH_KNOTS ( ( 4, 4 ),
 ( 2, 2 ),
 ( 0.000000000000000000, 1.000000000000000000 ),
 ( 0.000000000000000000, 1.000000000000000000 ),
 .UNSPECIFIED. ) 
 GEOMETRIC_REPRESENTATION_ITEM ( )  RATIONAL_B_SPLINE_SURFACE ( (
 ( 1.000000000000000000, 1.000000000000000000),
 ( 0.9960225298536222738, 0.9999952330161893110),
 ( 0.9960225298536222738, 0.9999952330161893110),
 ( 1.000000000000000000, 1.000000000000000000) ) ) 
 REPRESENTATION_ITEM ( '' )  SURFACE ( )  );
#8012 = LINE ( 'NONE', #9721, #26344 ) ;
#8013 = CARTESIAN_POINT ( 'NONE',  ( 25.64699802086726166, 56.66140964017734660, 97.66487797954027883 ) ) ;
#8014 = ORIENTED_EDGE ( 'NONE', *, *, #17510, .F. ) ;
#8015 = ORIENTED_EDGE ( 'NONE', *, *, #16587, .T. ) ;
#8016 = CARTESIAN_POINT ( 'NONE',  ( 109.1592201516379674, 0.004194960840990064228, 0.006649399203953477652 ) ) ;
#8018 = LINE ( 'NONE', #2056, #11892 ) ;
#8017 = CARTESIAN_POINT ( 'NONE',  ( -1.044556982611270612, 28.22896456560720679, 36.05793013899066324 ) ) ;
#8019 = CARTESIAN_POINT ( 'NONE',  ( -25.21435515916025594, 1.749597353048488237E-16, -4.373993382621220594E-17 ) ) ;
#8020 = CARTESIAN_POINT ( 'NONE',  ( 10.93730112725990367, -84.82621002473354110, -125.1380233598488019 ) ) ;
#8021 = CARTESIAN_POINT ( 'NONE',  ( -20.47566338032521216, -16.24827550219808003, 25.06314818626711372 ) ) ;
#8022 = ORIENTED_EDGE ( 'NONE', *, *, #25018, .F. ) ;
#8023 = CARTESIAN_POINT ( 'NONE',  ( -1.619063947482194177, 35.99532424477422410, 29.22875152547716482 ) ) ;
#8024 = EDGE_CURVE ( 'NONE', #26828, #6495, #15751, .T. ) ;
#8025 = CARTESIAN_POINT ( 'NONE',  ( 109.1592201516379674, -0.006044422199831509662, -0.005027640251764362717 ) ) ;
#8026 = CARTESIAN_POINT ( 'NONE',  ( 5.340103579038210313, -117.9209211655063569, 88.52145169228927557 ) ) ;
#8027 = ORIENTED_EDGE ( 'NONE', *, *, #12843, .T. ) ;
#8028 = ORIENTED_EDGE ( 'NONE', *, *, #10523, .T. ) ;
#8029 = EDGE_CURVE ( 'NONE', #28095, #26828, #12649, .T. ) ;
#8030 = FACE_OUTER_BOUND ( 'NONE', #12702, .T. ) ;
#8031 = VERTEX_POINT ( 'NONE', #2897 ) ;
#8032 = EDGE_LOOP ( 'NONE', ( #17671, #19164, #15774, #8813 ) ) ;
#8033 = ADVANCED_FACE ( 'NONE', ( #731 ), #10191, .F. ) ;
#8034 = CARTESIAN_POINT ( 'NONE',  ( 1.833691583653538792, 96.83253123394209183, 108.0753610255256376 ) ) ;
#8035 = ORIENTED_EDGE ( 'NONE', *, *, #4777, .T. ) ;
#8036 = CARTESIAN_POINT ( 'NONE',  ( 25.98552792386799126, 112.6247604222998859, 10.75254026142839336 ) ) ;
#8037 = CARTESIAN_POINT ( 'NONE',  ( 30.59138290137876481, 79.74792615266136409, 84.53179630244015641 ) ) ;
#8038 = CARTESIAN_POINT ( 'NONE',  ( -9.156249394959713683, 53.90509764945130655, -8.027840202794127578 ) ) ;
#8039 = B_SPLINE_CURVE_WITH_KNOTS ( 'NONE', 3,
 ( #2845, #11337, #15936, #9177, #20110, #27003, #13920 ),
 .UNSPECIFIED., .F., .F.,
 ( 4, 3, 4 ),
 ( 8.998878031629686802E-18, 0.0002669560319015653704, 0.0004157520161273759373 ),
 .UNSPECIFIED. ) ;
#8040 = CARTESIAN_POINT ( 'NONE',  ( 2.430230287190572103, -86.70145658344738138, 116.8646894862409056 ) ) ;
#8041 = CARTESIAN_POINT ( 'NONE',  ( 21.16825799904930605, 119.4343305756974871, 63.85626241912757450 ) ) ;
#8042 = DIRECTION ( 'NONE',  ( -1.000000000000000000, -0.000000000000000000, -0.000000000000000000 ) ) ;
#8043 = CARTESIAN_POINT ( 'NONE',  ( -20.20700224038492721, 28.44216453106536946, -8.199606986804427677 ) ) ;
#8044 = ORIENTED_EDGE ( 'NONE', *, *, #1982, .F. ) ;
#8045 = CARTESIAN_POINT ( 'NONE',  ( -1.048996300304477769, -13.42280206896947092, 43.78665266739852058 ) ) ;
#8047 = CARTESIAN_POINT ( 'NONE',  ( -1.050229599974473516, 43.63650726458064355, -13.90955673306141627 ) ) ;
#8046 = CARTESIAN_POINT ( 'NONE',  ( 32.73300124599738581, 8.473903470907664826, -117.3295799645428588 ) ) ;
#8048 = DIRECTION ( 'NONE',  ( 0.5914120900931444380, 0.09226095020378470568, -0.8010740644654233966 ) ) ;
#8049 = ORIENTED_EDGE ( 'NONE', *, *, #24124, .F. ) ;
#8050 = ORIENTED_EDGE ( 'NONE', *, *, #27976, .F. ) ;
#8051 = CARTESIAN_POINT ( 'NONE',  ( 1.833485406944043827, -141.8265699653865113, -30.69200235379080510 ) ) ;
#8052 = CARTESIAN_POINT ( 'NONE',  ( 119.2224693531408803, 70.00000000000000000, -19.99999999999998934 ) ) ;
#8053 = CARTESIAN_POINT ( 'NONE',  ( -20.21097721712958517, 28.05863618200121934, 9.464413111084452268 ) ) ;
#8054 = CARTESIAN_POINT ( 'NONE',  ( 10.93730112725969938, 56.95489579269752767, 140.0398180619111770 ) ) ;
#8055 = CARTESIAN_POINT ( 'NONE',  ( 109.1589550718174877, 0.004269295012386558133, 0.006257602293694224452 ) ) ;
#8056 = CARTESIAN_POINT ( 'NONE',  ( -1.113548883309542603, 12.28732181966579695, 44.18588492042577798 ) ) ;
#8057 = CARTESIAN_POINT ( 'NONE',  ( -1.619063947482201282, -44.80407745103776307, 11.94059994246206635 ) ) ;
#8058 = ORIENTED_EDGE ( 'NONE', *, *, #11450, .F. ) ;
#8059 = CARTESIAN_POINT ( 'NONE',  ( 32.73300124599732186, 0.000000000000000000, 0.000000000000000000 ) ) ;
#8060 = CARTESIAN_POINT ( 'NONE',  ( -22.34422965417126505, 5.100074259623119666, 37.57019010019537575 ) ) ;
#8061 = CARTESIAN_POINT ( 'NONE',  ( -1.046936909428696882, 12.93351869073272908, -43.93225665392618851 ) ) ;
#8062 = CARTESIAN_POINT ( 'NONE',  ( 119.2224693531408803, 90.00000000000005684, -40.00000000000000711 ) ) ;
#8063 = CARTESIAN_POINT ( 'NONE',  ( 25.64699802086723679, 107.4581924007665350, 34.66526531169679259 ) ) ;
#8064 = CARTESIAN_POINT ( 'NONE',  ( 1.833206308920097172, -108.3342547309371469, 96.54250175814081558 ) ) ;
#8065 = CARTESIAN_POINT ( 'NONE',  ( -4.473127245936431073, 3.196405119333807221, -49.22197550883368677 ) ) ;
#8066 = ADVANCED_FACE ( 'NONE', ( #12938 ), #13835, .T. ) ;
#8067 = ORIENTED_EDGE ( 'NONE', *, *, #14398, .F. ) ;
#8068 = FACE_OUTER_BOUND ( 'NONE', #285, .T. ) ;
#8069 = CARTESIAN_POINT ( 'NONE',  ( 109.1586900883932856, -0.006479576224403809682, -0.002995460350180784680 ) ) ;
#8070 = EDGE_CURVE ( 'NONE', #17840, #17905, #15030, .T. ) ;
#8071 = CARTESIAN_POINT ( 'NONE',  ( 2.430230287190592531, -57.85706160874235593, 133.5180086894989415 ) ) ;
#8072 = ADVANCED_FACE ( 'NONE', ( #27793 ), #22588, .T. ) ;
#8073 = B_SPLINE_CURVE_WITH_KNOTS ( 'NONE', 3,
 ( #19647, #26000, #23998, #23863 ),
 .UNSPECIFIED., .F., .F.,
 ( 4, 4 ),
 ( 0.0005339083821118883934, 0.001067817517169162515 ),
 .UNSPECIFIED. ) ;
#8074 = VERTEX_POINT ( 'NONE', #14542 ) ;
#8075 = CARTESIAN_POINT ( 'NONE',  ( 32.73300124599741423, -75.82012867748416340, -89.94078864464141532 ) ) ;
#8076 = ORIENTED_EDGE ( 'NONE', *, *, #12634, .F. ) ;
#8077 = CARTESIAN_POINT ( 'NONE',  ( -2.265401668238139266, -17.02144111536849636, 43.82493763960401623 ) ) ;
#8078 = CARTESIAN_POINT ( 'NONE',  ( -1.048171036023512803, -43.23005599774311492, -15.11933492062811801 ) ) ;
#8079 = CARTESIAN_POINT ( 'NONE',  ( -20.57838717382308147, -10.78122205917020437, -27.96569011373082603 ) ) ;
#8080 = CARTESIAN_POINT ( 'NONE',  ( -1.619063947482201282, 44.80407745103784123, -11.94059994246174838 ) ) ;
#8081 = CARTESIAN_POINT ( 'NONE',  ( 24.01988960052068123, 129.8107982898200987, 17.94039809062665114 ) ) ;
#8082 = LINE ( 'NONE', #1159, #23095 ) ;
#8083 = CARTESIAN_POINT ( 'NONE',  ( 25.64681081121879203, 112.3352186517032294, -11.38886654529559017 ) ) ;
#8084 = CARTESIAN_POINT ( 'NONE',  ( -20.38016308990359349, -10.62413300761005353, -27.81387210821418776 ) ) ;
#8085 = ORIENTED_EDGE ( 'NONE', *, *, #14943, .F. ) ;
#8086 = VERTEX_POINT ( 'NONE', #8497 ) ;
#8087 = CARTESIAN_POINT ( 'NONE',  ( 1.834118845439484335, -15.34511559672585435, -144.2964192726483645 ) ) ;
#8088 = CARTESIAN_POINT ( 'NONE',  ( -20.57838717382308147, -23.26537097894118133, -18.89542499756491978 ) ) ;
#8089 = CARTESIAN_POINT ( 'NONE',  ( 2.433796855181233454, 84.34988187691088513, -118.5671979538048504 ) ) ;
#8090 = CARTESIAN_POINT ( 'NONE',  ( -1.155031165708890306, 12.20332162035463419, -44.25214473648917135 ) ) ;
#8091 = DIRECTION ( 'NONE',  ( 0.000000000000000000, 5.223019709707975211E-21, -1.000000000000000000 ) ) ;
#8092 = CARTESIAN_POINT ( 'NONE',  ( 2.063896406836605024, 133.2511741302128314, -57.85593781835284233 ) ) ;
#8093 = CARTESIAN_POINT ( 'NONE',  ( -1.049817751779892117, -45.79652915392414769, -0.5106138415325238711 ) ) ;
#8094 = ORIENTED_EDGE ( 'NONE', *, *, #11768, .F. ) ;
#8095 = CARTESIAN_POINT ( 'NONE',  ( 19.66333377628718182, 105.3186440504706951, -88.78556591841191903 ) ) ;
#8096 = CARTESIAN_POINT ( 'NONE',  ( 180.4657679828686980, -1.252232817320263489E-15, 3.130582043300658722E-16 ) ) ;
#8097 = CARTESIAN_POINT ( 'NONE',  ( -20.20700224038492721, -23.35150625415671755, -18.19058640100215385 ) ) ;
#8098 = EDGE_CURVE ( 'NONE', #21365, #675, #17142, .T. ) ;
#8099 = CARTESIAN_POINT ( 'NONE',  ( -20.24419206586953379, -24.70913649113841970, -16.36655224501358319 ) ) ;
#8100 = CARTESIAN_POINT ( 'NONE',  ( 24.01988960052070610, -129.0012934948647114, 23.05141021591238371 ) ) ;
#8101 = VERTEX_POINT ( 'NONE', #25917 ) ;
#8102 = CARTESIAN_POINT ( 'NONE',  ( 109.1586900883932856, -0.0008465529156635612316, -0.007088091345229652514 ) ) ;
#8103 = LINE ( 'NONE', #14555, #12087 ) ;
#8104 = ORIENTED_EDGE ( 'NONE', *, *, #2356, .T. ) ;
#8105 = VERTEX_POINT ( 'NONE', #19424 ) ;
#8106 = ORIENTED_EDGE ( 'NONE', *, *, #7553, .T. ) ;
#8107 = CARTESIAN_POINT ( 'NONE',  ( 21.16825799904906802, -32.46271504707843292, -131.4851843440079620 ) ) ;
#8108 = CARTESIAN_POINT ( 'NONE',  ( -7.078251931573400491, 20.86696228105224549, -47.71415099571811425 ) ) ;
#8109 = CARTESIAN_POINT ( 'NONE',  ( -55.24271866751342941, -0.006757859501005985571, -0.006671293903669251422 ) ) ;
#8110 = ORIENTED_EDGE ( 'NONE', *, *, #27428, .F. ) ;
#8111 = CARTESIAN_POINT ( 'NONE',  ( 1.833485406944057594, 58.53321471327059555, -132.7804117027882285 ) ) ;
#8112 = DIRECTION ( 'NONE',  ( 1.000000000000000000, -6.938893903907226837E-18, 1.734723475976806709E-18 ) ) ;
#8113 = EDGE_CURVE ( 'NONE', #20148, #10460, #18441, .T. ) ;
#8114 = CARTESIAN_POINT ( 'NONE',  ( 2.108393763691186695, -138.5721856399487706, 43.67806918959093565 ) ) ;
#8115 = CARTESIAN_POINT ( 'NONE',  ( 25.64704443564076186, -75.45310550990100751, -83.99864088993849975 ) ) ;
#8116 = CARTESIAN_POINT ( 'NONE',  ( -20.20700224038492721, 0.9908225410482660589, 29.58392382092671724 ) ) ;
#8117 = CARTESIAN_POINT ( 'NONE',  ( 25.64699802086725811, -11.56593161917390411, 112.3172869996024730 ) ) ;
#8118 = EDGE_CURVE ( 'NONE', #15484, #12242, #18513, .T. ) ;
#8119 = CARTESIAN_POINT ( 'NONE',  ( 25.86096068574579832, -113.0494979885903746, -0.9975172952970271512 ) ) ;
#8120 = ADVANCED_FACE ( 'NONE', ( #16860 ), #5378, .F. ) ;
#8121 = CARTESIAN_POINT ( 'NONE',  ( 21.16825799904935224, 112.1052598354960992, 75.99073816868315134 ) ) ;
#8122 = CARTESIAN_POINT ( 'NONE',  ( 25.70243777736187951, 112.2504268534934084, 12.53519966262519603 ) ) ;
#8123 = CARTESIAN_POINT ( 'NONE',  ( -55.24198130335446422, 0.009170435128245552417, -0.001516807524704325135 ) ) ;
#8124 = CARTESIAN_POINT ( 'NONE',  ( 28.43349137099833612, -98.08682467580831599, 76.27296957774096597 ) ) ;
#8125 = CARTESIAN_POINT ( 'NONE',  ( 99.22246935314079508, 69.99999999999998579, -40.00000000000000711 ) ) ;
#8126 = VERTEX_POINT ( 'NONE', #10799 ) ;
#8127 = EDGE_LOOP ( 'NONE', ( #21203, #9977, #12863, #2011 ) ) ;
#8128 = DIRECTION ( 'NONE',  ( 0.000000000000000000, 5.223019709707975211E-21, -1.000000000000000000 ) ) ;
#8130 = ORIENTED_EDGE ( 'NONE', *, *, #2431, .F. ) ;
#8129 = DIRECTION ( 'NONE',  ( 0.5946245182733607137, 0.7655593692109022852, -0.2456431038754784968 ) ) ;
#8131 = ORIENTED_EDGE ( 'NONE', *, *, #20837, .T. ) ;
#8132 = VERTEX_POINT ( 'NONE', #5923 ) ;
#8133 = EDGE_LOOP ( 'NONE', ( #27809, #23414, #4983, #399 ) ) ;
#8134 = B_SPLINE_CURVE_WITH_KNOTS ( 'NONE', 3,
 ( #5755, #23316, #14649, #16389, #20856, #12626 ),
 .UNSPECIFIED., .F., .F.,
 ( 4, 2, 4 ),
 ( 1.536381426628689196E-16, 0.003570751334075638293, 0.007141502668151123064 ),
 .UNSPECIFIED. ) ;
#8135 = CARTESIAN_POINT ( 'NONE',  ( -1.019300379054419725, 16.06793277092052818, 42.90269154183410194 ) ) ;
#8136 = CARTESIAN_POINT ( 'NONE',  ( -20.20700224038492010, 16.58740185276710832, -24.51628800869052682 ) ) ;
#8137 = ADVANCED_FACE ( 'NONE', ( #8628 ), #28089, .T. ) ;
#8138 = CARTESIAN_POINT ( 'NONE',  ( 1.833485406944043827, 137.8414413349085521, 45.34878176254281357 ) ) ;
#8139 = CARTESIAN_POINT ( 'NONE',  ( -20.21097721712959228, 23.76068428613707439, 17.67178718142832494 ) ) ;
#8140 = EDGE_CURVE ( 'NONE', #5273, #13567, #14016, .T. ) ;
#8141 = CARTESIAN_POINT ( 'NONE',  ( -20.57838717382308147, 27.96569011373101077, 10.78122205916971055 ) ) ;
#8142 =( NAMED_UNIT ( * ) PLANE_ANGLE_UNIT ( ) SI_UNIT ( $, .RADIAN. ) );
#8143 = EDGE_CURVE ( 'NONE', #6339, #24736, #22296, .T. ) ;
#8144 = VERTEX_POINT ( 'NONE', #6620 ) ;
#8145 = ORIENTED_EDGE ( 'NONE', *, *, #619, .T. ) ;
#8146 = FACE_OUTER_BOUND ( 'NONE', #25958, .T. ) ;
#8148 = CARTESIAN_POINT ( 'NONE',  ( -19.53423201713129842, 4.045852573675910766E-15, -28.92774122539760384 ) ) ;
#8147 = CARTESIAN_POINT ( 'NONE',  ( -8.786685647604720373, -47.14957014837338534, -25.35688121747513435 ) ) ;
#8149 = CARTESIAN_POINT ( 'NONE',  ( 25.64699802086720837, -103.2460182674614941, -45.70780507840543549 ) ) ;
#8150 = CARTESIAN_POINT ( 'NONE',  ( -1.619063947482197729, 2.489035965910159298, -46.30105812165548684 ) ) ;
#8151 = CARTESIAN_POINT ( 'NONE',  ( 26.11404676487257603, 90.92995828888199128, 67.46175819463394419 ) ) ;
#8152 = ORIENTED_EDGE ( 'NONE', *, *, #15361, .F. ) ;
#8153 = CARTESIAN_POINT ( 'NONE',  ( -7.078251931573406708, -5.101176922831029081, -51.82710018979473432 ) ) ;
#8154 = CARTESIAN_POINT ( 'NONE',  ( 109.1624594426973118, -0.01595733256932007141, 0.0004639210235604286246 ) ) ;
#8155 = CARTESIAN_POINT ( 'NONE',  ( -55.24390624410018802, 0.001811362924359719581, 0.01027195578987765215 ) ) ;
#8156 = VERTEX_POINT ( 'NONE', #8922 ) ;
#8157 = CARTESIAN_POINT ( 'NONE',  ( -1.619063947482197729, -44.80407745103793360, -11.94059994246142331 ) ) ;
#8158 = VERTEX_POINT ( 'NONE', #26737 ) ;
#8159 = EDGE_LOOP ( 'NONE', ( #10532, #12670, #14995, #8636 ) ) ;
#8160 = B_SPLINE_CURVE_WITH_KNOTS ( 'NONE', 3,
 ( #21178, #18885, #12679, #16877, #1736, #7682, #23365, #23084, #25377, #16581 ),
 .UNSPECIFIED., .F., .F.,
 ( 4, 3, 3, 4 ),
 ( 3.469446951953614189E-18, 0.0002669560319015691651, 0.0005492286108966379842, 0.0008315040496093522703 ),
 .UNSPECIFIED. ) ;
#8161 = B_SPLINE_CURVE_WITH_KNOTS ( 'NONE', 3,
 ( #22739, #20688, #3142, #3558 ),
 .UNSPECIFIED., .F., .F.,
 ( 4, 4 ),
 ( 0.000000000000000000, 0.01077107196513907815 ),
 .UNSPECIFIED. ) ;
#8162 = CARTESIAN_POINT ( 'NONE',  ( 109.1624594426973260, -0.01476644236456055130, 0.006066618937909619945 ) ) ;
#8163 = VERTEX_POINT ( 'NONE', #20121 ) ;
#8164 = CARTESIAN_POINT ( 'NONE',  ( 55.79472521941426777, -62.63970324008236190, -37.00555938668325950 ) ) ;
#8165 =( BOUNDED_SURFACE ( )  B_SPLINE_SURFACE ( 3, 1, ( 
 ( #2232, #11037 ),
 ( #21693, #8597 ),
 ( #17360, #19800 ),
 ( #6440, #15194 ) ),
 .UNSPECIFIED., .F., .F., .F. ) 
 B_SPLINE_SURFACE_WITH_KNOTS ( ( 4, 4 ),
 ( 2, 2 ),
 ( 0.000000000000000000, 1.000000000000000000 ),
 ( 0.000000000000000000, 1.000000000000000000 ),
 .UNSPECIFIED. ) 
 GEOMETRIC_REPRESENTATION_ITEM ( )  RATIONAL_B_SPLINE_SURFACE ( (
 ( 1.000000000000000000, 1.000000000000000000),
 ( 0.9956975270656955868, 0.8568959468854907557),
 ( 0.9956975270656955868, 0.8568959468854907557),
 ( 1.000000000000000000, 1.000000000000000000) ) ) 
 REPRESENTATION_ITEM ( '' )  SURFACE ( )  );
#8166 = CARTESIAN_POINT ( 'NONE',  ( 28.37599760073042532, 112.5845136272808418, -22.09615888373845038 ) ) ;
#8167 = EDGE_CURVE ( 'NONE', #21682, #25305, #14387, .T. ) ;
#8168 = B_SPLINE_CURVE_WITH_KNOTS ( 'NONE', 3,
 ( #6632, #13362, #7065, #28475, #13226, #421, #26194, #22161, #6773, #26609 ),
 .UNSPECIFIED., .F., .F.,
 ( 4, 3, 3, 4 ),
 ( 1.962615573354718958E-17, 0.0002669559177086296099, 0.0005339118354151037174, 0.001067817517169159913 ),
 .UNSPECIFIED. ) ;
#8169 = CARTESIAN_POINT ( 'NONE',  ( -20.57838717382308147, -23.26537097894090778, 18.89542499756525729 ) ) ;
#8170 = CARTESIAN_POINT ( 'NONE',  ( 26.04756280548352265, -107.2904246402797384, 36.02883009343602083 ) ) ;
#8171 = CARTESIAN_POINT ( 'NONE',  ( 60.46576798286869803, -4.195655488513964285E-16, 1.048913872128491071E-16 ) ) ;
#8172 = EDGE_CURVE ( 'NONE', #1672, #6924, #22442, .T. ) ;
#8173 = CARTESIAN_POINT ( 'NONE',  ( 32.73300124599739291, -3.836798148478013371, -117.5726003567929610 ) ) ;
#8174 = CARTESIAN_POINT ( 'NONE',  ( -28.41354790283022069, 14.62505768302800924, -18.00456980371904692 ) ) ;
#8175 = FACE_OUTER_BOUND ( 'NONE', #19205, .T. ) ;
#8176 = ADVANCED_FACE ( 'NONE', ( #22150 ), #6969, .T. ) ;
#8177 = ORIENTED_EDGE ( 'NONE', *, *, #15988, .F. ) ;
#8178 = ORIENTED_EDGE ( 'NONE', *, *, #1648, .T. ) ;
#8179 = CARTESIAN_POINT ( 'NONE',  ( -55.24300891470650754, -0.005486913146700035313, 0.008142823778062066586 ) ) ;
#8180 = CARTESIAN_POINT ( 'NONE',  ( 109.1586900883932856, 0.002109621908814802386, -0.006819617742893407421 ) ) ;
#8182 = CARTESIAN_POINT ( 'NONE',  ( 26.28373643307398666, 17.46364395087465482, 126.3595147275199935 ) ) ;
#8181 = CARTESIAN_POINT ( 'NONE',  ( -8.786685647604894456, 7.199674155859698388, 53.04920435127174017 ) ) ;
#8183 = CARTESIAN_POINT ( 'NONE',  ( 28.37603512858357035, -112.5845402829047401, -22.09615328858562933 ) ) ;
#8184 = CARTESIAN_POINT ( 'NONE',  ( 28.43349137099838941, -8.951033805645545627, 123.9292945876798910 ) ) ;
#8185 = CARTESIAN_POINT ( 'NONE',  ( -16.86833981943424376, -19.19877306373879122, -39.83928801320582380 ) ) ;
#8187 = ADVANCED_FACE ( 'NONE', ( #13351 ), #5563, .T. ) ;
#8186 = DIRECTION ( 'NONE',  ( 0.000000000000000000, 5.223019709708233256E-21, -1.000000000000000000 ) ) ;
#8188 = ORIENTED_EDGE ( 'NONE', *, *, #24327, .F. ) ;
#8189 = DIRECTION ( 'NONE',  ( -0.000000000000000000, 1.000000000000000000, 0.000000000000000000 ) ) ;
#8190 = DIRECTION ( 'NONE',  ( -0.5914120900931443270, 0.7903769105750344526, 0.1598001217819390862 ) ) ;
#8191 = CARTESIAN_POINT ( 'NONE',  ( 109.1589550718175161, 0.006257602293702357703, 0.004269295012381938564 ) ) ;
#8192 = CARTESIAN_POINT ( 'NONE',  ( -10.86508079875779842, -24.22249093393332231, -45.04061326950863275 ) ) ;
#8193 = CARTESIAN_POINT ( 'NONE',  ( 2.433796855181205476, -46.34326152018838485, 137.9325382748283744 ) ) ;
#8194 = VERTEX_POINT ( 'NONE', #15505 ) ;
#8195 = CARTESIAN_POINT ( 'NONE',  ( 109.1592201516379674, -0.005485778713202971689, -0.005631912476303796086 ) ) ;
#8196 = CARTESIAN_POINT ( 'NONE',  ( 9.884929003653608603, -150.4771565009630194, -4.203795436553942722 ) ) ;
#8197 = ORIENTED_EDGE ( 'NONE', *, *, #9006, .F. ) ;
#8198 = CARTESIAN_POINT ( 'NONE',  ( 109.1592201516379674, 0.006536841731962000392, 0.004368284148525281539 ) ) ;
#8199 = CARTESIAN_POINT ( 'NONE',  ( 25.64681081121879203, 97.57530875170606066, 56.81519825470789442 ) ) ;
#8200 = CARTESIAN_POINT ( 'NONE',  ( -1.045287976400362417, -43.05558670614257721, -15.59869763335051651 ) ) ;
#8201 = CARTESIAN_POINT ( 'NONE',  ( -1.048172774974269084, -13.17853518375268074, 43.86067135048633503 ) ) ;
#8202 = CARTESIAN_POINT ( 'NONE',  ( -7.733045908741333463, 51.44704017882777691, -10.42750254442556290 ) ) ;
#8203 = CARTESIAN_POINT ( 'NONE',  ( 10.93730112726005821, 140.0398180619120865, -56.95489579269602842 ) ) ;
#8204 = CARTESIAN_POINT ( 'NONE',  ( 1.833838850855462388, 141.9202662332488387, 30.25705358194902672 ) ) ;
#8205 = EDGE_CURVE ( 'NONE', #8855, #19774, #4076, .T. ) ;
#8206 = CARTESIAN_POINT ( 'NONE',  ( -1.045287976400386842, -28.14015102489780062, 36.12803364096639314 ) ) ;
#8207 = CARTESIAN_POINT ( 'NONE',  ( 25.86096068574580187, -35.88291140783994138, 107.2082119295151585 ) ) ;
#8208 = CARTESIAN_POINT ( 'NONE',  ( 25.64708228042118421, 34.92896069507428081, -107.3728320282185251 ) ) ;
#8209 = EDGE_LOOP ( 'NONE', ( #6663, #7745, #21243, #18991 ) ) ;
#8210 = EDGE_CURVE ( 'NONE', #22199, #4319, #11349, .T. ) ;
#8211 = VERTEX_POINT ( 'NONE', #4307 ) ;
#8212 = CARTESIAN_POINT ( 'NONE',  ( -12.82751273423882665, 48.09651489336691554, 8.715310691359739792 ) ) ;
#8213 = B_SPLINE_CURVE_WITH_KNOTS ( 'NONE', 3,
 ( #7753, #14769, #1387, #14487, #11908, #20676 ),
 .UNSPECIFIED., .F., .F.,
 ( 4, 2, 4 ),
 ( 1.736890526760486189E-17, 0.0006311571484586111017, 0.001262314296917205507 ),
 .UNSPECIFIED. ) ;
#8214 = CARTESIAN_POINT ( 'NONE',  ( 28.43349137099830415, -111.8014342888390047, 54.21282462801730873 ) ) ;
#8215 = FACE_OUTER_BOUND ( 'NONE', #28163, .T. ) ;
#8216 = B_SPLINE_CURVE_WITH_KNOTS ( 'NONE', 3,
 ( #3355, #20481, #24961, #2932, #20619, #27235, #12143, #9844 ),
 .UNSPECIFIED., .F., .F.,
 ( 4, 2, 2, 4 ),
 ( 6.938893903907228378E-18, 0.0002429592666046700381, 0.0004859185332093331373, 0.0009718370664186709368 ),
 .UNSPECIFIED. ) ;
#8217 = CARTESIAN_POINT ( 'NONE',  ( 25.64681081121879203, -84.18689316039996129, -75.24277141833577787 ) ) ;
#8218 = CARTESIAN_POINT ( 'NONE',  ( 26.28373643307412166, 126.3595147275199935, -17.46364395087335808 ) ) ;
#8219 = CARTESIAN_POINT ( 'NONE',  ( -7.078251931573406708, 44.92740138729204347, 26.33626633876174239 ) ) ;
#8220 = B_SPLINE_CURVE_WITH_KNOTS ( 'NONE', 3,
 ( #12429, #1769, #15007, #5835 ),
 .UNSPECIFIED., .F., .F.,
 ( 4, 4 ),
 ( 2.221529986854170653E-16, 0.008383748772659682658 ),
 .UNSPECIFIED. ) ;
#8221 = CARTESIAN_POINT ( 'NONE',  ( -55.24198130335446422, 0.009170435128245552417, -0.001516807524704325135 ) ) ;
#8222 = VERTEX_POINT ( 'NONE', #8767 ) ;
#8223 = CARTESIAN_POINT ( 'NONE',  ( 55.79472521941428198, -66.75682020267511518, -28.92526238350541945 ) ) ;
#8224 = CARTESIAN_POINT ( 'NONE',  ( 109.1624594426973260, -0.007576898892904785146, -0.01405141589343901314 ) ) ;
#8225 = CARTESIAN_POINT ( 'NONE',  ( -1.259920593601968397, -25.19630221849078211, -38.49623866863340993 ) ) ;
#8226 = FACE_OUTER_BOUND ( 'NONE', #22065, .T. ) ;
#8227 = LINE ( 'NONE', #6078, #11614 ) ;
#8228 = ORIENTED_EDGE ( 'NONE', *, *, #15237, .T. ) ;
#8229 = CARTESIAN_POINT ( 'NONE',  ( 1.833485406944043827, 44.33323125129927433, 138.1714136985309835 ) ) ;
#8230 = CARTESIAN_POINT ( 'NONE',  ( 26.04756280548353686, -97.45505646068872352, 57.54844730865634261 ) ) ;
#8231 = ORIENTED_EDGE ( 'NONE', *, *, #1806, .F. ) ;
#8232 = CIRCLE ( 'NONE', #10121, 53.53553390275978785 ) ;
#8233 = EDGE_LOOP ( 'NONE', ( #18321, #25024, #18086, #22379 ) ) ;
#8234 = AXIS2_PLACEMENT_3D ( 'NONE', #22600, #11077, #17818 ) ;
#8235 = ORIENTED_EDGE ( 'NONE', *, *, #6352, .T. ) ;
#8236 = B_SPLINE_CURVE_WITH_KNOTS ( 'NONE', 3,
 ( #6431, #13310, #21962, #4399 ),
 .UNSPECIFIED., .F., .F.,
 ( 4, 4 ),
 ( 3.021408270392383890E-16, 0.008383748772659765924 ),
 .UNSPECIFIED. ) ;
#8237 = CARTESIAN_POINT ( 'NONE',  ( -55.25297051322618813, 0.01466904165775564234, -0.002853887643044135131 ) ) ;
#8238 = CARTESIAN_POINT ( 'NONE',  ( 32.73300124599737160, -113.0038235389604466, 32.68291970228198551 ) ) ;
#8239 = DIRECTION ( 'NONE',  ( 0.000000000000000000, 0.000000000000000000, 1.000000000000000000 ) ) ;
#8240 = EDGE_CURVE ( 'NONE', #16841, #13900, #21924, .T. ) ;
#8241 = CARTESIAN_POINT ( 'NONE',  ( -1.045287976400383290, -12.68782741917353185, -44.00138577190637079 ) ) ;
#8242 = ORIENTED_EDGE ( 'NONE', *, *, #18452, .F. ) ;
#8243 = DIRECTION ( 'NONE',  ( 1.000000000000000000, -0.000000000000000000, 0.000000000000000000 ) ) ;
#8244 = EDGE_CURVE ( 'NONE', #19470, #8537, #6848, .T. ) ;
#8245 = ORIENTED_EDGE ( 'NONE', *, *, #13520, .F. ) ;
#8246 = CARTESIAN_POINT ( 'NONE',  ( 2.433796855181205476, 1.451562450951669803, -145.5024947199069345 ) ) ;
#8247 = CARTESIAN_POINT ( 'NONE',  ( -1.045287976400383290, -12.68782741917353185, -44.00138577190637079 ) ) ;
#8248 = EDGE_CURVE ( 'NONE', #11422, #20246, #22974, .T. ) ;
#8249 = B_SPLINE_CURVE_WITH_KNOTS ( 'NONE', 3,
 ( #16775, #4493, #13136, #15283, #13416, #13271, #22057 ),
 .UNSPECIFIED., .F., .F.,
 ( 4, 3, 4 ),
 ( 1.105886215935214523E-17, 0.0007657099931970557912, 0.001530725384384964971 ),
 .UNSPECIFIED. ) ;
#8250 = CARTESIAN_POINT ( 'NONE',  ( 1.833206308920083183, -138.2356393957898888, 44.13245285122219030 ) ) ;
#8251 = CARTESIAN_POINT ( 'NONE',  ( 119.2224693531408803, 90.00000000000005684, 39.99999999999999289 ) ) ;
#8252 = CARTESIAN_POINT ( 'NONE',  ( 13.36082413113063083, 84.67697637120581078, -127.3428651193239602 ) ) ;
#8253 = CARTESIAN_POINT ( 'NONE',  ( -55.24198130335446422, 0.006527480770976314475, -0.006617369590168970667 ) ) ;
#8254 = CARTESIAN_POINT ( 'NONE',  ( -7.078251931573400491, -5.101176922830306104, 51.82710018979479116 ) ) ;
#8255 = CARTESIAN_POINT ( 'NONE',  ( -8.786685647604890903, -25.35688121747466184, 47.14957014837381166 ) ) ;
#8256 = EDGE_LOOP ( 'NONE', ( #18878, #24575, #6089, #20570 ) ) ;
#8257 = EDGE_LOOP ( 'NONE', ( #3573, #23533, #17926, #21410 ) ) ;
#8258 = CARTESIAN_POINT ( 'NONE',  ( -1.155031165708877872, 38.31525684316177660, 25.28071330859845389 ) ) ;
#8259 = CARTESIAN_POINT ( 'NONE',  ( -1.048172774974279076, 45.78636862970795107, -1.020161070261278224 ) ) ;
#8260 = EDGE_LOOP ( 'NONE', ( #12288, #17744 ) ) ;
#8261 = ADVANCED_FACE ( 'NONE', ( #9921 ), #416, .F. ) ;
#8262 = EDGE_LOOP ( 'NONE', ( #25798, #3173 ) ) ;
#8263 = B_SPLINE_CURVE_WITH_KNOTS ( 'NONE', 3,
 ( #6747, #24302, #13336, #22135, #23763, #4009, #4992, #22576, #13918, #390 ),
 .UNSPECIFIED., .F., .F.,
 ( 4, 3, 3, 4 ),
 ( 6.938893903907228378E-18, 0.0002669560319015686230, 0.0005492286108966328885, 0.0008315040496093396936 ),
 .UNSPECIFIED. ) ;
#8264 = B_SPLINE_CURVE_WITH_KNOTS ( 'NONE', 3,
 ( #18996, #8077, #16259, #25059, #7788, #5314, #14087, #3309 ),
 .UNSPECIFIED., .F., .F.,
 ( 4, 2, 2, 4 ),
 ( 2.169948783056603995E-16, 0.002761568181852859429, 0.005523136363705502018, 0.01104627272741079240 ),
 .UNSPECIFIED. ) ;
#8265 = EDGE_CURVE ( 'NONE', #28137, #1581, #23337, .T. ) ;
#8266 = CARTESIAN_POINT ( 'NONE',  ( -23.79248802219724368, 7.157555990716900851, -32.40806545715334153 ) ) ;
#8267 = EDGE_CURVE ( 'NONE', #19868, #21344, #11788, .T. ) ;
#8268 = CARTESIAN_POINT ( 'NONE',  ( -23.77929240705207192, 4.877832571065432887, 35.93174012244165283 ) ) ;
#8269 = CARTESIAN_POINT ( 'NONE',  ( 25.64681081121880624, -46.30456157731397582, 102.9795863647027119 ) ) ;
#8270 = CARTESIAN_POINT ( 'NONE',  ( 30.59141879584279522, 55.75104644134894016, 101.9665761624291775 ) ) ;
#8271 = CARTESIAN_POINT ( 'NONE',  ( 26.11404676487259024, 102.9690087468808031, -47.08215554553414961 ) ) ;
#8272 = CARTESIAN_POINT ( 'NONE',  ( 6.505213034913034000E-17, 4.541450660883840889E-15, -37.50000000000001421 ) ) ;
#8273 = CARTESIAN_POINT ( 'NONE',  ( 25.64660436782564190, -112.3516544824817203, -11.22538561722002548 ) ) ;
#8274 = ORIENTED_EDGE ( 'NONE', *, *, #6104, .T. ) ;
#8275 = ORIENTED_EDGE ( 'NONE', *, *, #4081, .T. ) ;
#8277 = CARTESIAN_POINT ( 'NONE',  ( 6.224689322667647851, -126.9212313063849820, 76.23997225729220872 ) ) ;
#8276 = CARTESIAN_POINT ( 'NONE',  ( 109.1586059443104944, 0.001921075557427549818, 0.006808232911144248591 ) ) ;
#8278 = CARTESIAN_POINT ( 'NONE',  ( -20.20700224038492010, -8.199606986804138131, 28.44216453106544762 ) ) ;
#8279 = B_SPLINE_CURVE_WITH_KNOTS ( 'NONE', 3,
 ( #12548, #7689, #5809, #20904 ),
 .UNSPECIFIED., .F., .F.,
 ( 4, 4 ),
 ( 0.000000000000000000, 0.01077107196513889600 ),
 .UNSPECIFIED. ) ;
#8280 = FACE_OUTER_BOUND ( 'NONE', #9487, .T. ) ;
#8281 = CARTESIAN_POINT ( 'NONE',  ( 25.86096068574578766, 90.87263912324419834, 67.25583614083872419 ) ) ;
#8282 = ORIENTED_EDGE ( 'NONE', *, *, #8645, .T. ) ;
#8283 = CARTESIAN_POINT ( 'NONE',  ( 2.108985857320932578, 137.7807691131293950, -46.11505917359297513 ) ) ;
#8284 = CARTESIAN_POINT ( 'NONE',  ( -7.711401346138395674, -35.51061203065555816, -38.61705198405353912 ) ) ;
#8285 = DIRECTION ( 'NONE',  ( 0.000000000000000000, 5.223019709707975211E-21, -1.000000000000000000 ) ) ;
#8286 = ORIENTED_EDGE ( 'NONE', *, *, #22055, .F. ) ;
#8287 = CARTESIAN_POINT ( 'NONE',  ( 2.063896406836605024, -28.88716984836217350, -142.3682421260910473 ) ) ;
#8288 = VERTEX_POINT ( 'NONE', #7770 ) ;
#8289 = ORIENTED_EDGE ( 'NONE', *, *, #7137, .F. ) ;
#8290 = CARTESIAN_POINT ( 'NONE',  ( 2.263178113027048077, -13.80342493153413130, -144.7392881653025825 ) ) ;
#8291 = EDGE_CURVE ( 'NONE', #25686, #1993, #20911, .T. ) ;
#8292 = EDGE_CURVE ( 'NONE', #1116, #17852, #28091, .T. ) ;
#8293 = ORIENTED_EDGE ( 'NONE', *, *, #23171, .F. ) ;
#8294 = AXIS2_PLACEMENT_3D ( 'NONE', #18866, #20881, #5922 ) ;
#8295 = LINE ( 'NONE', #23151, #13323 ) ;
#8296 = B_SPLINE_CURVE_WITH_KNOTS ( 'NONE', 3,
 ( #20243, #27699, #8009, #16771, #25553, #536 ),
 .UNSPECIFIED., .F., .F.,
 ( 4, 2, 4 ),
 ( 4.906538933386797396E-18, 0.003570751334075636559, 0.007141502668151274852 ),
 .UNSPECIFIED. ) ;
#8297 = VECTOR ( 'NONE', #13692, 999.9999999999998863 ) ;
#8298 = CARTESIAN_POINT ( 'NONE',  ( -20.20700224038492010, 18.19058640100223556, -23.35150625415664649 ) ) ;
#8299 = VECTOR ( 'NONE', #23578, 1000.000000000000114 ) ;
#8300 = CARTESIAN_POINT ( 'NONE',  ( 26.11404676487257603, -110.9778746459745520, -22.43340081644882389 ) ) ;
#8301 = CARTESIAN_POINT ( 'NONE',  ( 30.58324630866349025, 106.6567942264195494, 57.02364853894509622 ) ) ;
#8302 = LINE ( 'NONE', #2078, #8299 ) ;
#8303 = CARTESIAN_POINT ( 'NONE',  ( 19.66333377628710366, -4.491394265033200384, 137.6761449113043341 ) ) ;
#8304 = ORIENTED_EDGE ( 'NONE', *, *, #16257, .F. ) ;
#8305 = CARTESIAN_POINT ( 'NONE',  ( 1.833603222531970722, 125.4455769441942863, 72.93978951866027671 ) ) ;
#8307 = CARTESIAN_POINT ( 'NONE',  ( -1.113427685306993542, 45.82016658690751854, -1.967672929087340261 ) ) ;
#8306 = CARTESIAN_POINT ( 'NONE',  ( -20.20700224038492721, -27.82980252387826781, -10.08426345511578504 ) ) ;
#8308 = CARTESIAN_POINT ( 'NONE',  ( -28.41354790283022069, 8.345538364877384652, 21.64275480268738860 ) ) ;
#8309 = ORIENTED_EDGE ( 'NONE', *, *, #18091, .T. ) ;
#8310 = ORIENTED_EDGE ( 'NONE', *, *, #7415, .F. ) ;
#8311 = DIRECTION ( 'NONE',  ( -0.5946245182733607137, 0.6487139525627779735, -0.4749651461092186389 ) ) ;
#8312 = LINE ( 'NONE', #12753, #3777 ) ;
#8314 = CARTESIAN_POINT ( 'NONE',  ( 28.43349137099826862, 17.01091693849741304, 123.0821667346709063 ) ) ;
#8313 = CARTESIAN_POINT ( 'NONE',  ( 1.833485406944057594, -137.8414413349088932, 45.34878176254188276 ) ) ;
#8315 = CARTESIAN_POINT ( 'NONE',  ( 1.894214914920982595, 125.2241265685480869, -73.39939580274808861 ) ) ;
#8316 = B_SPLINE_CURVE_WITH_KNOTS ( 'NONE', 3,
 ( #25386, #16449, #27380, #16157, #7390, #20615 ),
 .UNSPECIFIED., .F., .F.,
 ( 4, 2, 4 ),
 ( 0.000000000000000000, 0.0004335184443140221305, 0.0008670368886280442611 ),
 .UNSPECIFIED. ) ;
#8317 = CARTESIAN_POINT ( 'NONE',  ( -4.162674018437130030, 3.424137510344948510, -48.79210541969630555 ) ) ;
#8318 = VERTEX_POINT ( 'NONE', #1131 ) ;
#8319 = CARTESIAN_POINT ( 'NONE',  ( -24.53237795827027412, -22.94498492516361310, -24.99972053297897290 ) ) ;
#8320 = ORIENTED_EDGE ( 'NONE', *, *, #27548, .T. ) ;
#8321 = CARTESIAN_POINT ( 'NONE',  ( -1.056502255334265339, 13.66916755949911177, 43.72121397317208391 ) ) ;
#8322 = CARTESIAN_POINT ( 'NONE',  ( -2.265401668238147259, 25.45016726748371738, 39.53028715828205009 ) ) ;
#8323 = VECTOR ( 'NONE', #7482, 1000.000000000000000 ) ;
#8324 = CARTESIAN_POINT ( 'NONE',  ( 1.832998868059890096, 145.1092030902949830, -0.5339089137752986991 ) ) ;
#8325 = CARTESIAN_POINT ( 'NONE',  ( 25.86096068574580542, -110.7864907291860561, 22.52859312382151558 ) ) ;
#8326 = CARTESIAN_POINT ( 'NONE',  ( 1.833838850855473490, 117.3439621615263917, 85.36536653357383386 ) ) ;
#8327 = VECTOR ( 'NONE', #8482, 1000.000000000000000 ) ;
#8328 = ORIENTED_EDGE ( 'NONE', *, *, #2318, .F. ) ;
#8329 = CARTESIAN_POINT ( 'NONE',  ( -1.583189561560253589, -16.68617981233733616, -43.29471907393735819 ) ) ;
#8330 = VECTOR ( 'NONE', #2705, 1000.000000000000114 ) ;
#8331 = EDGE_CURVE ( 'NONE', #15612, #4924, #7527, .T. ) ;
#8332 = CARTESIAN_POINT ( 'NONE',  ( -7.711401346138408108, 51.42722225669434266, 10.36923727626067304 ) ) ;
#8333 = EDGE_CURVE ( 'NONE', #8318, #7281, #2708, .T. ) ;
#8334 = B_SPLINE_CURVE_WITH_KNOTS ( 'NONE', 3,
 ( #8835, #13000, #2328, #22216, #8414, #17445, #23824, #8546 ),
 .UNSPECIFIED., .F., .F.,
 ( 4, 2, 2, 4 ),
 ( 3.469446951953614189E-18, 0.0002429588503611210509, 0.0004859177007222386323, 0.0009718354014444772647 ),
 .UNSPECIFIED. ) ;
#8335 =( BOUNDED_SURFACE ( )  B_SPLINE_SURFACE ( 3, 1, ( 
 ( #1510, #10446 ),
 ( #14745, #5705 ),
 ( #14605, #17043 ),
 ( #10170, #12173 ) ),
 .UNSPECIFIED., .F., .F., .F. ) 
 B_SPLINE_SURFACE_WITH_KNOTS ( ( 4, 4 ),
 ( 2, 2 ),
 ( 0.000000000000000000, 1.000000000000000000 ),
 ( 0.000000000000000000, 1.000000000000000000 ),
 .UNSPECIFIED. ) 
 GEOMETRIC_REPRESENTATION_ITEM ( )  RATIONAL_B_SPLINE_SURFACE ( (
 ( 1.000000000000000000, 1.000000000000000000),
 ( 0.9956975270656955868, 0.8568959468854907557),
 ( 0.9956975270656955868, 0.8568959468854907557),
 ( 1.000000000000000000, 1.000000000000000000) ) ) 
 REPRESENTATION_ITEM ( '' )  SURFACE ( )  );
#8336 = VERTEX_POINT ( 'NONE', #27167 ) ;
#8337 = DIRECTION ( 'NONE',  ( 0.000000000000000000, 0.000000000000000000, 1.000000000000000000 ) ) ;
#8338 = ORIENTED_EDGE ( 'NONE', *, *, #7108, .T. ) ;
#8339 = EDGE_CURVE ( 'NONE', #8356, #4222, #5097, .T. ) ;
#8340 = CARTESIAN_POINT ( 'NONE',  ( 9.884929003653608603, -57.36421526887068012, -139.1775604444709700 ) ) ;
#8341 = CARTESIAN_POINT ( 'NONE',  ( -1.113427685306983550, -12.28784199929904730, 44.18561238466750041 ) ) ;
#8342 = FACE_OUTER_BOUND ( 'NONE', #21607, .T. ) ;
#8343 = EDGE_CURVE ( 'NONE', #10583, #20165, #2352, .T. ) ;
#8344 = CARTESIAN_POINT ( 'NONE',  ( -28.41354790283022069, 5.969609727608339966, 22.41474081377994310 ) ) ;
#8345 = VECTOR ( 'NONE', #13768, 1000.000000000000000 ) ;
#8346 = FACE_OUTER_BOUND ( 'NONE', #706, .T. ) ;
#8347 = CARTESIAN_POINT ( 'NONE',  ( 1.834118845439484335, 29.99597360113071787, 141.9759513273465643 ) ) ;
#8348 = CARTESIAN_POINT ( 'NONE',  ( -55.24728320129491266, -0.008013189884951492717, -0.01214321324517155139 ) ) ;
#8349 = AXIS2_PLACEMENT_3D ( 'NONE', #23776, #10388, #8091 ) ;
#8350 = CARTESIAN_POINT ( 'NONE',  ( -1.259920593601978833, -28.82601305773628297, 35.85909937955954518 ) ) ;
#8351 = CARTESIAN_POINT ( 'NONE',  ( 32.73300124599732186, 0.000000000000000000, 0.000000000000000000 ) ) ;
#8352 = CARTESIAN_POINT ( 'NONE',  ( 26.04756280548354042, -47.04636360340759182, -102.9366382251197507 ) ) ;
#8353 = CARTESIAN_POINT ( 'NONE',  ( 5.340103556456459621, -146.8647350107031002, 13.12023871801074293 ) ) ;
#8354 = ORIENTED_EDGE ( 'NONE', *, *, #17942, .T. ) ;
#8355 = AXIS2_PLACEMENT_3D ( 'NONE', #4771, #4621, #13539 ) ;
#8356 = VERTEX_POINT ( 'NONE', #23597 ) ;
#8357 = EDGE_LOOP ( 'NONE', ( #18129, #21226, #21513, #6144 ) ) ;
#8358 = B_SPLINE_CURVE_WITH_KNOTS ( 'NONE', 3,
 ( #20716, #14088, #2730, #24640, #22465, #13805 ),
 .UNSPECIFIED., .F., .F.,
 ( 4, 2, 4 ),
 ( 4.906538933386797396E-18, 0.003570751334075636559, 0.007141502668151274852 ),
 .UNSPECIFIED. ) ;
#8359 = CARTESIAN_POINT ( 'NONE',  ( 26.11404676487257603, 84.89295829319495112, 74.91683232331003239 ) ) ;
#8360 = CARTESIAN_POINT ( 'NONE',  ( -1.045287976400365970, 15.59869763335156101, 43.05558670614217931 ) ) ;
#8361 = CARTESIAN_POINT ( 'NONE',  ( -7.711401346138400115, 38.61705198405368122, -35.51061203065540894 ) ) ;
#8362 = CARTESIAN_POINT ( 'NONE',  ( 1.893872463202028511, -141.7768406633802840, -31.10971550360730120 ) ) ;
#8363 = EDGE_CURVE ( 'NONE', #2427, #23708, #28018, .T. ) ;
#8364 = CARTESIAN_POINT ( 'NONE',  ( -1.239374126674604337, -25.08410696974269527, -38.61989855450929809 ) ) ;
#8365 = CARTESIAN_POINT ( 'NONE',  ( 28.37644542392842695, -124.0168596762486999, 8.957364412599812198 ) ) ;
#8366 = ORIENTED_EDGE ( 'NONE', *, *, #17857, .F. ) ;
#8367 = CARTESIAN_POINT ( 'NONE',  ( -8.786685647604890903, -9.545808661480982948, -52.67761315067281913 ) ) ;
#8368 = CARTESIAN_POINT ( 'NONE',  ( 1.832998868059858122, -0.5339089137758143977, 145.1092030902949830 ) ) ;
#8369 = B_SPLINE_CURVE_WITH_KNOTS ( 'NONE', 3,
 ( #28468, #6216, #10664, #24185, #26188, #23783, #1724, #23642, #26054, #17541 ),
 .UNSPECIFIED., .F., .F.,
 ( 4, 3, 3, 4 ),
 ( 5.003707553108401214E-17, 0.0002669559177086323746, 0.0005339118354151100058, 0.001067817517169148203 ),
 .UNSPECIFIED. ) ;
#8370 = CARTESIAN_POINT ( 'NONE',  ( 32.73300124599741423, 113.0038235389606314, -32.68291970228113996 ) ) ;
#8371 = ORIENTED_EDGE ( 'NONE', *, *, #8710, .T. ) ;
#8372 = CARTESIAN_POINT ( 'NONE',  ( -2.265401668238145483, -36.42007794497270368, -29.73100299756553966 ) ) ;
#8373 = B_SPLINE_CURVE_WITH_KNOTS ( 'NONE', 3,
 ( #22342, #303, #4341, #17850, #22040, #13120 ),
 .UNSPECIFIED., .F., .F.,
 ( 4, 2, 4 ),
 ( 1.389302603484999005E-17, 0.0006311571484586052470, 0.001262314296917187292 ),
 .UNSPECIFIED. ) ;
#8374 = CARTESIAN_POINT ( 'NONE',  ( 25.69398547355840989, -97.43788956976189297, 57.11291030433619653 ) ) ;
#8375 = ORIENTED_EDGE ( 'NONE', *, *, #1465, .T. ) ;
#8376 = EDGE_CURVE ( 'NONE', #17227, #6927, #10288, .T. ) ;
#8377 = VECTOR ( 'NONE', #836, 999.9999999999998863 ) ;
#8378 = VERTEX_POINT ( 'NONE', #28157 ) ;
#8379 = ORIENTED_EDGE ( 'NONE', *, *, #9859, .F. ) ;
#8381 = CIRCLE ( 'NONE', #15698, 151.1787379149930359 ) ;
#8380 =( BOUNDED_SURFACE ( )  B_SPLINE_SURFACE ( 3, 1, ( 
 ( #22867, #15792 ),
 ( #20536, #24877 ),
 ( #27148, #16072 ),
 ( #24601, #17796 ) ),
 .UNSPECIFIED., .F., .F., .F. ) 
 B_SPLINE_SURFACE_WITH_KNOTS ( ( 4, 4 ),
 ( 2, 2 ),
 ( 0.000000000000000000, 1.000000000000000000 ),
 ( 0.000000000000000000, 1.000000000000000000 ),
 .UNSPECIFIED. ) 
 GEOMETRIC_REPRESENTATION_ITEM ( )  RATIONAL_B_SPLINE_SURFACE ( (
 ( 1.000000000000000000, 1.000000000000000000),
 ( 0.9960225298536222738, 0.9999952330161893110),
 ( 0.9960225298536222738, 0.9999952330161893110),
 ( 1.000000000000000000, 1.000000000000000000) ) ) 
 REPRESENTATION_ITEM ( '' )  SURFACE ( )  );
#8382 = EDGE_CURVE ( 'NONE', #12154, #3886, #20552, .T. ) ;
#8383 = CARTESIAN_POINT ( 'NONE',  ( -55.25719721206881729, -0.009391134844728631428, 0.006045473558784497832 ) ) ;
#8384 = CARTESIAN_POINT ( 'NONE',  ( 13.84597867724975551, -140.9259526407712713, 40.76072889493709539 ) ) ;
#8385 = CARTESIAN_POINT ( 'NONE',  ( 109.1721716018069515, -0.01488186354165290347, 0.008358834333178027584 ) ) ;
#8386 = CARTESIAN_POINT ( 'NONE',  ( 16.05277956358202474, 92.36732600443350805, -109.5668455727251285 ) ) ;
#8387 = VERTEX_POINT ( 'NONE', #6029 ) ;
#8388 = CARTESIAN_POINT ( 'NONE',  ( 1.833485406944057594, -59.50871042846138437, -132.3460930279897241 ) ) ;
#8389 = ORIENTED_EDGE ( 'NONE', *, *, #295, .F. ) ;
#8390 = DIRECTION ( 'NONE',  ( -1.000000000000000000, -0.000000000000000000, -0.000000000000000000 ) ) ;
#8391 = B_SPLINE_CURVE_WITH_KNOTS ( 'NONE', 3,
 ( #12038, #12448, #25282, #10325, #23412, #5992, #18794 ),
 .UNSPECIFIED., .F., .F.,
 ( 4, 3, 4 ),
 ( 3.642919299551294898E-17, 0.02816610861753242323, 0.04000277880656207680 ),
 .UNSPECIFIED. ) ;
#8392 = CARTESIAN_POINT ( 'NONE',  ( -20.90916690077961348, 38.93431874629082756, 7.054312691028585824 ) ) ;
#8393 = CARTESIAN_POINT ( 'NONE',  ( 1.833838850855475933, 97.16351016226039405, -107.7780290788686983 ) ) ;
#8394 = CARTESIAN_POINT ( 'NONE',  ( 109.1721716018069515, 0.01673651515802103765, -0.003350975118861028619 ) ) ;
#8395 = VECTOR ( 'NONE', #8544, 1000.000000000000114 ) ;
#8396 = CARTESIAN_POINT ( 'NONE',  ( 109.1592201516379674, -0.006044422199822568030, 0.005027640251767196387 ) ) ;
#8397 = CARTESIAN_POINT ( 'NONE',  ( -40.00000000000000000, 0.000000000000000000, 0.000000000000000000 ) ) ;
#8398 = ORIENTED_EDGE ( 'NONE', *, *, #20632, .T. ) ;
#8399 = ORIENTED_EDGE ( 'NONE', *, *, #3812, .T. ) ;
#8400 = CARTESIAN_POINT ( 'NONE',  ( 2.433796855181233454, 74.00833731765563073, 125.2830755159756677 ) ) ;
#8402 = ORIENTED_EDGE ( 'NONE', *, *, #4747, .F. ) ;
#8401 = DIRECTION ( 'NONE',  ( 0.000000000000000000, 0.000000000000000000, 1.000000000000000000 ) ) ;
#8403 = ORIENTED_EDGE ( 'NONE', *, *, #13864, .T. ) ;
#8404 = EDGE_CURVE ( 'NONE', #5134, #23391, #24335, .T. ) ;
#8405 = ORIENTED_EDGE ( 'NONE', *, *, #1960, .F. ) ;
#8406 = ORIENTED_EDGE ( 'NONE', *, *, #21501, .F. ) ;
#8407 = ADVANCED_FACE ( 'NONE', ( #25739 ), #25073, .F. ) ;
#8408 = B_SPLINE_CURVE_WITH_KNOTS ( 'NONE', 3,
 ( #19969, #9040, #17798, #27149, #4716, #26719, #24603 ),
 .UNSPECIFIED., .F., .F.,
 ( 4, 3, 4 ),
 ( 8.845388854693243284E-18, 0.009512539173626400127, 0.02506242213020845599 ),
 .UNSPECIFIED. ) ;
#8409 = EDGE_CURVE ( 'NONE', #20822, #6550, #15388, .T. ) ;
#8410 = VECTOR ( 'NONE', #4115, 1000.000000000000000 ) ;
#8411 = DIRECTION ( 'NONE',  ( 0.5914120900931443270, -0.8027508043202544741, 0.07630783612999995913 ) ) ;
#8412 = CARTESIAN_POINT ( 'NONE',  ( 1.831572820252008738, 116.8148281295969326, 86.09108691067808650 ) ) ;
#8413 = CARTESIAN_POINT ( 'NONE',  ( -90.83090735639699176, 0.000000000000000000, 0.000000000000000000 ) ) ;
#8414 = CARTESIAN_POINT ( 'NONE',  ( 25.73574536432417403, 24.27578079247314946, -110.3312765349290743 ) ) ;
#8415 = FACE_OUTER_BOUND ( 'NONE', #5201, .T. ) ;
#8416 = CARTESIAN_POINT ( 'NONE',  ( -1.050231094221210748, 27.12595454131558981, 36.90262059116437854 ) ) ;
#8417 = CARTESIAN_POINT ( 'NONE',  ( 26.11404676487259024, 74.91683232331092768, -84.89295829319416953 ) ) ;
#8418 = ORIENTED_EDGE ( 'NONE', *, *, #8857, .F. ) ;
#8419 = ORIENTED_EDGE ( 'NONE', *, *, #22905, .T. ) ;
#8421 = FACE_OUTER_BOUND ( 'NONE', #7454, .T. ) ;
#8420 = CARTESIAN_POINT ( 'NONE',  ( -1.539760825549688850, 29.16712717142812039, 35.94320866319458219 ) ) ;
#8422 = LINE ( 'NONE', #19209, #1429 ) ;
#8423 = CARTESIAN_POINT ( 'NONE',  ( 25.64681081121879203, -110.5293738517606954, -23.06870491922435207 ) ) ;
#8424 = AXIS2_PLACEMENT_3D ( 'NONE', #14335, #10041, #13912 ) ;
#8425 = EDGE_CURVE ( 'NONE', #15441, #16457, #1549, .T. ) ;
#8426 = ORIENTED_EDGE ( 'NONE', *, *, #22772, .F. ) ;
#8427 = CARTESIAN_POINT ( 'NONE',  ( 25.64681081121879203, 97.57530875170684226, -56.81519825470653018 ) ) ;
#8428 = CIRCLE ( 'NONE', #15762, 111.9614997405030152 ) ;
#8429 = CARTESIAN_POINT ( 'NONE',  ( 10.93730112726002979, 104.7670965581027644, -108.9902118373731241 ) ) ;
#8430 = CARTESIAN_POINT ( 'NONE',  ( -1.050231094221220296, -37.20185272688478051, -26.71409683968603588 ) ) ;
#8431 = ORIENTED_EDGE ( 'NONE', *, *, #23327, .T. ) ;
#8432 = ORIENTED_EDGE ( 'NONE', *, *, #23079, .T. ) ;
#8433 = EDGE_CURVE ( 'NONE', #21416, #12683, #5885, .T. ) ;
#8434 = CARTESIAN_POINT ( 'NONE',  ( -1.619063947482201282, -11.94059994246191359, -44.80407745103779860 ) ) ;
#8435 = VERTEX_POINT ( 'NONE', #18828 ) ;
#8436 = EDGE_LOOP ( 'NONE', ( #14458, #8076, #888, #20921 ) ) ;
#8437 = CARTESIAN_POINT ( 'NONE',  ( -8.259864102781676820, 36.24929574824966494, 38.68084189741909995 ) ) ;
#8438 = CIRCLE ( 'NONE', #13472, 53.53553390275978785 ) ;
#8439 = VERTEX_POINT ( 'NONE', #7918 ) ;
#8440 = CARTESIAN_POINT ( 'NONE',  ( -1.239374126674604337, 42.99367564261301311, 16.50008610789253893 ) ) ;
#8441 = CARTESIAN_POINT ( 'NONE',  ( -20.20612091757425688, 18.30568244821375501, -23.26073043121635919 ) ) ;
#8442 = CONICAL_SURFACE ( 'NONE', #24548, 117.6351876552689504, 0.9945805576725580410 ) ;
#8443 = CARTESIAN_POINT ( 'NONE',  ( 109.1778270068192853, 0.003465086990435488432, -0.008646067828082850890 ) ) ;
#8444 = CARTESIAN_POINT ( 'NONE',  ( 25.81918753295378011, -107.2019194967338365, 35.81374485821577736 ) ) ;
#8445 = CARTESIAN_POINT ( 'NONE',  ( -1.050230346682680560, 14.15335421912582170, -43.55729751025868524 ) ) ;
#8446 = DIRECTION ( 'NONE',  ( 0.7563875759206388771, 0.6531865459554678788, 0.03500244528122787441 ) ) ;
#8447 = CARTESIAN_POINT ( 'NONE',  ( -55.24390624410018802, -0.009374879212970498032, 0.004572280736701721943 ) ) ;
#8448 = CARTESIAN_POINT ( 'NONE',  ( 32.73300124599734318, 114.2056417606548706, 28.19767303745648945 ) ) ;
#8449 = FACE_OUTER_BOUND ( 'NONE', #12806, .T. ) ;
#8450 = ORIENTED_EDGE ( 'NONE', *, *, #19202, .F. ) ;
#8452 = ORIENTED_EDGE ( 'NONE', *, *, #17546, .T. ) ;
#8451 = B_SPLINE_CURVE_WITH_KNOTS ( 'NONE', 3,
 ( #13534, #9518, #13965, #15685, #729, #16126 ),
 .UNSPECIFIED., .F., .F.,
 ( 4, 2, 4 ),
 ( 3.035766082959412415E-18, 0.0006311636237756829224, 0.001262327247551362809 ),
 .UNSPECIFIED. ) ;
#8453 = CARTESIAN_POINT ( 'NONE',  ( 5.340103579038250281, -139.5040934216402775, 47.74933483136832990 ) ) ;
#8454 = B_SPLINE_CURVE_WITH_KNOTS ( 'NONE', 3,
 ( #21142, #16403, #3165, #3731, #1426, #14382, #12094 ),
 .UNSPECIFIED., .F., .F.,
 ( 4, 3, 4 ),
 ( 2.695974601917670536E-16, 0.009512539173626363698, 0.02506242213020817844 ),
 .UNSPECIFIED. ) ;
#8455 = FACE_OUTER_BOUND ( 'NONE', #4484, .T. ) ;
#8457 = CARTESIAN_POINT ( 'NONE',  ( 32.73300124599734318, 16.10546300444822165, 116.5274707358856290 ) ) ;
#8456 = DIRECTION ( 'NONE',  ( 1.000000000000000000, -6.938893903907226837E-18, 1.734723475976806709E-18 ) ) ;
#8458 = CARTESIAN_POINT ( 'NONE',  ( 2.433796855181205476, 98.43889364294005873, -107.1581411821775305 ) ) ;
#8459 = CARTESIAN_POINT ( 'NONE',  ( 25.98107933586725338, 97.42660475433947909, 57.50946808479267958 ) ) ;
#8460 = CARTESIAN_POINT ( 'NONE',  ( -1.239374126674604337, -42.99367564261267916, 16.50008610789344488 ) ) ;
#8461 = EDGE_CURVE ( 'NONE', #431, #21575, #3374, .T. ) ;
#8462 = VECTOR ( 'NONE', #16494, 1000.000000000000000 ) ;
#8463 = ORIENTED_EDGE ( 'NONE', *, *, #9667, .F. ) ;
#8464 = CARTESIAN_POINT ( 'NONE',  ( 28.37599760073042177, 13.77583212279483682, -113.9023239246301529 ) ) ;
#8465 = CARTESIAN_POINT ( 'NONE',  ( -25.21435515916025594, 1.749597353048488237E-16, -4.373993382621220594E-17 ) ) ;
#8466 = EDGE_CURVE ( 'NONE', #4937, #19738, #1403, .T. ) ;
#8467 = FACE_OUTER_BOUND ( 'NONE', #21437, .T. ) ;
#8468 = CARTESIAN_POINT ( 'NONE',  ( -55.24271866751342941, 0.008433070970614317194, 0.004365563123939311327 ) ) ;
#8469 = CARTESIAN_POINT ( 'NONE',  ( 26.04756280548354397, -55.62433096787491849, 98.56594554799102070 ) ) ;
#8471 = EDGE_CURVE ( 'NONE', #25254, #18677, #11994, .T. ) ;
#8470 = ORIENTED_EDGE ( 'NONE', *, *, #1105, .T. ) ;
#8472 = CARTESIAN_POINT ( 'NONE',  ( 55.49584447822657296, 15.34602024131385711, -70.91003759562300957 ) ) ;
#8473 = EDGE_LOOP ( 'NONE', ( #18670, #8289, #4761, #15861 ) ) ;
#8474 = CARTESIAN_POINT ( 'NONE',  ( 1.833206308920053207, 116.9567745381559973, 85.89457656603909186 ) ) ;
#8475 = DIRECTION ( 'NONE',  ( 1.000000000000000000, -6.938893903907226837E-18, 1.734723475976806709E-18 ) ) ;
#8476 = CARTESIAN_POINT ( 'NONE',  ( 1.833485406944043827, 44.33323125129927433, 138.1714136985309835 ) ) ;
#8477 = CARTESIAN_POINT ( 'NONE',  ( 1.833206310202329492, -116.9567751109825195, 85.89457578512777047 ) ) ;
#8478 = CARTESIAN_POINT ( 'NONE',  ( 1.833206308920081185, 125.2945011813205127, 73.19872517709758597 ) ) ;
#8479 = CARTESIAN_POINT ( 'NONE',  ( -1.113427685307011084, 35.91272432484659305, -28.52429901637181686 ) ) ;
#8480 = CARTESIAN_POINT ( 'NONE',  ( -1.045287976400365970, -45.76855895860942525, 1.530335034934587002 ) ) ;
#8481 = CARTESIAN_POINT ( 'NONE',  ( 25.64704443564077962, 23.34498572103320058, 110.4715096490033375 ) ) ;
#8482 = DIRECTION ( 'NONE',  ( -1.000000000000000000, -0.000000000000000000, -0.000000000000000000 ) ) ;
#8483 = CARTESIAN_POINT ( 'NONE',  ( 1.833485406944043827, -132.7804117027891948, 58.53321471326832182 ) ) ;
#8484 = CARTESIAN_POINT ( 'NONE',  ( -1.045287976400362417, 25.66401692419989899, -37.92705037016767733 ) ) ;
#8485 = CARTESIAN_POINT ( 'NONE',  ( -55.25297051322618813, 0.01354497706059544504, -0.006313402748432239003 ) ) ;
#8486 = CARTESIAN_POINT ( 'NONE',  ( 8.186469777910922119, -19.05650978729101652, -148.1306754055310932 ) ) ;
#8487 = CARTESIAN_POINT ( 'NONE',  ( -20.57838717382308147, -10.78122205917020437, -27.96569011373082603 ) ) ;
#8488 = ORIENTED_EDGE ( 'NONE', *, *, #17702, .T. ) ;
#8489 = EDGE_CURVE ( 'NONE', #18715, #13261, #13660, .T. ) ;
#8490 = ORIENTED_EDGE ( 'NONE', *, *, #19272, .F. ) ;
#8491 = ORIENTED_EDGE ( 'NONE', *, *, #26214, .F. ) ;
#8492 = CARTESIAN_POINT ( 'NONE',  ( -1.058473599757810746, -42.99101666105219977, 15.81436910992565004 ) ) ;
#8493 = CARTESIAN_POINT ( 'NONE',  ( -1.113427685306992876, 16.03057832159213092, 42.96952363574816758 ) ) ;
#8494 = CARTESIAN_POINT ( 'NONE',  ( 1.831572820252008738, 16.14965423926401655, -144.2101521542828664 ) ) ;
#8495 = CARTESIAN_POINT ( 'NONE',  ( 1.831572820252009626, -84.49389457294216754, 117.9752562883663813 ) ) ;
#8496 = B_SPLINE_CURVE_WITH_KNOTS ( 'NONE', 3,
 ( #16089, #13643, #835, #18238, #22741, #9187, #2560, #24464, #15810, #3007 ),
 .UNSPECIFIED., .F., .F.,
 ( 4, 3, 3, 4 ),
 ( 3.122502256758253386E-17, 0.0002669559177086182800, 0.0005339118354150958028, 0.001067817517169165117 ),
 .UNSPECIFIED. ) ;
#8497 = CARTESIAN_POINT ( 'NONE',  ( -1.619063947482197729, -44.80407745103793360, -11.94059994246142331 ) ) ;
#8498 = CARTESIAN_POINT ( 'NONE',  ( 32.73300124599740002, 62.10906484417377271, -99.90245962373766986 ) ) ;
#8499 = FACE_OUTER_BOUND ( 'NONE', #15941, .T. ) ;
#8500 = ORIENTED_EDGE ( 'NONE', *, *, #28280, .T. ) ;
#8501 = CARTESIAN_POINT ( 'NONE',  ( -1.056502255334264895, -43.72121397317232550, -13.66916755949833373 ) ) ;
#8502 = CARTESIAN_POINT ( 'NONE',  ( -55.24300891470650754, -0.0003472257464211635897, -0.009812809446892990090 ) ) ;
#8503 = CARTESIAN_POINT ( 'NONE',  ( 25.64700659047698750, 23.69811251893883508, -110.3963107228933183 ) ) ;
#8504 = ADVANCED_FACE ( 'NONE', ( #22263 ), #14184, .F. ) ;
#8505 = CARTESIAN_POINT ( 'NONE',  ( -20.47566338032515887, -28.85746366088576664, -7.708089572830313152 ) ) ;
#8506 =( BOUNDED_SURFACE ( )  B_SPLINE_SURFACE ( 3, 1, ( 
 ( #11386, #9392 ),
 ( #13974, #736 ),
 ( #2907, #18143 ),
 ( #446, #13681 ) ),
 .UNSPECIFIED., .F., .F., .F. ) 
 B_SPLINE_SURFACE_WITH_KNOTS ( ( 4, 4 ),
 ( 2, 2 ),
 ( 0.000000000000000000, 1.000000000000000000 ),
 ( 0.000000000000000000, 1.000000000000000000 ),
 .UNSPECIFIED. ) 
 GEOMETRIC_REPRESENTATION_ITEM ( )  RATIONAL_B_SPLINE_SURFACE ( (
 ( 1.000000000000000000, 1.000000000000000000),
 ( 0.9934239774497837239, 0.8357310067453919133),
 ( 0.9934239774497837239, 0.8357310067453919133),
 ( 1.000000000000000000, 1.000000000000000000) ) ) 
 REPRESENTATION_ITEM ( '' )  SURFACE ( )  );
#8507 = EDGE_CURVE ( 'NONE', #13254, #11834, #13001, .T. ) ;
#8508 = ORIENTED_EDGE ( 'NONE', *, *, #27558, .F. ) ;
#8509 = CARTESIAN_POINT ( 'NONE',  ( -6.588769196390752647, 34.04709086065316370, -38.42957692275855663 ) ) ;
#8510 = DIRECTION ( 'NONE',  ( 0.5946245182733607137, -0.7655593692109038395, 0.2456431038754731122 ) ) ;
#8511 = VERTEX_POINT ( 'NONE', #7012 ) ;
#8512 = ORIENTED_EDGE ( 'NONE', *, *, #17344, .T. ) ;
#8513 = ORIENTED_EDGE ( 'NONE', *, *, #17543, .T. ) ;
#8514 = B_SPLINE_CURVE_WITH_KNOTS ( 'NONE', 3,
 ( #14271, #12404, #5952, #16594, #3780, #23092, #25388, #5664 ),
 .UNSPECIFIED., .F., .F.,
 ( 4, 2, 2, 4 ),
 ( 1.250926888277100303E-17, 0.0002429592666046849459, 0.0004859185332093573693, 0.0009718370664187002102 ),
 .UNSPECIFIED. ) ;
#8515 = B_SPLINE_CURVE_WITH_KNOTS ( 'NONE', 3,
 ( #24816, #469, #13702, #18019, #7116, #5069, #22506, #20328 ),
 .UNSPECIFIED., .F., .F.,
 ( 4, 2, 2, 4 ),
 ( 6.938893903907228378E-18, 0.0002429588503611197770, 0.0004859177007222326150, 0.0009718354014444818183 ),
 .UNSPECIFIED. ) ;
#8516 = CARTESIAN_POINT ( 'NONE',  ( 1.832998868059890096, -117.7096351258393128, 84.86110816369568965 ) ) ;
#8517 = DIRECTION ( 'NONE',  ( -1.000000000000000000, -0.000000000000000000, -0.000000000000000000 ) ) ;
#8518 = CARTESIAN_POINT ( 'NONE',  ( -55.24198130335446422, 0.006527480770974009895, 0.006617369590171991688 ) ) ;
#8519 = CARTESIAN_POINT ( 'NONE',  ( -1.239374126674604337, 11.92219841463891861, 44.48112152129332486 ) ) ;
#8520 = VERTEX_POINT ( 'NONE', #28293 ) ;
#8521 = EDGE_CURVE ( 'NONE', #2978, #11691, #17909, .T. ) ;
#8522 = CARTESIAN_POINT ( 'NONE',  ( 1.893872463202068923, -132.2106029832898173, -59.90695624048819212 ) ) ;
#8523 = EDGE_CURVE ( 'NONE', #1087, #14920, #1691, .T. ) ;
#8524 = CARTESIAN_POINT ( 'NONE',  ( -8.786685647604894456, -23.24040270374358030, 48.22796981442792230 ) ) ;
#8525 = CARTESIAN_POINT ( 'NONE',  ( 9.884929003653608603, 4.203795436554465859, -150.4771565009629910 ) ) ;
#8526 = CARTESIAN_POINT ( 'NONE',  ( 10.93730112725939030, 140.0398180619108075, 56.95489579269806057 ) ) ;
#8527 = CARTESIAN_POINT ( 'NONE',  ( -16.86833981943423666, 7.884812276282103127, -43.51541671545727041 ) ) ;
#8528 = CARTESIAN_POINT ( 'NONE',  ( -55.24340739397742794, -0.01010924026184046101, 0.0007387096945705813253 ) ) ;
#8529 = EDGE_CURVE ( 'NONE', #25504, #5185, #12952, .T. ) ;
#8530 = CARTESIAN_POINT ( 'NONE',  ( 13.84597867724970754, 146.3210145202070009, -10.56985607909651925 ) ) ;
#8531 = EDGE_CURVE ( 'NONE', #9075, #21777, #15692, .T. ) ;
#8532 = ORIENTED_EDGE ( 'NONE', *, *, #12184, .T. ) ;
#8533 =( BOUNDED_SURFACE ( )  B_SPLINE_SURFACE ( 3, 1, ( 
 ( #13854, #20331 ),
 ( #7119, #11411 ),
 ( #191, #22367 ),
 ( #26518, #15876 ) ),
 .UNSPECIFIED., .F., .F., .F. ) 
 B_SPLINE_SURFACE_WITH_KNOTS ( ( 4, 4 ),
 ( 2, 2 ),
 ( 0.000000000000000000, 1.000000000000000000 ),
 ( 0.000000000000000000, 1.000000000000000000 ),
 .UNSPECIFIED. ) 
 GEOMETRIC_REPRESENTATION_ITEM ( )  RATIONAL_B_SPLINE_SURFACE ( (
 ( 1.000000000000000000, 1.000000000000000000),
 ( 0.7789835883360576307, 0.9689951854195403280),
 ( 0.7789835883360576307, 0.9689951854195403280),
 ( 1.000000000000000000, 1.000000000000000000) ) ) 
 REPRESENTATION_ITEM ( '' )  SURFACE ( )  );
#8534 = ORIENTED_EDGE ( 'NONE', *, *, #24412, .T. ) ;
#8535 = CARTESIAN_POINT ( 'NONE',  ( 25.87036335909426654, -24.47383578007052662, -110.3794299719623098 ) ) ;
#8536 = CARTESIAN_POINT ( 'NONE',  ( -28.41354790283022069, -19.47297445639540214, 12.60397206714853624 ) ) ;
#8537 = VERTEX_POINT ( 'NONE', #17782 ) ;
#8538 = ORIENTED_EDGE ( 'NONE', *, *, #15862, .F. ) ;
#8539 = EDGE_LOOP ( 'NONE', ( #10875, #5860, #20742, #24172 ) ) ;
#8540 = CARTESIAN_POINT ( 'NONE',  ( 2.433796855181219243, -145.5024947199069913, 1.451562450949123395 ) ) ;
#8541 = CARTESIAN_POINT ( 'NONE',  ( 1.832998868059890096, 44.33343224355417789, -138.1720401012262585 ) ) ;
#8542 = CARTESIAN_POINT ( 'NONE',  ( 2.433796855181233454, 16.65276281464563723, 144.5536872373192807 ) ) ;
#8543 = CARTESIAN_POINT ( 'NONE',  ( 2.433796855181233454, 145.5024947199069913, -1.451562450950139249 ) ) ;
#8544 = DIRECTION ( 'NONE',  ( -0.7563875759206389882, 0.1685564395263298709, -0.6320336713238514648 ) ) ;
#8545 = EDGE_CURVE ( 'NONE', #1646, #11749, #13298, .T. ) ;
#8546 = CARTESIAN_POINT ( 'NONE',  ( 26.11404676487259024, 24.64483677385001315, -110.5078194225158654 ) ) ;
#8547 = CARTESIAN_POINT ( 'NONE',  ( 109.1624594426973118, 0.009004164758064552368, -0.01318243916934998781 ) ) ;
#8548 = CARTESIAN_POINT ( 'NONE',  ( 109.1778270068192853, -0.002278716897421693890, 0.009031542838317245525 ) ) ;
#8550 = EDGE_LOOP ( 'NONE', ( #25279, #21950, #11462, #23712 ) ) ;
#8549 = EDGE_CURVE ( 'NONE', #12509, #7528, #3675, .T. ) ;
#8551 = ORIENTED_EDGE ( 'NONE', *, *, #7365, .F. ) ;
#8552 = CARTESIAN_POINT ( 'NONE',  ( 25.73574536432414561, -57.18187897120868968, 97.42965068311210075 ) ) ;
#8553 = EDGE_CURVE ( 'NONE', #27588, #20203, #3025, .T. ) ;
#8554 = CARTESIAN_POINT ( 'NONE',  ( -55.25719721206881729, -0.0006290797159201363779, 0.01115102788683008592 ) ) ;
#8555 = CARTESIAN_POINT ( 'NONE',  ( 2.263178607246686624, -1.401567185705457463, -145.3892423243864584 ) ) ;
#8556 = CARTESIAN_POINT ( 'NONE',  ( 1.833485406944043827, 96.69979900902318093, -108.1939177044916107 ) ) ;
#8557 = ORIENTED_EDGE ( 'NONE', *, *, #26796, .T. ) ;
#8558 = CARTESIAN_POINT ( 'NONE',  ( -4.780792508754334591, -3.764354093953240277, 49.38761389561005188 ) ) ;
#8559 = CARTESIAN_POINT ( 'NONE',  ( 1.893872463202031398, -144.2520230501565095, -16.11957794552919054 ) ) ;
#8560 = CARTESIAN_POINT ( 'NONE',  ( -1.048171036023509917, -26.08692787913895472, -37.64178826568597458 ) ) ;
#8561 = ORIENTED_EDGE ( 'NONE', *, *, #20953, .T. ) ;
#8562 = VERTEX_POINT ( 'NONE', #26424 ) ;
#8563 = CARTESIAN_POINT ( 'NONE',  ( -55.24271866751342941, 0.001545935011627245191, 0.009369360294294363373 ) ) ;
#8564 = ORIENTED_EDGE ( 'NONE', *, *, #22967, .T. ) ;
#8565 = CARTESIAN_POINT ( 'NONE',  ( 109.1592201516379674, 0.006044422199822535938, -0.005027640251767235419 ) ) ;
#8566 = ORIENTED_EDGE ( 'NONE', *, *, #22772, .T. ) ;
#8567 = B_SPLINE_CURVE_WITH_KNOTS ( 'NONE', 3,
 ( #23323, #13158, #16692, #14517 ),
 .UNSPECIFIED., .F., .F.,
 ( 4, 4 ),
 ( 3.539284956047283840E-16, 0.01077107486149763566 ),
 .UNSPECIFIED. ) ;
#8568 =( BOUNDED_SURFACE ( )  B_SPLINE_SURFACE ( 3, 1, ( 
 ( #10083, #5618 ),
 ( #25761, #19137 ),
 ( #25628, #12645 ),
 ( #14525, #9947 ) ),
 .UNSPECIFIED., .F., .F., .F. ) 
 B_SPLINE_SURFACE_WITH_KNOTS ( ( 4, 4 ),
 ( 2, 2 ),
 ( 0.000000000000000000, 1.000000000000000000 ),
 ( 0.000000000000000000, 1.000000000000000000 ),
 .UNSPECIFIED. ) 
 GEOMETRIC_REPRESENTATION_ITEM ( )  RATIONAL_B_SPLINE_SURFACE ( (
 ( 1.000000000000000000, 1.000000000000000000),
 ( 0.9593753223639863714, 0.9995975284513187731),
 ( 0.9593753223639863714, 0.9995975284513187731),
 ( 1.000000000000000000, 1.000000000000000000) ) ) 
 REPRESENTATION_ITEM ( '' )  SURFACE ( )  );
#8569 = CARTESIAN_POINT ( 'NONE',  ( -90.83090735639699176, 0.000000000000000000, -20.00000000000000000 ) ) ;
#8570 = ORIENTED_EDGE ( 'NONE', *, *, #6380, .F. ) ;
#8571 = CARTESIAN_POINT ( 'NONE',  ( 109.1587776205901577, -0.002904816147418966092, -0.006729130500857893188 ) ) ;
#8572 = VECTOR ( 'NONE', #21005, 999.9999999999998863 ) ;
#8573 = CARTESIAN_POINT ( 'NONE',  ( -20.47566262905009538, 18.81547655725247381, -23.19796652405680248 ) ) ;
#8574 = CARTESIAN_POINT ( 'NONE',  ( 25.64681081121879203, -12.21581276189731469, -112.2483031020014579 ) ) ;
#8575 = FACE_OUTER_BOUND ( 'NONE', #326, .T. ) ;
#8576 = CARTESIAN_POINT ( 'NONE',  ( 2.063896406836609909, -116.7302989755743141, 86.47093297168963488 ) ) ;
#8577 = CARTESIAN_POINT ( 'NONE',  ( -25.21435515916043357, -6.169479169075226643, 34.05351380035340014 ) ) ;
#8578 = EDGE_CURVE ( 'NONE', #6993, #16312, #255, .T. ) ;
#8579 = EDGE_LOOP ( 'NONE', ( #21529, #11393, #9639, #1775 ) ) ;
#8580 = CARTESIAN_POINT ( 'NONE',  ( 1.833838850855474600, 125.6242502389386431, 72.63194208529516516 ) ) ;
#8582 = CARTESIAN_POINT ( 'NONE',  ( -20.57838717382308147, 29.92853265176831812, 1.611677988432465014 ) ) ;
#8581 = CARTESIAN_POINT ( 'NONE',  ( 109.1587776205901861, 0.003057017121600544719, 0.006661366261223563776 ) ) ;
#8583 = CARTESIAN_POINT ( 'NONE',  ( 25.98552792386801968, -112.3992180166319343, 12.89843290883488969 ) ) ;
#8585 = ORIENTED_EDGE ( 'NONE', *, *, #4453, .T. ) ;
#8584 = EDGE_CURVE ( 'NONE', #17077, #1421, #20651, .T. ) ;
#8586 = ORIENTED_EDGE ( 'NONE', *, *, #12675, .F. ) ;
#8587 = CARTESIAN_POINT ( 'NONE',  ( 30.58324630866353644, 116.1819705588612663, 33.60235057864013442 ) ) ;
#8588 = CARTESIAN_POINT ( 'NONE',  ( 1.833485406944043827, -73.01664920993054864, 125.4007332306543105 ) ) ;
#8589 = CARTESIAN_POINT ( 'NONE',  ( -4.780792508754326597, -48.13366140756551914, 11.68149851467511446 ) ) ;
#8590 = EDGE_CURVE ( 'NONE', #4923, #5555, #7162, .T. ) ;
#8591 = CARTESIAN_POINT ( 'NONE',  ( 13.84597867724988518, 69.17016226639039189, 129.3717503931851240 ) ) ;
#8592 = CARTESIAN_POINT ( 'NONE',  ( 5.340103579038085968, 100.3626145943033663, 108.0219267094749114 ) ) ;
#8593 = CARTESIAN_POINT ( 'NONE',  ( 26.04756280548353686, 90.90573670389328242, -67.42001818240375144 ) ) ;
#8594 = ORIENTED_EDGE ( 'NONE', *, *, #22050, .T. ) ;
#8595 = CARTESIAN_POINT ( 'NONE',  ( 2.108393763691192913, -107.1124103264142775, -98.16799842733358616 ) ) ;
#8596 = CARTESIAN_POINT ( 'NONE',  ( 109.1586900883932856, -0.0001010081143884683351, 0.007137750914552287197 ) ) ;
#8597 = CARTESIAN_POINT ( 'NONE',  ( 1.831572820252008738, -59.92262167723526289, 132.1614873090347260 ) ) ;
#8598 = CARTESIAN_POINT ( 'NONE',  ( 5.340103556456493372, -147.4316330165020190, -2.303180381359786644 ) ) ;
#8599 = CARTESIAN_POINT ( 'NONE',  ( 1.833838848569431468, 117.5008734796311529, 85.14939661881604138 ) ) ;
#8600 = ORIENTED_EDGE ( 'NONE', *, *, #7105, .T. ) ;
#8601 = LINE ( 'NONE', #6731, #5718 ) ;
#8602 = CARTESIAN_POINT ( 'NONE',  ( 1.833750490713681458, 15.43355859895851445, -144.2866297127912105 ) ) ;
#8603 = ORIENTED_EDGE ( 'NONE', *, *, #17825, .T. ) ;
#8604 = CARTESIAN_POINT ( 'NONE',  ( 2.263178113027036531, 116.7985471375932036, 86.59154384226214063 ) ) ;
#8605 =( BOUNDED_SURFACE ( )  B_SPLINE_SURFACE ( 3, 1, ( 
 ( #2133, #28469 ),
 ( #8253, #21878 ),
 ( #16753, #8775 ),
 ( #26464, #19044 ) ),
 .UNSPECIFIED., .F., .F., .F. ) 
 B_SPLINE_SURFACE_WITH_KNOTS ( ( 4, 4 ),
 ( 2, 2 ),
 ( 0.000000000000000000, 1.000000000000000000 ),
 ( 0.000000000000000000, 1.000000000000000000 ),
 .UNSPECIFIED. ) 
 GEOMETRIC_REPRESENTATION_ITEM ( )  RATIONAL_B_SPLINE_SURFACE ( (
 ( 1.000000000000000000, 1.000000000000000000),
 ( 0.9593753223639863714, 0.9995975284513187731),
 ( 0.9593753223639863714, 0.9995975284513187731),
 ( 1.000000000000000000, 1.000000000000000000) ) ) 
 REPRESENTATION_ITEM ( '' )  SURFACE ( )  );
#8606 = CARTESIAN_POINT ( 'NONE',  ( 25.64681081121879203, 66.03065707439057519, -91.59071981940505225 ) ) ;
#8607 = DIRECTION ( 'NONE',  ( 0.000000000000000000, 0.000000000000000000, 1.000000000000000000 ) ) ;
#8608 = CARTESIAN_POINT ( 'NONE',  ( 25.64704443564077607, 97.71717520928676493, 56.57116289738639381 ) ) ;
#8609 = CARTESIAN_POINT ( 'NONE',  ( 2.263178113027023652, 125.2099934853450947, 73.90841366068426055 ) ) ;
#8610 = EDGE_CURVE ( 'NONE', #1523, #2580, #21885, .T. ) ;
#8611 = CARTESIAN_POINT ( 'NONE',  ( 25.87036335909426299, 55.67065048714147935, -98.40409479825380856 ) ) ;
#8612 = CARTESIAN_POINT ( 'NONE',  ( 119.2224693531408803, -90.00000000000005684, 39.99999999999997158 ) ) ;
#8613 = CARTESIAN_POINT ( 'NONE',  ( -20.57838717382308147, 28.96176188950229502, 7.715628353033378239 ) ) ;
#8614 = DIRECTION ( 'NONE',  ( 1.000000000000000000, -6.938893903907226837E-18, 1.734723475976806709E-18 ) ) ;
#8615 = CARTESIAN_POINT ( 'NONE',  ( -25.21435515916042647, 15.02493970636146692, -31.17620025257592786 ) ) ;
#8616 = ADVANCED_FACE ( 'NONE', ( #5258 ), #5405, .F. ) ;
#8617 = CARTESIAN_POINT ( 'NONE',  ( 2.063896406836609909, 46.16709813092625581, 137.7380992975104164 ) ) ;
#8618 = EDGE_CURVE ( 'NONE', #14205, #12120, #17428, .T. ) ;
#8619 = CARTESIAN_POINT ( 'NONE',  ( 9.884929003653608603, 97.56484214660623877, 114.6392083957121315 ) ) ;
#8620 = DIRECTION ( 'NONE',  ( 0.000000000000000000, -3.469446951953603342E-16, 1.000000000000000000 ) ) ;
#8621 = CARTESIAN_POINT ( 'NONE',  ( 6.224689322667630975, 62.55544044765430556, -134.1951906609232594 ) ) ;
#8622 = ORIENTED_EDGE ( 'NONE', *, *, #20880, .T. ) ;
#8623 = VERTEX_POINT ( 'NONE', #512 ) ;
#8624 = CARTESIAN_POINT ( 'NONE',  ( -22.34422965417125440, -16.46028608106132651, -34.15536449444082479 ) ) ;
#8625 = CARTESIAN_POINT ( 'NONE',  ( -20.57838717382308147, 1.611677988432361097, -29.92853265176831812 ) ) ;
#8626 = CARTESIAN_POINT ( 'NONE',  ( 26.11404676487259024, 108.0249973236467582, 33.91085499298413453 ) ) ;
#8627 = FACE_OUTER_BOUND ( 'NONE', #8127, .T. ) ;
#8628 = FACE_OUTER_BOUND ( 'NONE', #15894, .T. ) ;
#8629 = CARTESIAN_POINT ( 'NONE',  ( 55.79472521941428198, -53.57698701322248525, 49.22042574086407996 ) ) ;
#8630 = CARTESIAN_POINT ( 'NONE',  ( -4.473127245936434626, -47.80062405537809411, -12.17046501147497750 ) ) ;
#8631 = EDGE_LOOP ( 'NONE', ( #1713, #12980, #25503, #16720 ) ) ;
#8632 = CARTESIAN_POINT ( 'NONE',  ( 2.108393763691198242, 132.2055356348361670, 60.26375949664234355 ) ) ;
#8633 = CARTESIAN_POINT ( 'NONE',  ( -55.24728320129491266, 0.003868537197317429340, 0.01402509393918536899 ) ) ;
#8634 = CARTESIAN_POINT ( 'NONE',  ( 7.762687761849954095E-17, 6.048924312129458720E-15, -44.74884827092600403 ) ) ;
#8635 = CARTESIAN_POINT ( 'NONE',  ( -28.41354790283022069, 19.47297445639567925, 12.60397206714810814 ) ) ;
#8636 = ORIENTED_EDGE ( 'NONE', *, *, #20530, .T. ) ;
#8637 = CARTESIAN_POINT ( 'NONE',  ( 30.58324630866343696, -100.1119227962715996, -67.85993782330868385 ) ) ;
#8638 = CARTESIAN_POINT ( 'NONE',  ( -1.050230346682677007, 0.0006945978175690684661, -45.79907861045643358 ) ) ;
#8639 = ORIENTED_EDGE ( 'NONE', *, *, #4847, .F. ) ;
#8640 = ORIENTED_EDGE ( 'NONE', *, *, #25964, .T. ) ;
#8641 = ORIENTED_EDGE ( 'NONE', *, *, #22090, .T. ) ;
#8642 = ADVANCED_FACE ( 'NONE', ( #9308 ), #27181, .T. ) ;
#8643 = CARTESIAN_POINT ( 'NONE',  ( 26.28373643307413232, -35.44121223574943258, 122.5382646256986590 ) ) ;
#8644 = CARTESIAN_POINT ( 'NONE',  ( 1.833485406944043827, 144.3694338680884925, 14.63699153649408480 ) ) ;
#8645 = EDGE_CURVE ( 'NONE', #17323, #16951, #6798, .T. ) ;
#8646 = CARTESIAN_POINT ( 'NONE',  ( 26.11404676487257603, 65.63269960453364149, -92.25884714080342519 ) ) ;
#8647 = EDGE_CURVE ( 'NONE', #15393, #27833, #25674, .T. ) ;
#8648 = B_SPLINE_CURVE_WITH_KNOTS ( 'NONE', 3,
 ( #28449, #28316, #13334, #19822, #8754, #26168 ),
 .UNSPECIFIED., .F., .F.,
 ( 4, 2, 4 ),
 ( 6.942281208919283290E-18, 0.0006311571484586111017, 0.001262314296917215264 ),
 .UNSPECIFIED. ) ;
#8649 = CARTESIAN_POINT ( 'NONE',  ( 1.833809397773874084, 72.40070666294590751, 125.7576368866145629 ) ) ;
#8650 = CARTESIAN_POINT ( 'NONE',  ( -55.25297051322618813, -0.007247191603131164853, -0.01306918787467609838 ) ) ;
#8651 = ORIENTED_EDGE ( 'NONE', *, *, #13617, .T. ) ;
#8652 = B_SPLINE_CURVE_WITH_KNOTS ( 'NONE', 3,
 ( #8434, #17199, #25985, #8703, #4236, #21807, #2067, #10872 ),
 .UNSPECIFIED., .F., .F.,
 ( 4, 2, 2, 4 ),
 ( 2.225109362706117716E-16, 0.002761568181852862899, 0.005523136363705503753, 0.01104627272741078546 ),
 .UNSPECIFIED. ) ;
#8653 = ORIENTED_EDGE ( 'NONE', *, *, #25532, .T. ) ;
#8654 = CARTESIAN_POINT ( 'NONE',  ( 1.833206310202325051, 126.0392056382542165, 71.90885922990194956 ) ) ;
#8655 = CARTESIAN_POINT ( 'NONE',  ( -1.019300379054419725, -2.023851374322995778, -45.76814864815089123 ) ) ;
#8656 = DIRECTION ( 'NONE',  ( 1.000000000000000000, -6.938893903907226837E-18, 1.734723475976806709E-18 ) ) ;
#8657 = DIRECTION ( 'NONE',  ( -1.000000000000000000, -0.000000000000000000, -0.000000000000000000 ) ) ;
#8658 =( BOUNDED_SURFACE ( )  B_SPLINE_SURFACE ( 3, 1, ( 
 ( #6095, #27813 ),
 ( #26069, #8519 ),
 ( #2021, #21468 ),
 ( #8109, #1608 ) ),
 .UNSPECIFIED., .F., .F., .F. ) 
 B_SPLINE_SURFACE_WITH_KNOTS ( ( 4, 4 ),
 ( 2, 2 ),
 ( 0.000000000000000000, 1.000000000000000000 ),
 ( 0.000000000000000000, 1.000000000000000000 ),
 .UNSPECIFIED. ) 
 GEOMETRIC_REPRESENTATION_ITEM ( )  RATIONAL_B_SPLINE_SURFACE ( (
 ( 1.000000000000000000, 1.000000000000000000),
 ( 0.9934239774497837239, 0.8357310067453919133),
 ( 0.9934239774497837239, 0.8357310067453919133),
 ( 1.000000000000000000, 1.000000000000000000) ) ) 
 REPRESENTATION_ITEM ( '' )  SURFACE ( )  );
#8659 = CARTESIAN_POINT ( 'NONE',  ( -55.24271866751342941, -0.004256484107792937385, -0.008488649505346276131 ) ) ;
#8660 = CARTESIAN_POINT ( 'NONE',  ( 2.433796855181219243, -28.83182736670634583, 142.6247129145647534 ) ) ;
#8661 = CARTESIAN_POINT ( 'NONE',  ( -1.045287976400386842, -28.14015102489780062, 36.12803364096639314 ) ) ;
#8662 = CARTESIAN_POINT ( 'NONE',  ( -1.259920593601976613, -44.39818421957808425, 12.06711544331609609 ) ) ;
#8663 = CARTESIAN_POINT ( 'NONE',  ( -1.031422197589716205, -28.14735071801769095, -36.13727897780117360 ) ) ;
#8664 = ORIENTED_EDGE ( 'NONE', *, *, #16799, .T. ) ;
#8665 = VECTOR ( 'NONE', #237, 1000.000000000000000 ) ;
#8666 = ORIENTED_EDGE ( 'NONE', *, *, #1278, .F. ) ;
#8667 = CARTESIAN_POINT ( 'NONE',  ( 1.894214914920957948, -108.5033568857718649, -96.41356089048393585 ) ) ;
#8668 = CARTESIAN_POINT ( 'NONE',  ( 55.49584447822657296, -48.34726110739950400, -54.09506550945674519 ) ) ;
#8669 = ORIENTED_EDGE ( 'NONE', *, *, #27027, .T. ) ;
#8670 = ORIENTED_EDGE ( 'NONE', *, *, #5865, .F. ) ;
#8671 = VERTEX_POINT ( 'NONE', #9447 ) ;
#8672 = ADVANCED_FACE ( 'NONE', ( #3249 ), #3765, .T. ) ;
#8673 = MANIFOLD_SOLID_BREP ( 'Chamfer1', #3167 ) ;
#8674 = EDGE_CURVE ( 'NONE', #24455, #25128, #17080, .T. ) ;
#8675 = B_SPLINE_CURVE_WITH_KNOTS ( 'NONE', 3,
 ( #20728, #1017, #14676, #25641, #25203, #10386, #16558 ),
 .UNSPECIFIED., .F., .F.,
 ( 4, 3, 4 ),
 ( 5.239467995070050734E-16, 0.02816610861753244405, 0.04000277880656272211 ),
 .UNSPECIFIED. ) ;
#8676 = CARTESIAN_POINT ( 'NONE',  ( 55.79472521941428198, 28.92526238350565393, -66.75682020267501571 ) ) ;
#8677 = EDGE_CURVE ( 'NONE', #4951, #22965, #28103, .T. ) ;
#8678 = CARTESIAN_POINT ( 'NONE',  ( 109.1778270068192853, 0.008960903982060982112, -0.002542344697958619920 ) ) ;
#8679 = ADVANCED_FACE ( 'NONE', ( #8280 ), #8335, .F. ) ;
#8680 = FACE_OUTER_BOUND ( 'NONE', #17201, .T. ) ;
#8681 = CARTESIAN_POINT ( 'NONE',  ( 1.831572820252008738, 117.9752562883678308, -84.49389457294016381 ) ) ;
#8682 = CARTESIAN_POINT ( 'NONE',  ( -1.044557008772713402, 43.01636061109007159, 15.70482370518772086 ) ) ;
#8683 = CARTESIAN_POINT ( 'NONE',  ( 25.64681081121879203, -110.5293738517610080, 23.06870491922286348 ) ) ;
#8684 = CARTESIAN_POINT ( 'NONE',  ( 32.73300124599732186, 0.000000000000000000, 0.000000000000000000 ) ) ;
#8685 = CARTESIAN_POINT ( 'NONE',  ( -1.046935749539996907, 25.87617179820970748, 37.78548154587966934 ) ) ;
#8686 = CARTESIAN_POINT ( 'NONE',  ( -7.733045908741331687, -5.980865481987790666, 52.15131830128831325 ) ) ;
#8687 =( BOUNDED_SURFACE ( )  B_SPLINE_SURFACE ( 3, 1, ( 
 ( #5536, #7573 ),
 ( #12017, #20789 ),
 ( #9719, #18774 ),
 ( #9868, #1352 ) ),
 .UNSPECIFIED., .F., .F., .F. ) 
 B_SPLINE_SURFACE_WITH_KNOTS ( ( 4, 4 ),
 ( 2, 2 ),
 ( 0.000000000000000000, 1.000000000000000000 ),
 ( 0.000000000000000000, 1.000000000000000000 ),
 .UNSPECIFIED. ) 
 GEOMETRIC_REPRESENTATION_ITEM ( )  RATIONAL_B_SPLINE_SURFACE ( (
 ( 1.000000000000000000, 1.000000000000000000),
 ( 0.9956975270656955868, 0.8568959468854907557),
 ( 0.9956975270656955868, 0.8568959468854907557),
 ( 1.000000000000000000, 1.000000000000000000) ) ) 
 REPRESENTATION_ITEM ( '' )  SURFACE ( )  );
#8688 = ORIENTED_EDGE ( 'NONE', *, *, #26871, .T. ) ;
#8689 = VERTEX_POINT ( 'NONE', #27560 ) ;
#8690 = B_SPLINE_CURVE_WITH_KNOTS ( 'NONE', 3,
 ( #9102, #13265, #1906, #17729, #19474, #8540 ),
 .UNSPECIFIED., .F., .F.,
 ( 4, 2, 4 ),
 ( 9.659140056172959483E-18, 0.0006311571484586074154, 0.001262314296917205940 ),
 .UNSPECIFIED. ) ;
#8692 = CARTESIAN_POINT ( 'NONE',  ( -1.031422197589716205, 36.13727897780129439, -28.14735071801756661 ) ) ;
#8691 = DIRECTION ( 'NONE',  ( -0.7637818620346801257, 0.02150485345384840416, 0.6451161201712179993 ) ) ;
#8693 = CARTESIAN_POINT ( 'NONE',  ( 10.93730112725932635, 0.000000000000000000, 0.000000000000000000 ) ) ;
#8694 = CARTESIAN_POINT ( 'NONE',  ( -20.24399999263415850, -29.60996018918693551, -1.282322917263360340 ) ) ;
#8695 = CARTESIAN_POINT ( 'NONE',  ( -1.464342487929870096, 35.90631960086420094, -29.09292098541673965 ) ) ;
#8696 = VERTEX_POINT ( 'NONE', #8020 ) ;
#8697 = CARTESIAN_POINT ( 'NONE',  ( 25.64692232868534560, 97.62014907493959015, -56.73833653200140503 ) ) ;
#8698 = CARTESIAN_POINT ( 'NONE',  ( -20.20700224038492721, -18.19058640100206503, 23.35150625415678860 ) ) ;
#8699 = CARTESIAN_POINT ( 'NONE',  ( -1.046936909428679341, -27.93981068760648157, -36.28616897897442328 ) ) ;
#8700 = VERTEX_POINT ( 'NONE', #1780 ) ;
#8701 = ORIENTED_EDGE ( 'NONE', *, *, #24070, .F. ) ;
#8702 = B_SPLINE_CURVE_WITH_KNOTS ( 'NONE', 3,
 ( #9627, #10221, #7924, #20854 ),
 .UNSPECIFIED., .F., .F.,
 ( 4, 4 ),
 ( 2.081668171172168513E-17, 0.008383560773332729421 ),
 .UNSPECIFIED. ) ;
#8703 = CARTESIAN_POINT ( 'NONE',  ( -4.162674018437137136, -11.82104147411594752, -47.46216648493552981 ) ) ;
#8704 = ORIENTED_EDGE ( 'NONE', *, *, #9941, .T. ) ;
#8705 = CARTESIAN_POINT ( 'NONE',  ( 25.98107933586719298, 107.2544904356373223, 35.99661810150902852 ) ) ;
#8706 = ORIENTED_EDGE ( 'NONE', *, *, #7280, .F. ) ;
#8707 = EDGE_CURVE ( 'NONE', #10702, #18351, #2277, .T. ) ;
#8708 = CARTESIAN_POINT ( 'NONE',  ( 25.81918753295379432, 67.18811037444432088, 90.88802830331984239 ) ) ;
#8709 = VERTEX_POINT ( 'NONE', #23133 ) ;
#8710 = EDGE_CURVE ( 'NONE', #26014, #21864, #21507, .T. ) ;
#8711 = CARTESIAN_POINT ( 'NONE',  ( 2.430230287190589422, 98.44218333480770866, 107.1617224697467634 ) ) ;
#8712 = CARTESIAN_POINT ( 'NONE',  ( -20.24399999263414429, 18.44171895251396265, -23.20123049637371793 ) ) ;
#8713 = CARTESIAN_POINT ( 'NONE',  ( 25.64681081121879203, -66.03065707438999254, 91.59071981940550700 ) ) ;
#8714 = CARTESIAN_POINT ( 'NONE',  ( 2.430230287190572103, -71.49654683843419889, -126.7388733285352345 ) ) ;
#8715 = CARTESIAN_POINT ( 'NONE',  ( -55.25719721206881729, -0.01041086141212477223, 0.004044147484878232723 ) ) ;
#8716 = CARTESIAN_POINT ( 'NONE',  ( 2.108985857320894386, 144.3577886602087403, -16.46110181986536602 ) ) ;
#8717 = CARTESIAN_POINT ( 'NONE',  ( 32.73300124599735739, -3.836798148479648507, 117.5726003567929610 ) ) ;
#8718 = CARTESIAN_POINT ( 'NONE',  ( 25.69398547355839568, 103.4778695380289548, 45.25878216557469358 ) ) ;
#8720 = CARTESIAN_POINT ( 'NONE',  ( -28.13707043255157103, -0.7675454997508607269, -22.88591869784690402 ) ) ;
#8719 = CARTESIAN_POINT ( 'NONE',  ( 1.832998868059858122, -14.63705790013910502, -144.3700883710218648 ) ) ;
#8721 = CARTESIAN_POINT ( 'NONE',  ( -1.031422197589711764, 37.93675465142472802, -25.67058493451456158 ) ) ;
#8722 = EDGE_LOOP ( 'NONE', ( #8488, #22758, #14839, #4479 ) ) ;
#8723 = VERTEX_POINT ( 'NONE', #8150 ) ;
#8724 = CARTESIAN_POINT ( 'NONE',  ( 25.69398547355838502, 83.43419615433096226, -76.12333255527431675 ) ) ;
#8725 = CARTESIAN_POINT ( 'NONE',  ( 1.834118845439484335, -14.99112450600344104, 144.3336252355296381 ) ) ;
#8727 = CARTESIAN_POINT ( 'NONE',  ( 55.49584447822657296, -15.34602024131336151, 70.91003759562310904 ) ) ;
#8726 = CARTESIAN_POINT ( 'NONE',  ( -1.049817751779875907, -27.33161971822171310, 36.75003908324323021 ) ) ;
#8728 = CARTESIAN_POINT ( 'NONE',  ( 10.93730112726002979, 104.7670965581027644, -108.9902118373731241 ) ) ;
#8729 = B_SPLINE_CURVE_WITH_KNOTS ( 'NONE', 3,
 ( #6142, #14892, #6403, #3958, #15156, #28399 ),
 .UNSPECIFIED., .F., .F.,
 ( 4, 2, 4 ),
 ( 0.000000000000000000, 0.0004335184443140241905, 0.0008670368886280483810 ),
 .UNSPECIFIED. ) ;
#8730 = CARTESIAN_POINT ( 'NONE',  ( 19.66333377628728840, 135.6014041990442820, -24.23123354948703323 ) ) ;
#8731 = CARTESIAN_POINT ( 'NONE',  ( -55.25297051322618813, -0.002853887643042011396, 0.01466904165775133329 ) ) ;
#8732 = ORIENTED_EDGE ( 'NONE', *, *, #25751, .T. ) ;
#8733 = CARTESIAN_POINT ( 'NONE',  ( -1.323830074806771062, 16.42382241777537644, -43.04593525292974476 ) ) ;
#8734 = CARTESIAN_POINT ( 'NONE',  ( -90.83090735639699176, 0.000000000000000000, 0.000000000000000000 ) ) ;
#8735 = CARTESIAN_POINT ( 'NONE',  ( 25.64692872815576763, 112.2585610031153038, 12.12228186621096704 ) ) ;
#8736 = CARTESIAN_POINT ( 'NONE',  ( 25.64681081121879203, 75.24277141833607629, -84.18689316039970549 ) ) ;
#8737 = ORIENTED_EDGE ( 'NONE', *, *, #8549, .T. ) ;
#8738 = CARTESIAN_POINT ( 'NONE',  ( -55.24390624410018802, -0.01032895241566633357, -0.001451500391952961289 ) ) ;
#8739 =( BOUNDED_SURFACE ( )  B_SPLINE_SURFACE ( 3, 1, ( 
 ( #573, #9370 ),
 ( #18125, #9506 ),
 ( #26903, #7214 ),
 ( #24776, #5024 ) ),
 .UNSPECIFIED., .F., .F., .F. ) 
 B_SPLINE_SURFACE_WITH_KNOTS ( ( 4, 4 ),
 ( 2, 2 ),
 ( 0.000000000000000000, 1.000000000000000000 ),
 ( 0.000000000000000000, 1.000000000000000000 ),
 .UNSPECIFIED. ) 
 GEOMETRIC_REPRESENTATION_ITEM ( )  RATIONAL_B_SPLINE_SURFACE ( (
 ( 1.000000000000000000, 1.000000000000000000),
 ( 0.9956975270656955868, 0.8568959468854907557),
 ( 0.9956975270656955868, 0.8568959468854907557),
 ( 1.000000000000000000, 1.000000000000000000) ) ) 
 REPRESENTATION_ITEM ( '' )  SURFACE ( )  );
#8740 = CARTESIAN_POINT ( 'NONE',  ( -20.20700224038492721, -28.44216453106542986, -8.199606986804219844 ) ) ;
#8741 = EDGE_CURVE ( 'NONE', #2685, #13364, #21077, .T. ) ;
#8742 = AXIS2_PLACEMENT_3D ( 'NONE', #15247, #20139, #7070 ) ;
#8743 = EDGE_LOOP ( 'NONE', ( #16518, #20875, #22314, #1845 ) ) ;
#8744 = CARTESIAN_POINT ( 'NONE',  ( -8.786685647604885574, 6.096987947571466530E-17, -1.524246986892866633E-17 ) ) ;
#8745 = ORIENTED_EDGE ( 'NONE', *, *, #6646, .T. ) ;
#8746 = EDGE_CURVE ( 'NONE', #987, #27064, #21232, .T. ) ;
#8747 = CARTESIAN_POINT ( 'NONE',  ( 2.433796855181233454, 116.8607839509068498, -86.69855925933855190 ) ) ;
#8748 = CARTESIAN_POINT ( 'NONE',  ( -25.21435515916025594, 1.749597353048488237E-16, -4.373993382621220594E-17 ) ) ;
#8749 = EDGE_LOOP ( 'NONE', ( #23808, #16100, #11715, #3424 ) ) ;
#8750 = EDGE_CURVE ( 'NONE', #182, #4802, #13972, .T. ) ;
#8751 = CARTESIAN_POINT ( 'NONE',  ( 2.108985857320947677, -71.53406810961571693, 126.4634971826981484 ) ) ;
#8752 = CARTESIAN_POINT ( 'NONE',  ( 32.73300124599736449, -66.00340565729409548, 97.37344512919831629 ) ) ;
#8753 = LINE ( 'NONE', #17521, #19874 ) ;
#8754 = CARTESIAN_POINT ( 'NONE',  ( 2.263178607246697727, -138.7064943909642238, -43.59477707254173851 ) ) ;
#8755 = CARTESIAN_POINT ( 'NONE',  ( 109.1721716018069515, 0.001583175916617806213, 0.01699510305643761598 ) ) ;
#8756 = CARTESIAN_POINT ( 'NONE',  ( 109.1592201516379674, 0.001331853079208314200, 0.007748443302128560708 ) ) ;
#8757 = FACE_OUTER_BOUND ( 'NONE', #20646, .T. ) ;
#8758 = DIRECTION ( 'NONE',  ( -1.000000000000000000, -0.000000000000000000, -0.000000000000000000 ) ) ;
#8759 = CARTESIAN_POINT ( 'NONE',  ( 9.884929003653608603, 65.04493172071660467, -135.7578851563879425 ) ) ;
#8760 = VERTEX_POINT ( 'NONE', #7875 ) ;
#8761 = ORIENTED_EDGE ( 'NONE', *, *, #27775, .T. ) ;
#8762 = CARTESIAN_POINT ( 'NONE',  ( -20.20700224038492721, -29.58392382092672790, 0.9908225410481621420 ) ) ;
#8763 = CARTESIAN_POINT ( 'NONE',  ( 55.49584447822657296, 54.09506550945689440, -48.34726110739932636 ) ) ;
#8764 = CARTESIAN_POINT ( 'NONE',  ( 1.832998868059890096, -84.86110816369685494, 117.7096351258384885 ) ) ;
#8765 = VECTOR ( 'NONE', #25380, 1000.000000000000227 ) ;
#8766 = CARTESIAN_POINT ( 'NONE',  ( 109.1592201516379674, 0.005027640251767214602, 0.006044422199822552418 ) ) ;
#8767 = CARTESIAN_POINT ( 'NONE',  ( 1.833485406944057594, 0.5339064996884692604, 145.1085452359073429 ) ) ;
#8768 = EDGE_CURVE ( 'NONE', #4319, #9399, #3952, .T. ) ;
#8769 = CARTESIAN_POINT ( 'NONE',  ( 55.79472521941428198, -72.42790650415570042, -6.880567342320453861 ) ) ;
#8770 = ORIENTED_EDGE ( 'NONE', *, *, #13408, .T. ) ;
#8771 = CARTESIAN_POINT ( 'NONE',  ( 28.37603512858459709, 37.15644006762219220, 108.5491486026792387 ) ) ;
#8772 = CARTESIAN_POINT ( 'NONE',  ( 2.063896406836609909, 132.1577797566314416, -60.31174178979677691 ) ) ;
#8773 = CIRCLE ( 'NONE', #17925, 151.1787379149930359 ) ;
#8774 = CARTESIAN_POINT ( 'NONE',  ( 25.64703792032470986, 23.32999623362277219, -110.4746717456747263 ) ) ;
#8775 = CARTESIAN_POINT ( 'NONE',  ( -1.056502255334264895, -36.75727364034712963, 27.33667001641208572 ) ) ;
#8776 = CARTESIAN_POINT ( 'NONE',  ( 25.98107933586735641, 12.91054317625263437, -112.3948402207510497 ) ) ;
#8777 = CARTESIAN_POINT ( 'NONE',  ( -1.155031165708881646, -42.97366960678589720, 16.13806347973043387 ) ) ;
#8778 = EDGE_CURVE ( 'NONE', #1993, #28403, #15331, .T. ) ;
#8779 =( BOUNDED_SURFACE ( )  B_SPLINE_SURFACE ( 3, 1, ( 
 ( #19010, #1166 ),
 ( #9959, #25356 ),
 ( #16858, #5921 ),
 ( #14395, #12245 ) ),
 .UNSPECIFIED., .F., .F., .F. ) 
 B_SPLINE_SURFACE_WITH_KNOTS ( ( 4, 4 ),
 ( 2, 2 ),
 ( 0.000000000000000000, 1.000000000000000000 ),
 ( 0.000000000000000000, 1.000000000000000000 ),
 .UNSPECIFIED. ) 
 GEOMETRIC_REPRESENTATION_ITEM ( )  RATIONAL_B_SPLINE_SURFACE ( (
 ( 1.000000000000000000, 1.000000000000000000),
 ( 0.6386103224230302855, 0.9954351624131538845),
 ( 0.6386103224230302855, 0.9954351624131538845),
 ( 1.000000000000000000, 1.000000000000000000) ) ) 
 REPRESENTATION_ITEM ( '' )  SURFACE ( )  );
#8780 = VERTEX_POINT ( 'NONE', #16634 ) ;
#8781 = CARTESIAN_POINT ( 'NONE',  ( 2.108393763691170264, 142.3786741588524194, -28.95405853987377398 ) ) ;
#8782 = CARTESIAN_POINT ( 'NONE',  ( 109.1589550718174877, -0.005233222325298260598, 0.005477029346537757269 ) ) ;
#8783 = EDGE_LOOP ( 'NONE', ( #26482, #24369, #25399, #21017 ) ) ;
#8784 = ADVANCED_FACE ( 'NONE', ( #25428 ), #590, .F. ) ;
#8785 = EDGE_CURVE ( 'NONE', #11951, #9428, #24657, .T. ) ;
#8786 = ORIENTED_EDGE ( 'NONE', *, *, #15785, .T. ) ;
#8787 = ORIENTED_EDGE ( 'NONE', *, *, #1885, .F. ) ;
#8788 = AXIS2_PLACEMENT_3D ( 'NONE', #16687, #27895, #7926 ) ;
#8789 = AXIS2_PLACEMENT_3D ( 'NONE', #24272, #11305, #21960 ) ;
#8790 = CARTESIAN_POINT ( 'NONE',  ( 32.73300124599732186, 0.000000000000000000, 0.000000000000000000 ) ) ;
#8791 = LINE ( 'NONE', #1875, #18865 ) ;
#8792 = CARTESIAN_POINT ( 'NONE',  ( -55.24300891470648622, 0.009812809446890878931, 0.0003472257464245802360 ) ) ;
#8793 = VECTOR ( 'NONE', #15367, 1000.000000000000000 ) ;
#8794 = ORIENTED_EDGE ( 'NONE', *, *, #18898, .T. ) ;
#8795 = CARTESIAN_POINT ( 'NONE',  ( -18.41936578851719730, -37.37524689996168803, 20.09935324538230006 ) ) ;
#8796 = CARTESIAN_POINT ( 'NONE',  ( -4.473127245936434626, 37.94261489385718988, -31.51789735524207003 ) ) ;
#8797 = VERTEX_POINT ( 'NONE', #14959 ) ;
#8798 = DIRECTION ( 'NONE',  ( 1.000000000000000000, -6.938893903907226837E-18, 1.734723475976806709E-18 ) ) ;
#8799 = CARTESIAN_POINT ( 'NONE',  ( -9.156249394959713683, 48.32878616081047340, 25.18996226954561735 ) ) ;
#8800 = CARTESIAN_POINT ( 'NONE',  ( 2.433796855181233454, 57.85512797798071460, -133.5135467655512400 ) ) ;
#8801 = CARTESIAN_POINT ( 'NONE',  ( -1.045287976400365970, 45.76855895860946077, 1.530335034933974381 ) ) ;
#8802 = CARTESIAN_POINT ( 'NONE',  ( -25.21435515916043713, 34.05351380035342146, 6.169479169075106739 ) ) ;
#8803 = LINE ( 'NONE', #21336, #7376 ) ;
#8804 = CARTESIAN_POINT ( 'NONE',  ( -1.031422197589711764, 36.13727897780167808, 28.14735071801703725 ) ) ;
#8805 = DIRECTION ( 'NONE',  ( 0.000000000000000000, 0.000000000000000000, 1.000000000000000000 ) ) ;
#8806 = AXIS2_PLACEMENT_3D ( 'NONE', #26308, #6196, #1839 ) ;
#8807 = VECTOR ( 'NONE', #21689, 1000.000000000000114 ) ;
#8808 = CARTESIAN_POINT ( 'NONE',  ( -20.38016308990357572, -27.81387210821415223, 10.62413300761014945 ) ) ;
#8809 = FACE_OUTER_BOUND ( 'NONE', #14169, .T. ) ;
#8810 = CARTESIAN_POINT ( 'NONE',  ( 109.1586900883932856, -0.003656351050331892692, -0.006130969560687349849 ) ) ;
#8811 = CARTESIAN_POINT ( 'NONE',  ( -25.21435515916043002, 23.92354251275938992, -25.00736669481030106 ) ) ;
#8812 = EDGE_CURVE ( 'NONE', #19237, #13619, #2651, .T. ) ;
#8813 = ORIENTED_EDGE ( 'NONE', *, *, #24634, .F. ) ;
#8814 = AXIS2_PLACEMENT_3D ( 'NONE', #10966, #12, #8805 ) ;
#8815 = EDGE_CURVE ( 'NONE', #6918, #16636, #18824, .T. ) ;
#8816 = ORIENTED_EDGE ( 'NONE', *, *, #27395, .F. ) ;
#8817 = CARTESIAN_POINT ( 'NONE',  ( 32.73300124599739291, -20.69176323058542621, -115.8010721414085538 ) ) ;
#8818 = CARTESIAN_POINT ( 'NONE',  ( 10.93730112725993919, -42.00474393596157086, -145.2260730187406352 ) ) ;
#8819 = ORIENTED_EDGE ( 'NONE', *, *, #9241, .F. ) ;
#8820 = ADVANCED_FACE ( 'NONE', ( #8499 ), #27985, .F. ) ;
#8821 = ORIENTED_EDGE ( 'NONE', *, *, #561, .T. ) ;
#8822 = ORIENTED_EDGE ( 'NONE', *, *, #26478, .T. ) ;
#8823 = CARTESIAN_POINT ( 'NONE',  ( 109.1586059443104944, 0.004524147648833166946, 0.005438258427225630375 ) ) ;
#8824 =( BOUNDED_SURFACE ( )  B_SPLINE_SURFACE ( 3, 1, ( 
 ( #4834, #9018 ),
 ( #2519, #15329 ),
 ( #13311, #510 ),
 ( #24421, #15185 ) ),
 .UNSPECIFIED., .F., .F., .F. ) 
 B_SPLINE_SURFACE_WITH_KNOTS ( ( 4, 4 ),
 ( 2, 2 ),
 ( 0.000000000000000000, 1.000000000000000000 ),
 ( 0.000000000000000000, 1.000000000000000000 ),
 .UNSPECIFIED. ) 
 GEOMETRIC_REPRESENTATION_ITEM ( )  RATIONAL_B_SPLINE_SURFACE ( (
 ( 1.000000000000000000, 1.000000000000000000),
 ( 0.9934239774497837239, 0.8357310067453919133),
 ( 0.9934239774497837239, 0.8357310067453919133),
 ( 1.000000000000000000, 1.000000000000000000) ) ) 
 REPRESENTATION_ITEM ( '' )  SURFACE ( )  );
#8825 = B_SPLINE_CURVE_WITH_KNOTS ( 'NONE', 3,
 ( #23214, #21165, #19156, #22925, #27357, #8225, #10393, #1593, #3329, #25077 ),
 .UNSPECIFIED., .F., .F.,
 ( 4, 2, 2, 2, 4 ),
 ( 2.825996620262520077E-16, 0.0003346187017559037265, 0.0006692374035115249099, 0.001003856105267145931, 0.001338474807022767060 ),
 .UNSPECIFIED. ) ;
#8826 = CARTESIAN_POINT ( 'NONE',  ( 2.430230287190589422, -107.1617224697470903, 98.44218333480735339 ) ) ;
#8827 = CARTESIAN_POINT ( 'NONE',  ( 109.1586900883932856, -0.006757191295060859491, -0.002301750759599753733 ) ) ;
#8828 = B_SPLINE_CURVE_WITH_KNOTS ( 'NONE', 3,
 ( #20482, #16163, #20766, #1333, #18305, #9992, #23241, #20620, #21043, #27531 ),
 .UNSPECIFIED., .F., .F.,
 ( 4, 2, 2, 2, 4 ),
 ( 2.888718286224068903E-16, 0.0003346187017559086596, 0.0006692374035115283793, 0.001003856105267148099, 0.001338474807022767927 ),
 .UNSPECIFIED. ) ;
#8829 = CARTESIAN_POINT ( 'NONE',  ( -1.155001620486248770, -25.28075036143248866, -38.31519699443491334 ) ) ;
#8830 =( BOUNDED_SURFACE ( )  B_SPLINE_SURFACE ( 3, 1, ( 
 ( #8596, #17359 ),
 ( #6304, #28296 ),
 ( #6033, #26150 ),
 ( #4407, #19253 ) ),
 .UNSPECIFIED., .F., .F., .F. ) 
 B_SPLINE_SURFACE_WITH_KNOTS ( ( 4, 4 ),
 ( 2, 2 ),
 ( 0.000000000000000000, 1.000000000000000000 ),
 ( 0.000000000000000000, 1.000000000000000000 ),
 .UNSPECIFIED. ) 
 GEOMETRIC_REPRESENTATION_ITEM ( )  RATIONAL_B_SPLINE_SURFACE ( (
 ( 1.000000000000000000, 1.000000000000000000),
 ( 0.9956975270656955868, 0.8568959468854907557),
 ( 0.9956975270656955868, 0.8568959468854907557),
 ( 1.000000000000000000, 1.000000000000000000) ) ) 
 REPRESENTATION_ITEM ( '' )  SURFACE ( )  );
#8831 = VECTOR ( 'NONE', #10542, 1000.000000000000114 ) ;
#8832 = CARTESIAN_POINT ( 'NONE',  ( -1.045287976400362417, 37.92705037016796155, 25.66401692419947977 ) ) ;
#8833 = CARTESIAN_POINT ( 'NONE',  ( 2.063896406836605024, 118.3103904147693157, -84.29612368209032525 ) ) ;
#8834 = CARTESIAN_POINT ( 'NONE',  ( 28.37603512858455801, -91.75440368549980974, 68.88140609180166507 ) ) ;
#8835 = CARTESIAN_POINT ( 'NONE',  ( 25.64681081121880624, 23.88203588908233499, -110.3564950173079353 ) ) ;
#8836 = CARTESIAN_POINT ( 'NONE',  ( 10.93730112725977932, -128.3908183996597074, 79.81734490845860819 ) ) ;
#8837 = CARTESIAN_POINT ( 'NONE',  ( 26.11404676487259024, 113.2169081140373947, -1.130420376097525326 ) ) ;
#8838 = CARTESIAN_POINT ( 'NONE',  ( 1.833838850855474378, -117.4485666028824085, 85.22139087169041716 ) ) ;
#8839 = EDGE_CURVE ( 'NONE', #6575, #27642, #10801, .T. ) ;
#8840 = ORIENTED_EDGE ( 'NONE', *, *, #24348, .T. ) ;
#8841 = ORIENTED_EDGE ( 'NONE', *, *, #13704, .F. ) ;
#8843 = CARTESIAN_POINT ( 'NONE',  ( 28.37599760073042887, 58.91309773266286953, -98.45181492308057614 ) ) ;
#8842 = CARTESIAN_POINT ( 'NONE',  ( -8.786685647604896232, 9.545808661481343549, 52.67761315067276229 ) ) ;
#8844 = DIRECTION ( 'NONE',  ( -0.5946245182733608248, 0.3243201896541688112, -0.7356888587241603439 ) ) ;
#8845 = CARTESIAN_POINT ( 'NONE',  ( 0.000000000000000000, 0.000000000000000000, 0.000000000000000000 ) ) ;
#8846 = CARTESIAN_POINT ( 'NONE',  ( 2.433796855181205476, -16.65276281464661423, 144.5536872373191102 ) ) ;
#8847 = CARTESIAN_POINT ( 'NONE',  ( 32.73300124599732186, 0.000000000000000000, 0.000000000000000000 ) ) ;
#8848 = ORIENTED_EDGE ( 'NONE', *, *, #16906, .F. ) ;
#8849 = CARTESIAN_POINT ( 'NONE',  ( 2.433796855181205476, 145.5024947199069629, 1.451562450950146133 ) ) ;
#8850 = EDGE_CURVE ( 'NONE', #20163, #28300, #620, .T. ) ;
#8851 = ORIENTED_EDGE ( 'NONE', *, *, #460, .F. ) ;
#8852 = CARTESIAN_POINT ( 'NONE',  ( -6.574463467970651287, -34.08059230520071736, -38.37705091668365043 ) ) ;
#8853 = CARTESIAN_POINT ( 'NONE',  ( -1.031422197589711987, -28.14735071801769095, -36.13727897780115939 ) ) ;
#8854 = ORIENTED_EDGE ( 'NONE', *, *, #295, .T. ) ;
#8855 = VERTEX_POINT ( 'NONE', #3894 ) ;
#8856 = CARTESIAN_POINT ( 'NONE',  ( -1.044556982611268170, -28.22896456560694034, -36.05793013899088351 ) ) ;
#8857 = EDGE_CURVE ( 'NONE', #16496, #19868, #6434, .T. ) ;
#8858 = ORIENTED_EDGE ( 'NONE', *, *, #13408, .F. ) ;
#8859 = CARTESIAN_POINT ( 'NONE',  ( 109.1778270068192853, 0.005186985107080939461, 0.007736698406806046500 ) ) ;
#8860 = AXIS2_PLACEMENT_3D ( 'NONE', #19684, #8758, #15363 ) ;
#8861 = EDGE_LOOP ( 'NONE', ( #25353, #6138, #8551, #22527 ) ) ;
#8862 = LINE ( 'NONE', #214, #5521 ) ;
#8863 = EDGE_LOOP ( 'NONE', ( #2738, #1313, #2141, #19764 ) ) ;
#8864 = B_SPLINE_CURVE_WITH_KNOTS ( 'NONE', 3,
 ( #20186, #20047, #19911, #13569 ),
 .UNSPECIFIED., .F., .F.,
 ( 4, 4 ),
 ( 0.000000000000000000, 0.008383560773332717278 ),
 .UNSPECIFIED. ) ;
#8865 = CARTESIAN_POINT ( 'NONE',  ( 2.433796855181205476, 126.7346379669265843, -71.49415740224942795 ) ) ;
#8866 = CARTESIAN_POINT ( 'NONE',  ( 109.1721716018069657, -0.01019541462303503142, -0.01368917435591430511 ) ) ;
#8867 =( BOUNDED_SURFACE ( )  B_SPLINE_SURFACE ( 3, 1, ( 
 ( #10013, #1217 ),
 ( #18490, #27547 ),
 ( #18637, #10155 ),
 ( #928, #20929 ) ),
 .UNSPECIFIED., .F., .F., .F. ) 
 B_SPLINE_SURFACE_WITH_KNOTS ( ( 4, 4 ),
 ( 2, 2 ),
 ( 0.000000000000000000, 1.000000000000000000 ),
 ( 0.000000000000000000, 1.000000000000000000 ),
 .UNSPECIFIED. ) 
 GEOMETRIC_REPRESENTATION_ITEM ( )  RATIONAL_B_SPLINE_SURFACE ( (
 ( 1.000000000000000000, 1.000000000000000000),
 ( 0.9960225298536222738, 0.9999952330161893110),
 ( 0.9960225298536222738, 0.9999952330161893110),
 ( 1.000000000000000000, 1.000000000000000000) ) ) 
 REPRESENTATION_ITEM ( '' )  SURFACE ( )  );
#8869 = VECTOR ( 'NONE', #23608, 1000.000000000000000 ) ;
#8868 = CARTESIAN_POINT ( 'NONE',  ( 109.1592201516379674, -0.004867031887010251669, 0.006174480289200302147 ) ) ;
#8870 = CARTESIAN_POINT ( 'NONE',  ( -55.24390624410018802, 0.007503127514282199352, -0.007245494385991655198 ) ) ;
#8871 = CARTESIAN_POINT ( 'NONE',  ( 2.430230287190581429, -132.3371620660946917, -60.50928654924886274 ) ) ;
#8872 = AXIS2_PLACEMENT_3D ( 'NONE', #18380, #18542, #25039 ) ;
#8873 = CARTESIAN_POINT ( 'NONE',  ( 2.430230287190572103, -138.8342928068223046, 43.58368230469342564 ) ) ;
#8874 = CARTESIAN_POINT ( 'NONE',  ( 109.1589550718175161, -0.001793588804100445990, -0.007359857714025717923 ) ) ;
#8875 = CARTESIAN_POINT ( 'NONE',  ( 25.64692232868535982, -56.17236075412014173, 97.94691534265413679 ) ) ;
#8876 = CIRCLE ( 'NONE', #19433, 151.1787379149930359 ) ;
#8877 = ADVANCED_FACE ( 'NONE', ( #5925 ), #27832, .F. ) ;
#8878 = ORIENTED_EDGE ( 'NONE', *, *, #852, .T. ) ;
#8879 = CARTESIAN_POINT ( 'NONE',  ( 26.11404676487259024, 83.38016054979885894, -76.59696442953111273 ) ) ;
#8880 = EDGE_CURVE ( 'NONE', #3267, #20088, #13572, .T. ) ;
#8881 = CARTESIAN_POINT ( 'NONE',  ( -1.056502255334265339, 45.80535052436398047, 0.5104472526221617290 ) ) ;
#8882 = CARTESIAN_POINT ( 'NONE',  ( 2.108985857320942348, 125.1820688103232015, -73.75356715682956121 ) ) ;
#8883 = CARTESIAN_POINT ( 'NONE',  ( 2.433796855181205476, -109.1007109081232471, 96.28145139437646094 ) ) ;
#8884 = CARTESIAN_POINT ( 'NONE',  ( -6.588769196390761529, 20.50531526814562966, -47.06982923582516065 ) ) ;
#8885 = CARTESIAN_POINT ( 'NONE',  ( 109.1589550718175161, -0.005777059646713217020, -0.004900004919101213011 ) ) ;
#8886 = ADVANCED_FACE ( 'NONE', ( #19881 ), #3369, .F. ) ;
#8887 = CARTESIAN_POINT ( 'NONE',  ( 1.832998868059858122, 138.1720401012266848, 44.33343224355280654 ) ) ;
#8888 = CARTESIAN_POINT ( 'NONE',  ( -25.21435515916043713, -34.29329011225952684, 4.655591116594705703 ) ) ;
#8889 = CARTESIAN_POINT ( 'NONE',  ( 1.832998868059890096, 96.70023740551270919, -108.1944082009147365 ) ) ;
#8890 = VERTEX_POINT ( 'NONE', #6800 ) ;
#8891 = CARTESIAN_POINT ( 'NONE',  ( -55.24340739397742794, 0.008612749836243148785, 0.005344433640974122733 ) ) ;
#8892 = CARTESIAN_POINT ( 'NONE',  ( 2.263178607246631113, -60.41552769843737991, -132.2496131833836159 ) ) ;
#8893 = AXIS2_PLACEMENT_3D ( 'NONE', #17488, #25728, #21822 ) ;
#8894 = ORIENTED_EDGE ( 'NONE', *, *, #3536, .T. ) ;
#8895 = CARTESIAN_POINT ( 'NONE',  ( 25.64700659047694487, -112.9110011064639565, -0.2275682798798776274 ) ) ;
#8896 = VECTOR ( 'NONE', #19985, 1000.000000000000000 ) ;
#8897 = CARTESIAN_POINT ( 'NONE',  ( -21.41430102051751660, -25.94791611261628717, -16.60879216503625244 ) ) ;
#8898 = CARTESIAN_POINT ( 'NONE',  ( 8.186469777910488688, 148.8557359139590517, 12.15801985874036539 ) ) ;
#8899 = VECTOR ( 'NONE', #15677, 1000.000000000000000 ) ;
#8900 = VERTEX_POINT ( 'NONE', #24796 ) ;
#8901 = CARTESIAN_POINT ( 'NONE',  ( 32.73300124599732186, 0.000000000000000000, 0.000000000000000000 ) ) ;
#8902 = CARTESIAN_POINT ( 'NONE',  ( -1.583189561560256253, 44.83405390829688741, 11.94859433442855412 ) ) ;
#8903 = LINE ( 'NONE', #13194, #14729 ) ;
#8904 = CARTESIAN_POINT ( 'NONE',  ( 32.73300124599732186, 0.000000000000000000, 0.000000000000000000 ) ) ;
#8905 = CARTESIAN_POINT ( 'NONE',  ( -8.786685647604885574, 6.096987947571466530E-17, -1.524246986892866633E-17 ) ) ;
#8906 = CARTESIAN_POINT ( 'NONE',  ( 55.49584447822657296, 42.86099773636541244, 58.53775398922272188 ) ) ;
#8907 = ORIENTED_EDGE ( 'NONE', *, *, #2906, .F. ) ;
#8908 = CARTESIAN_POINT ( 'NONE',  ( -8.786685647604885574, 6.096987947571466530E-17, -1.524246986892866633E-17 ) ) ;
#8909 = CARTESIAN_POINT ( 'NONE',  ( 10.93730112725953596, 92.80059208661681680, 119.3442956573276206 ) ) ;
#8910 = CARTESIAN_POINT ( 'NONE',  ( 10.93730112725991432, -71.28103789254845424, -133.3192575531807620 ) ) ;
#8911 = CARTESIAN_POINT ( 'NONE',  ( 25.98552792386801613, -98.51438617140701126, -55.63155129533035392 ) ) ;
#8912 = ORIENTED_EDGE ( 'NONE', *, *, #1105, .F. ) ;
#8913 = ORIENTED_EDGE ( 'NONE', *, *, #20410, .T. ) ;
#8914 = EDGE_LOOP ( 'NONE', ( #5237, #4042, #21080, #15314 ) ) ;
#8915 = VERTEX_POINT ( 'NONE', #15544 ) ;
#8916 = CARTESIAN_POINT ( 'NONE',  ( -20.38016308990358993, -29.73560196176845238, 1.509191766064522655 ) ) ;
#8917 = CARTESIAN_POINT ( 'NONE',  ( 26.11404676487257603, -33.91085499298301897, -108.0249973236470993 ) ) ;
#8918 = ADVANCED_FACE ( 'NONE', ( #596 ), #8506, .F. ) ;
#8920 = CARTESIAN_POINT ( 'NONE',  ( 25.64703792032470631, 75.66285916808298850, 83.80974623566321213 ) ) ;
#8919 = CARTESIAN_POINT ( 'NONE',  ( 2.263178607246686180, 98.32595927618852727, 107.1074316126221362 ) ) ;
#8921 = FACE_BOUND ( 'NONE', #19918, .T. ) ;
#8922 = CARTESIAN_POINT ( 'NONE',  ( 26.11404676487257603, 112.4785329405483765, -12.95861723607337979 ) ) ;
#8923 =( BOUNDED_SURFACE ( )  B_SPLINE_SURFACE ( 3, 1, ( 
 ( #14331, #18358 ),
 ( #27141, #4984 ),
 ( #7449, #23148 ),
 ( #16209, #3406 ) ),
 .UNSPECIFIED., .F., .F., .F. ) 
 B_SPLINE_SURFACE_WITH_KNOTS ( ( 4, 4 ),
 ( 2, 2 ),
 ( 0.000000000000000000, 1.000000000000000000 ),
 ( 0.000000000000000000, 1.000000000000000000 ),
 .UNSPECIFIED. ) 
 GEOMETRIC_REPRESENTATION_ITEM ( )  RATIONAL_B_SPLINE_SURFACE ( (
 ( 1.000000000000000000, 1.000000000000000000),
 ( 0.7789835883360578528, 0.9689951854195403280),
 ( 0.7789835883360578528, 0.9689951854195403280),
 ( 1.000000000000000000, 1.000000000000000000) ) ) 
 REPRESENTATION_ITEM ( '' )  SURFACE ( )  );
#8924 = CARTESIAN_POINT ( 'NONE',  ( 109.1586900883932856, -0.004701023939953891985, -0.005371970278523950648 ) ) ;
#8925 = ORIENTED_EDGE ( 'NONE', *, *, #1314, .F. ) ;
#8926 = CARTESIAN_POINT ( 'NONE',  ( -25.21435515916043357, 31.17620025257608418, 15.02493970636113474 ) ) ;
#8927 = FACE_OUTER_BOUND ( 'NONE', #21314, .T. ) ;
#8928 = CARTESIAN_POINT ( 'NONE',  ( 25.64692872815576408, 11.48248630407279336, 112.3258062264002746 ) ) ;
#8929 = CARTESIAN_POINT ( 'NONE',  ( 10.93730112726002979, 79.81734490846109509, -128.3908183996583432 ) ) ;
#8930 = EDGE_CURVE ( 'NONE', #15242, #20933, #5799, .T. ) ;
#8931 = B_SPLINE_CURVE_WITH_KNOTS ( 'NONE', 3,
 ( #21146, #3735, #8081, #1431, #27482, #16973, #7654 ),
 .UNSPECIFIED., .F., .F.,
 ( 4, 3, 4 ),
 ( 0.000000000000000000, 0.02398743853561324108, 0.04000277880656206986 ),
 .UNSPECIFIED. ) ;
#8932 = CARTESIAN_POINT ( 'NONE',  ( 109.1721716018069657, 0.01567407524362079974, 0.006757465437538844391 ) ) ;
#8933 = EDGE_CURVE ( 'NONE', #18539, #23610, #18460, .T. ) ;
#8934 = VERTEX_POINT ( 'NONE', #24359 ) ;
#8935 = CARTESIAN_POINT ( 'NONE',  ( -25.21435515916043713, 6.169479169075932745, 34.05351380035326514 ) ) ;
#8936 = CARTESIAN_POINT ( 'NONE',  ( 25.64681081121879203, -56.09509703373275613, -97.99105938547980088 ) ) ;
#8937 = ORIENTED_EDGE ( 'NONE', *, *, #25016, .T. ) ;
#8938 = ORIENTED_EDGE ( 'NONE', *, *, #7366, .T. ) ;
#8939 = AXIS2_PLACEMENT_3D ( 'NONE', #12180, #20947, #14472 ) ;
#8940 = ORIENTED_EDGE ( 'NONE', *, *, #26411, .T. ) ;
#8941 = CARTESIAN_POINT ( 'NONE',  ( -55.24271866751342941, -0.008433070970613524425, -0.004365563123939557658 ) ) ;
#8942 = DIRECTION ( 'NONE',  ( 0.000000000000000000, 0.000000000000000000, 1.000000000000000000 ) ) ;
#8943 = CARTESIAN_POINT ( 'NONE',  ( -1.583189561560252701, -16.68617981233673220, 43.29471907393757846 ) ) ;
#8944 = EDGE_LOOP ( 'NONE', ( #27715, #19323, #4507, #10314 ) ) ;
#8945 = CARTESIAN_POINT ( 'NONE',  ( -2.904412668506657358, 30.27712468694988601, -36.79926976721460363 ) ) ;
#8946 = CARTESIAN_POINT ( 'NONE',  ( -55.25719721206881729, -0.0006290797159227240433, -0.01115102788683359700 ) ) ;
#8947 = ORIENTED_EDGE ( 'NONE', *, *, #20466, .T. ) ;
#8948 = CARTESIAN_POINT ( 'NONE',  ( -20.24399999263414429, 10.36954246768245547, -27.76448601145544259 ) ) ;
#8949 = EDGE_LOOP ( 'NONE', ( #2438, #12654, #156, #9787 ) ) ;
#8950 = CARTESIAN_POINT ( 'NONE',  ( -21.41430102051745266, 29.81033373822138799, 7.777552968935449229 ) ) ;
#8951 = EDGE_CURVE ( 'NONE', #22982, #12673, #21214, .T. ) ;
#8952 = CARTESIAN_POINT ( 'NONE',  ( -55.24198130335446422, 0.009190321388310579431, -0.001391250620101621869 ) ) ;
#8953 = LINE ( 'NONE', #9386, #21260 ) ;
#8954 = CARTESIAN_POINT ( 'NONE',  ( 1.833838850093452599, 132.5643635152042634, -59.02146106674950232 ) ) ;
#8955 = CARTESIAN_POINT ( 'NONE',  ( -20.20700224038492721, 18.19058640100257662, 23.35150625415638714 ) ) ;
#8956 = CARTESIAN_POINT ( 'NONE',  ( -4.780792508754313275, -42.16805077400938728, 25.98388465890126042 ) ) ;
#8957 = DIRECTION ( 'NONE',  ( 1.000000000000000000, -6.938893903907226837E-18, 1.734723475976806709E-18 ) ) ;
#8958 = CARTESIAN_POINT ( 'NONE',  ( -20.21097721712959938, -17.13687106192361398, -24.14932359587282917 ) ) ;
#8959 = CARTESIAN_POINT ( 'NONE',  ( -23.79248802219730052, 30.42578156345387086, -13.25839849636368584 ) ) ;
#8960 = EDGE_LOOP ( 'NONE', ( #22889, #4038, #15582, #19998 ) ) ;
#8961 = ORIENTED_EDGE ( 'NONE', *, *, #9836, .T. ) ;
#8962 = CARTESIAN_POINT ( 'NONE',  ( -1.464342487929851222, 44.64187261869797396, 11.94843286121871273 ) ) ;
#8963 = CARTESIAN_POINT ( 'NONE',  ( -1.583189561560255143, -29.24830400313138767, 36.01941156322820348 ) ) ;
#8964 = VERTEX_POINT ( 'NONE', #17715 ) ;
#8965 = EDGE_LOOP ( 'NONE', ( #8085, #11186, #17162, #17348 ) ) ;
#8966 = ORIENTED_EDGE ( 'NONE', *, *, #24876, .T. ) ;
#8967 = CARTESIAN_POINT ( 'NONE',  ( 55.49584447822657296, 70.91003759562315167, 15.34602024131312170 ) ) ;
#8968 = CARTESIAN_POINT ( 'NONE',  ( 1.831572820252009626, -107.1759352627512811, 97.82994539998347250 ) ) ;
#8969 = ORIENTED_EDGE ( 'NONE', *, *, #27996, .F. ) ;
#8970 = CARTESIAN_POINT ( 'NONE',  ( 13.36082413113063083, 127.3428651193248271, 84.67697637120454601 ) ) ;
#8971 = CARTESIAN_POINT ( 'NONE',  ( -1.619063947482197729, -46.30105812165550105, -2.489035965909997206 ) ) ;
#8972 = EDGE_CURVE ( 'NONE', #4229, #18216, #7915, .T. ) ;
#8973 = CARTESIAN_POINT ( 'NONE',  ( 2.063896406836605024, -142.3682421260909337, 28.88716984836274193 ) ) ;
#8974 = ADVANCED_FACE ( 'NONE', ( #9090 ), #11429, .F. ) ;
#8975 = CARTESIAN_POINT ( 'NONE',  ( -16.86833981943426508, 38.94907963570754106, 20.94590537750566028 ) ) ;
#8976 = CARTESIAN_POINT ( 'NONE',  ( 13.84597867724978038, 4.782757490007880641, -146.6243035057531756 ) ) ;
#8977 = CARTESIAN_POINT ( 'NONE',  ( 2.430230287190592531, -144.5585181921887283, 16.65331920325692039 ) ) ;
#8978 = ADVANCED_FACE ( 'NONE', ( #16281 ), #13263, .F. ) ;
#8979 = CARTESIAN_POINT ( 'NONE',  ( 25.69398547355841345, -65.78402800526225747, 91.80679989327114754 ) ) ;
#8980 = VECTOR ( 'NONE', #14300, 999.9999999999998863 ) ;
#8981 = CARTESIAN_POINT ( 'NONE',  ( 109.1586059443104944, 0.001014167950280784247, -0.007001002073871750823 ) ) ;
#8982 = CARTESIAN_POINT ( 'NONE',  ( -2.265401668238151256, -2.645701981445478079, 46.93990709177546705 ) ) ;
#8983 = VERTEX_POINT ( 'NONE', #4079 ) ;
#8984 = ORIENTED_EDGE ( 'NONE', *, *, #9132, .F. ) ;
#8985 = DIRECTION ( 'NONE',  ( 0.000000000000000000, 5.223019709708233256E-21, -1.000000000000000000 ) ) ;
#8986 = CARTESIAN_POINT ( 'NONE',  ( -1.044557008772710960, 36.05793264791386576, 28.22896138707331204 ) ) ;
#8987 = CARTESIAN_POINT ( 'NONE',  ( 10.93730112725986281, -149.7554878793150408, 20.69552240458288850 ) ) ;
#8988 = CARTESIAN_POINT ( 'NONE',  ( -2.265401668238146815, 11.98901689611106036, 45.46007138824028004 ) ) ;
#8989 = CARTESIAN_POINT ( 'NONE',  ( 2.430230287190589422, -71.49654683843598946, 126.7388733285342823 ) ) ;
#8990 = ORIENTED_EDGE ( 'NONE', *, *, #25404, .F. ) ;
#8991 = CARTESIAN_POINT ( 'NONE',  ( -55.24340739397742084, -0.003826481709803442217, 0.009386184976286439385 ) ) ;
#8992 = ORIENTED_EDGE ( 'NONE', *, *, #9532, .T. ) ;
#8993 = CARTESIAN_POINT ( 'NONE',  ( -1.048996300304511298, 43.31387123529979277, -14.87787369922182990 ) ) ;
#8994 = CARTESIAN_POINT ( 'NONE',  ( 1.833485406944057594, -29.64752363041639782, 142.0485807715645024 ) ) ;
#8995 = ORIENTED_EDGE ( 'NONE', *, *, #12407, .T. ) ;
#8996 = VERTEX_POINT ( 'NONE', #17181 ) ;
#8997 = CARTESIAN_POINT ( 'NONE',  ( 1.833485406944043827, -58.53321471326791681, -132.7804117027893938 ) ) ;
#8999 = ORIENTED_EDGE ( 'NONE', *, *, #21640, .F. ) ;
#8998 = B_SPLINE_CURVE_WITH_KNOTS ( 'NONE', 3,
 ( #20381, #9024, #17786, #15611 ),
 .UNSPECIFIED., .F., .F.,
 ( 4, 4 ),
 ( 0.000000000000000000, 0.008383560773332706870 ),
 .UNSPECIFIED. ) ;
#9000 = CARTESIAN_POINT ( 'NONE',  ( 109.1589550718175161, 0.007008495014555480088, 0.002874971999837445946 ) ) ;
#9001 = ORIENTED_EDGE ( 'NONE', *, *, #7705, .F. ) ;
#9002 = CARTESIAN_POINT ( 'NONE',  ( 25.64660436782533282, 66.83584345385925474, 91.00479974714288289 ) ) ;
#9003 = EDGE_CURVE ( 'NONE', #12622, #25271, #28386, .T. ) ;
#9004 = CARTESIAN_POINT ( 'NONE',  ( 10.93730112725932813, 146.7718404940640085, 36.23586118136551448 ) ) ;
#9005 = B_SPLINE_CURVE_WITH_KNOTS ( 'NONE', 3,
 ( #11944, #11660, #13663, #17832, #2583, #11367 ),
 .UNSPECIFIED., .F., .F.,
 ( 4, 2, 4 ),
 ( 0.000000000000000000, 0.0004335184443140274431, 0.0008670368886280548863 ),
 .UNSPECIFIED. ) ;
#9006 = EDGE_CURVE ( 'NONE', #9151, #26384, #7832, .T. ) ;
#9007 = CARTESIAN_POINT ( 'NONE',  ( 1.832998868059890096, -132.7810136645742034, 58.53348008137602676 ) ) ;
#9008 = CARTESIAN_POINT ( 'NONE',  ( 25.64681081121879203, 75.86069728269103507, -83.63051021305824406 ) ) ;
#9009 = EDGE_CURVE ( 'NONE', #17579, #27510, #10562, .T. ) ;
#9010 = CARTESIAN_POINT ( 'NONE',  ( 1.832998868059890096, -97.49378069860867413, 107.4798986104856908 ) ) ;
#9011 = CARTESIAN_POINT ( 'NONE',  ( -7.078251931573406708, -44.92740138729184451, -26.33626633876207634 ) ) ;
#9012 = CARTESIAN_POINT ( 'NONE',  ( 109.1586059443104944, -0.005555961672780091939, -0.004378796245583014765 ) ) ;
#9013 = DIRECTION ( 'NONE',  ( 0.000000000000000000, 0.000000000000000000, -1.000000000000000000 ) ) ;
#9014 = CARTESIAN_POINT ( 'NONE',  ( -20.20700224038492721, -29.58392382092674211, -0.9908225410477480288 ) ) ;
#9015 = CARTESIAN_POINT ( 'NONE',  ( 25.64708228042120908, -56.48974615488991446, 97.76433875577625088 ) ) ;
#9016 = VERTEX_POINT ( 'NONE', #25967 ) ;
#9017 = CARTESIAN_POINT ( 'NONE',  ( 10.93730112725996229, -10.89264110824889364, -150.7858122213663989 ) ) ;
#9018 = CARTESIAN_POINT ( 'NONE',  ( -1.583189561560255143, -38.94740041318274848, 25.21827308671275247 ) ) ;
#9019 = CARTESIAN_POINT ( 'NONE',  ( -4.162674018437154899, -48.79210541969629844, -3.424137510344775759 ) ) ;
#9020 = CARTESIAN_POINT ( 'NONE',  ( 25.64660436782560637, 91.00479974714322395, -66.83584345385810366 ) ) ;
#9021 = CARTESIAN_POINT ( 'NONE',  ( 25.64699802086722968, -35.11755197949763385, -107.3112355540544769 ) ) ;
#9022 = CARTESIAN_POINT ( 'NONE',  ( -1.113548883309548376, 45.82026503946953255, 1.968251867499028585 ) ) ;
#9023 = DIRECTION ( 'NONE',  ( -1.000000000000000000, -0.000000000000000000, -0.000000000000000000 ) ) ;
#9024 = CARTESIAN_POINT ( 'NONE',  ( 28.37599760073042532, -37.15642189426477415, 108.5491283158100657 ) ) ;
#9025 = EDGE_LOOP ( 'NONE', ( #3817, #7738, #8669, #5846 ) ) ;
#9026 = CARTESIAN_POINT ( 'NONE',  ( 109.1592201516379674, 0.004368284148525261590, -0.006536841731962014269 ) ) ;
#9027 = CARTESIAN_POINT ( 'NONE',  ( 1.833721034905616776, -96.83259691102576028, 108.0754384393931673 ) ) ;
#9028 = ORIENTED_EDGE ( 'NONE', *, *, #8210, .F. ) ;
#9029 = CARTESIAN_POINT ( 'NONE',  ( -9.156249394959713683, -9.022661520477402775, 53.74753343182710807 ) ) ;
#9030 = EDGE_CURVE ( 'NONE', #15929, #25022, #26010, .T. ) ;
#9031 = EDGE_LOOP ( 'NONE', ( #11342, #19564, #5917, #23886 ) ) ;
#9032 = B_SPLINE_CURVE_WITH_KNOTS ( 'NONE', 3,
 ( #22730, #11777, #824, #17938 ),
 .UNSPECIFIED., .F., .F.,
 ( 4, 4 ),
 ( 0.000000000000000000, 0.01077107196513850222 ),
 .UNSPECIFIED. ) ;
#9033 = CARTESIAN_POINT ( 'NONE',  ( 55.79472521941426777, -53.57698701322181023, -49.22042574086480471 ) ) ;
#9034 = EDGE_CURVE ( 'NONE', #1898, #10065, #28378, .T. ) ;
#9035 = VERTEX_POINT ( 'NONE', #8272 ) ;
#9036 = CARTESIAN_POINT ( 'NONE',  ( -20.47566262905010603, 28.85746289809577547, -7.708089517695290382 ) ) ;
#9037 = ADVANCED_FACE ( 'NONE', ( #1772 ), #11265, .F. ) ;
#9038 = CARTESIAN_POINT ( 'NONE',  ( 25.64681081121879203, -34.49579773461859133, 107.5125461021401492 ) ) ;
#9039 = CARTESIAN_POINT ( 'NONE',  ( 25.64700659047696263, 23.25292178500362894, 110.4909389345859694 ) ) ;
#9040 = CARTESIAN_POINT ( 'NONE',  ( -10.86508079875781263, 9.118642906269942117, 50.32133009257457701 ) ) ;
#9041 = FACE_OUTER_BOUND ( 'NONE', #10898, .T. ) ;
#9042 = ORIENTED_EDGE ( 'NONE', *, *, #16075, .T. ) ;
#9043 = CARTESIAN_POINT ( 'NONE',  ( -20.20700224038492365, 10.08426345511628597, 27.82980252387807951 ) ) ;
#9044 = EDGE_CURVE ( 'NONE', #9116, #8689, #5047, .T. ) ;
#9045 = CARTESIAN_POINT ( 'NONE',  ( -21.41430102051744910, -7.777552968935554034, 29.81033373822135246 ) ) ;
#9046 = CARTESIAN_POINT ( 'NONE',  ( -55.24198130335446422, -0.004163123460805480056, 0.008310594958150618883 ) ) ;
#9047 = FACE_OUTER_BOUND ( 'NONE', #21916, .T. ) ;
#9048 = ORIENTED_EDGE ( 'NONE', *, *, #26196, .F. ) ;
#9049 = VERTEX_POINT ( 'NONE', #18751 ) ;
#9050 = ORIENTED_EDGE ( 'NONE', *, *, #21119, .F. ) ;
#9051 = DIRECTION ( 'NONE',  ( -0.7563875759206387661, -0.5078650950445656731, 0.4122509917856767570 ) ) ;
#9052 = CARTESIAN_POINT ( 'NONE',  ( -1.239374126674604337, 45.98822239537607004, 2.406737988131282702 ) ) ;
#9053 = CARTESIAN_POINT ( 'NONE',  ( 25.64681081121880624, -23.88203588908156760, 110.3564950173080916 ) ) ;
#9054 = CARTESIAN_POINT ( 'NONE',  ( -4.162674018437141576, 48.79210541969627712, 3.424137510345119484 ) ) ;
#9055 = DIRECTION ( 'NONE',  ( 0.000000000000000000, 0.000000000000000000, 1.000000000000000000 ) ) ;
#9056 = CARTESIAN_POINT ( 'NONE',  ( -28.13707043255157103, 12.83104814250454062, -18.96624908365850359 ) ) ;
#9057 = ORIENTED_EDGE ( 'NONE', *, *, #18420, .T. ) ;
#9058 = CARTESIAN_POINT ( 'NONE',  ( -2.911734481061402757, 47.57875121082948766, -2.802366807346352129 ) ) ;
#9059 = DIRECTION ( 'NONE',  ( 0.000000000000000000, 5.223019709707975211E-21, -1.000000000000000000 ) ) ;
#9060 = CARTESIAN_POINT ( 'NONE',  ( 109.1592201516379674, -0.006649399203953420406, -0.004194960840980667231 ) ) ;
#9061 = CARTESIAN_POINT ( 'NONE',  ( 13.36082413113061307, 152.6206443696329984, -9.660980093453126472 ) ) ;
#9062 = CARTESIAN_POINT ( 'NONE',  ( -28.13707043255157103, -21.52861750560944998, -7.802116958608919184 ) ) ;
#9063 = VERTEX_POINT ( 'NONE', #25241 ) ;
#9064 = CARTESIAN_POINT ( 'NONE',  ( 2.430230287190572103, -74.01081053031188617, 125.2872625092160064 ) ) ;
#9065 = CARTESIAN_POINT ( 'NONE',  ( -20.38016308990358638, 18.69911008768368532, 23.16952666206563549 ) ) ;
#9066 = CARTESIAN_POINT ( 'NONE',  ( 26.11404676487259024, -90.92995828888244603, 67.46175819463337575 ) ) ;
#9067 = ORIENTED_EDGE ( 'NONE', *, *, #6446, .T. ) ;
#9068 = ORIENTED_EDGE ( 'NONE', *, *, #7854, .F. ) ;
#9069 = ORIENTED_EDGE ( 'NONE', *, *, #7970, .T. ) ;
#9070 = EDGE_CURVE ( 'NONE', #2795, #14713, #1929, .T. ) ;
#9071 = CARTESIAN_POINT ( 'NONE',  ( 109.1778270068192853, 0.009177562596833046746, 0.001591747944966680336 ) ) ;
#9072 = CARTESIAN_POINT ( 'NONE',  ( 32.73300124599736449, -114.2056417606550127, 28.19767303745571496 ) ) ;
#9073 = CARTESIAN_POINT ( 'NONE',  ( -28.41354790283022069, 14.62505768302827036, 18.00456980371883731 ) ) ;
#9074 = EDGE_CURVE ( 'NONE', #11142, #5234, #8514, .T. ) ;
#9075 = VERTEX_POINT ( 'NONE', #14431 ) ;
#9076 = CARTESIAN_POINT ( 'NONE',  ( -4.780792508754314163, 32.07473752860781246, -37.74278713234406979 ) ) ;
#9077 =( BOUNDED_SURFACE ( )  B_SPLINE_SURFACE ( 3, 1, ( 
 ( #4388, #26263 ),
 ( #4522, #6558 ),
 ( #22085, #15310 ),
 ( #24561, #2353 ) ),
 .UNSPECIFIED., .F., .F., .F. ) 
 B_SPLINE_SURFACE_WITH_KNOTS ( ( 4, 4 ),
 ( 2, 2 ),
 ( 0.000000000000000000, 1.000000000000000000 ),
 ( 0.000000000000000000, 1.000000000000000000 ),
 .UNSPECIFIED. ) 
 GEOMETRIC_REPRESENTATION_ITEM ( )  RATIONAL_B_SPLINE_SURFACE ( (
 ( 1.000000000000000000, 1.000000000000000000),
 ( 0.9934239774497838349, 0.8357310067453913582),
 ( 0.9934239774497838349, 0.8357310067453913582),
 ( 1.000000000000000000, 1.000000000000000000) ) ) 
 REPRESENTATION_ITEM ( '' )  SURFACE ( )  );
#9078 = CARTESIAN_POINT ( 'NONE',  ( -1.049817751779876351, -0.5106138415323642210, 45.79652915392416190 ) ) ;
#9079 = ORIENTED_EDGE ( 'NONE', *, *, #6252, .F. ) ;
#9080 = EDGE_LOOP ( 'NONE', ( #315, #22581, #19116, #3948 ) ) ;
#9081 = CARTESIAN_POINT ( 'NONE',  ( 1.833691583653521695, 142.0122737882511785, -29.82175144857958671 ) ) ;
#9082 = CARTESIAN_POINT ( 'NONE',  ( -1.619063947482201282, 43.26576862488434472, -16.67502769180576649 ) ) ;
#9083 = CARTESIAN_POINT ( 'NONE',  ( 1.833206308920112049, -145.1075835660717246, -0.7447049373426916086 ) ) ;
#9084 = FACE_OUTER_BOUND ( 'NONE', #24749, .T. ) ;
#9085 = CARTESIAN_POINT ( 'NONE',  ( 25.64681081121879203, 56.09509703373343115, 97.99105938547943140 ) ) ;
#9086 = CARTESIAN_POINT ( 'NONE',  ( -24.53239521893626218, 33.71193723315153790, 3.868435622621383629 ) ) ;
#9087 = CARTESIAN_POINT ( 'NONE',  ( 2.433796855181233454, -133.5135467655514390, -57.85512797798025275 ) ) ;
#9088 = CARTESIAN_POINT ( 'NONE',  ( -4.162674018437135359, -25.90909455705140729, -41.48630000627045433 ) ) ;
#9089 = CARTESIAN_POINT ( 'NONE',  ( -25.21435515916043713, -31.17620025257576799, 15.02493970636179377 ) ) ;
#9090 = FACE_OUTER_BOUND ( 'NONE', #21514, .T. ) ;
#9091 = CARTESIAN_POINT ( 'NONE',  ( 1.834118845439484335, 96.96525081350000619, 107.9567937753796514 ) ) ;
#9092 = CARTESIAN_POINT ( 'NONE',  ( 28.37603512858351706, -10.20681926544442319, 114.2774673387026070 ) ) ;
#9093 = VERTEX_POINT ( 'NONE', #3490 ) ;
#9094 = ORIENTED_EDGE ( 'NONE', *, *, #23582, .F. ) ;
#9095 = CARTESIAN_POINT ( 'NONE',  ( -55.24390624410018802, 0.009374879212971231821, -0.004572280736701976080 ) ) ;
#9096 = CARTESIAN_POINT ( 'NONE',  ( 25.64660436782546071, 107.2041192742820783, -35.44263474731832986 ) ) ;
#9097 = ORIENTED_EDGE ( 'NONE', *, *, #5338, .T. ) ;
#9098 = ORIENTED_EDGE ( 'NONE', *, *, #13247, .F. ) ;
#9099 = ORIENTED_EDGE ( 'NONE', *, *, #19572, .F. ) ;
#9100 = CARTESIAN_POINT ( 'NONE',  ( 25.64681081121880624, -75.24277141833435678, -84.18689316040122606 ) ) ;
#9101 = ADVANCED_FACE ( 'NONE', ( #23935 ), #7244, .F. ) ;
#9102 = CARTESIAN_POINT ( 'NONE',  ( 1.833485406944057594, -145.1085452359073429, 0.5339064996879626657 ) ) ;
#9103 = EDGE_CURVE ( 'NONE', #21211, #10905, #16030, .T. ) ;
#9104 = CARTESIAN_POINT ( 'NONE',  ( 109.1587776205901861, -0.007186028091168167320, -0.001442274044995771765 ) ) ;
#9105 = EDGE_CURVE ( 'NONE', #26503, #5673, #17424, .T. ) ;
#9106 = B_SPLINE_CURVE_WITH_KNOTS ( 'NONE', 3,
 ( #23007, #27577, #3838, #25724 ),
 .UNSPECIFIED., .F., .F.,
 ( 4, 4 ),
 ( 3.348019117447978055E-16, 0.01077107486149846138 ),
 .UNSPECIFIED. ) ;
#9107 = CARTESIAN_POINT ( 'NONE',  ( -20.20700224038492721, 29.58392382092673500, -0.9908225410479557516 ) ) ;
#9108 = CARTESIAN_POINT ( 'NONE',  ( 2.433796855181233454, 43.58222566461826375, -138.8296532063083646 ) ) ;
#9109 = CARTESIAN_POINT ( 'NONE',  ( -8.786685647604931759, 47.14957014837394667, 25.35688121747446999 ) ) ;
#9110 = CARTESIAN_POINT ( 'NONE',  ( -20.20700224038492721, 24.51628800869048419, -16.58740185276719359 ) ) ;
#9111 = CARTESIAN_POINT ( 'NONE',  ( 5.340103556456435641, -126.5279493230354859, -75.71042922800671704 ) ) ;
#9112 = CARTESIAN_POINT ( 'NONE',  ( -4.780792508754321268, -45.80716263181250980, -18.84172549606854119 ) ) ;
#9113 = CARTESIAN_POINT ( 'NONE',  ( 2.430230287190572103, -125.2872625092157364, -74.01081053031231249 ) ) ;
#9114 = CIRCLE ( 'NONE', #3591, 151.1787379149930359 ) ;
#9115 = CARTESIAN_POINT ( 'NONE',  ( -4.780792508754334591, -3.764354093953240277, 49.38761389561005188 ) ) ;
#9116 = VERTEX_POINT ( 'NONE', #15259 ) ;
#9118 = CARTESIAN_POINT ( 'NONE',  ( 10.93730112725939030, 136.0306644680981947, 65.95960219663135149 ) ) ;
#9117 = FACE_OUTER_BOUND ( 'NONE', #27067, .T. ) ;
#9119 = CARTESIAN_POINT ( 'NONE',  ( 1.833721034905652081, -144.3516387774751024, -14.81406766076082171 ) ) ;
#9120 = CARTESIAN_POINT ( 'NONE',  ( 60.46576798286869803, -12.50000000000000000, 1.048913872128491071E-16 ) ) ;
#9121 = CARTESIAN_POINT ( 'NONE',  ( -55.24390624410018802, -0.01027195578987734684, 0.001811362924359352471 ) ) ;
#9122 = CARTESIAN_POINT ( 'NONE',  ( 26.28373643307409679, -82.21796085350716510, 97.52903534490833692 ) ) ;
#9123 = EDGE_CURVE ( 'NONE', #1609, #3680, #11257, .T. ) ;
#9124 = VERTEX_POINT ( 'NONE', #26209 ) ;
#9125 = CARTESIAN_POINT ( 'NONE',  ( 1.833691583653536572, -14.81406002961217894, -144.3515375443196262 ) ) ;
#9126 = ORIENTED_EDGE ( 'NONE', *, *, #16929, .T. ) ;
#9127 = CARTESIAN_POINT ( 'NONE',  ( -20.47566338032520861, -29.82700953060484395, 1.586617869344197018 ) ) ;
#9128 = CARTESIAN_POINT ( 'NONE',  ( -25.21435515916043357, -6.169479169075226643, 34.05351380035340014 ) ) ;
#9129 = VERTEX_POINT ( 'NONE', #6102 ) ;
#9130 = ORIENTED_EDGE ( 'NONE', *, *, #7457, .F. ) ;
#9131 = CARTESIAN_POINT ( 'NONE',  ( -28.41354790283022069, -14.62505768302787779, 18.00456980371915705 ) ) ;
#9132 = EDGE_CURVE ( 'NONE', #16636, #16438, #4361, .T. ) ;
#9133 = EDGE_LOOP ( 'NONE', ( #20492, #23929, #19132, #16760 ) ) ;
#9134 = CARTESIAN_POINT ( 'NONE',  ( -20.90916690077963835, -38.93431874629077782, -7.054312691028836291 ) ) ;
#9135 = VERTEX_POINT ( 'NONE', #2159 ) ;
#9136 = EDGE_CURVE ( 'NONE', #14557, #18539, #8803, .T. ) ;
#9137 = CARTESIAN_POINT ( 'NONE',  ( -24.53237795827026346, 16.68575684089495326, -29.54731592868563439 ) ) ;
#9138 = AXIS2_PLACEMENT_3D ( 'NONE', #10321, #19078, #21371 ) ;
#9139 = DIRECTION ( 'NONE',  ( -1.000000000000000000, -0.000000000000000000, -0.000000000000000000 ) ) ;
#9140 = CARTESIAN_POINT ( 'NONE',  ( -8.786685647604896232, 23.24040270374459993, 48.22796981442743913 ) ) ;
#9141 = CARTESIAN_POINT ( 'NONE',  ( -7.711401346138408108, 51.42722225669434266, 10.36923727626067304 ) ) ;
#9142 = DIRECTION ( 'NONE',  ( -1.000000000000000000, -0.000000000000000000, -0.000000000000000000 ) ) ;
#9143 = CARTESIAN_POINT ( 'NONE',  ( -22.34422965417126505, -33.39267070835835227, -17.95715691811035342 ) ) ;
#9144 = CARTESIAN_POINT ( 'NONE',  ( 0.000000000000000000, 9.797174393178826052E-15, 80.00000000000000000 ) ) ;
#9145 = CARTESIAN_POINT ( 'NONE',  ( -22.23342874802669300, 20.31166691703127114, -24.24669006619380696 ) ) ;
#9146 = CARTESIAN_POINT ( 'NONE',  ( 1.833485406944057594, 125.4007332306555895, -73.01664920992834595 ) ) ;
#9147 = SURFACE_SIDE_STYLE ('',( #20794 ) ) ;
#9148 = CARTESIAN_POINT ( 'NONE',  ( 109.1586900883932856, 0.007002774699553659596, -0.001385221016536877401 ) ) ;
#9150 = CARTESIAN_POINT ( 'NONE',  ( -4.178947244162628749, 18.28784278438515543, 45.38689110596700260 ) ) ;
#9149 = CARTESIAN_POINT ( 'NONE',  ( -21.81686047589425570, 33.92779429964205917, -18.24499610240053116 ) ) ;
#9151 = VERTEX_POINT ( 'NONE', #19309 ) ;
#9152 = CARTESIAN_POINT ( 'NONE',  ( 1.833485406944043827, -45.34878176254329674, 137.8414413349084100 ) ) ;
#9153 = CARTESIAN_POINT ( 'NONE',  ( 25.73574536432414206, 110.6664861019686725, -22.69874377039331392 ) ) ;
#9154 = B_SPLINE_CURVE_WITH_KNOTS ( 'NONE', 3,
 ( #20498, #786, #9293, #3093, #20640, #27257, #7145, #3231 ),
 .UNSPECIFIED., .F., .F.,
 ( 4, 2, 2, 4 ),
 ( 0.000000000000000000, 0.002761524886576637201, 0.005523049773153274403, 0.01104609954630654707 ),
 .UNSPECIFIED. ) ;
#9155 = LINE ( 'NONE', #13612, #24979 ) ;
#9156 = ORIENTED_EDGE ( 'NONE', *, *, #24151, .F. ) ;
#9157 = B_SPLINE_CURVE_WITH_KNOTS ( 'NONE', 3,
 ( #1283, #25190, #27906, #11943, #21289, #25341, #18566, #16968, #1571, #12232, #8078, #27334, #8200 ),
 .UNSPECIFIED., .F., .F.,
 ( 4, 3, 3, 3, 4 ),
 ( 8.673617379884035472E-18, 0.0007657099931970579596, 0.001531419946797923492, 0.002296279302920159471, 0.003061450627205763737 ),
 .UNSPECIFIED. ) ;
#9158 = CARTESIAN_POINT ( 'NONE',  ( 2.433796855181233454, -86.69855925933894980, -116.8607839509065371 ) ) ;
#9159 = ORIENTED_EDGE ( 'NONE', *, *, #28410, .F. ) ;
#9160 = ADVANCED_FACE ( 'NONE', ( #10964 ), #4277, .F. ) ;
#9161 = EDGE_CURVE ( 'NONE', #6242, #28150, #21515, .T. ) ;
#9162 = CARTESIAN_POINT ( 'NONE',  ( -1.155031165708885199, -35.88345263711027400, 28.62780465193348789 ) ) ;
#9163 = VERTEX_POINT ( 'NONE', #1888 ) ;
#9164 = CARTESIAN_POINT ( 'NONE',  ( -25.21435515916043002, 31.17620025257588523, -15.02493970636157705 ) ) ;
#9165 = EDGE_LOOP ( 'NONE', ( #2260, #7100, #25158, #16083 ) ) ;
#9166 = CARTESIAN_POINT ( 'NONE',  ( 28.37599760073042532, 93.86375353586258541, -65.97809271467041015 ) ) ;
#9167 = B_SPLINE_CURVE_WITH_KNOTS ( 'NONE', 3,
 ( #19883, #26496, #6802, #24361, #2032, #738, #7523, #13830 ),
 .UNSPECIFIED., .F., .F.,
 ( 4, 2, 2, 4 ),
 ( 6.505213034913026604E-19, 0.0002429592666046745376, 0.0004859185332093484246, 0.0009718370664186767914 ),
 .UNSPECIFIED. ) ;
#9168 = CARTESIAN_POINT ( 'NONE',  ( 10.93730112725972781, -71.28103789255033007, 133.3192575531796251 ) ) ;
#9169 = EDGE_LOOP ( 'NONE', ( #10952, #3888, #7067, #4509 ) ) ;
#9170 =( NAMED_UNIT ( * ) PLANE_ANGLE_UNIT ( ) SI_UNIT ( $, .RADIAN. ) );
#9171 = CARTESIAN_POINT ( 'NONE',  ( 30.58324630866341920, -92.47020419020127235, -77.95273942827436997 ) ) ;
#9172 = LINE ( 'NONE', #27736, #6552 ) ;
#9173 = LINE ( 'NONE', #5832, #1622 ) ;
#9174 = CARTESIAN_POINT ( 'NONE',  ( 2.078045971014549723E-18, -1.958632391140620919E-19, 37.50000000000001421 ) ) ;
#9175 = CARTESIAN_POINT ( 'NONE',  ( 25.64681081121879203, -112.9102952884414606, 0.4157506337723927414 ) ) ;
#9176 = ORIENTED_EDGE ( 'NONE', *, *, #1401, .T. ) ;
#9177 = CARTESIAN_POINT ( 'NONE',  ( 25.64703792032469565, 0.1487959541341497549, 112.9111140735909089 ) ) ;
#9178 = CARTESIAN_POINT ( 'NONE',  ( 28.37603512858449761, 48.29936889363955288, 104.0705994281838258 ) ) ;
#9179 = CARTESIAN_POINT ( 'NONE',  ( 32.73300124599732186, 0.000000000000000000, 0.000000000000000000 ) ) ;
#9180 = VERTEX_POINT ( 'NONE', #2453 ) ;
#9181 = VERTEX_POINT ( 'NONE', #22631 ) ;
#9182 = ORIENTED_EDGE ( 'NONE', *, *, #21326, .T. ) ;
#9183 = CARTESIAN_POINT ( 'NONE',  ( -19.53423201713130197, 1.355459634611817678E-16, -3.388649086529544194E-17 ) ) ;
#9184 = DIRECTION ( 'NONE',  ( 0.5914120900931444380, 0.6570486713847274451, -0.4674599267565326399 ) ) ;
#9185 = CARTESIAN_POINT ( 'NONE',  ( -55.24390624410018802, -0.004896917417131185259, 0.009209468562452437224 ) ) ;
#9186 = CARTESIAN_POINT ( 'NONE',  ( -1.049817751779889008, 0.5106138415326839652, -45.79652915392414769 ) ) ;
#9187 = CARTESIAN_POINT ( 'NONE',  ( 1.833838850855499691, 144.3055354793886238, 15.25659494068155375 ) ) ;
#9188 = CARTESIAN_POINT ( 'NONE',  ( 25.73574536432413851, -103.5288236655399174, 45.21157800100269242 ) ) ;
#9189 = CARTESIAN_POINT ( 'NONE',  ( 26.11404676487257603, 47.08215554553518700, 102.9690087468803341 ) ) ;
#9190 = ORIENTED_EDGE ( 'NONE', *, *, #16402, .T. ) ;
#9191 = CARTESIAN_POINT ( 'NONE',  ( 6.224689322667647851, 134.1951906609247658, -62.55544044765115785 ) ) ;
#9192 = CARTESIAN_POINT ( 'NONE',  ( 1.832998868059858122, 132.3466930259802155, -59.50898020732380189 ) ) ;
#9193 = CARTESIAN_POINT ( 'NONE',  ( 1.833485406944043827, -58.53321471326791681, -132.7804117027893938 ) ) ;
#9194 = ADVANCED_FACE ( 'NONE', ( #17711 ), #17148, .F. ) ;
#9195 = CARTESIAN_POINT ( 'NONE',  ( -55.24198130335446422, 0.006527480770974009895, 0.006617369590171991688 ) ) ;
#9196 = ADVANCED_FACE ( 'NONE', ( #4769 ), #4673, .F. ) ;
#9197 = DIRECTION ( 'NONE',  ( 0.000000000000000000, 0.000000000000000000, 1.000000000000000000 ) ) ;
#9198 = CIRCLE ( 'NONE', #25293, 117.6351876552689504 ) ;
#9199 = ORIENTED_EDGE ( 'NONE', *, *, #28410, .T. ) ;
#9200 = B_SPLINE_CURVE_WITH_KNOTS ( 'NONE', 3,
 ( #26785, #20312, #7099, #15859 ),
 .UNSPECIFIED., .F., .F.,
 ( 4, 4 ),
 ( 0.000000000000000000, 0.01077107196513847273 ),
 .UNSPECIFIED. ) ;
#9201 = FACE_OUTER_BOUND ( 'NONE', #14347, .T. ) ;
#9202 = ORIENTED_EDGE ( 'NONE', *, *, #14221, .F. ) ;
#9204 = EDGE_CURVE ( 'NONE', #17261, #25984, #11042, .T. ) ;
#9203 = CARTESIAN_POINT ( 'NONE',  ( 1.833485406944043827, 96.69979900902167458, 108.1939177044929323 ) ) ;
#9205 = CARTESIAN_POINT ( 'NONE',  ( -1.583189561560253589, 25.21827308671232259, -38.94740041318303270 ) ) ;
#9206 = ORIENTED_EDGE ( 'NONE', *, *, #22999, .F. ) ;
#9207 = EDGE_CURVE ( 'NONE', #1068, #23545, #4470, .T. ) ;
#9208 = ORIENTED_EDGE ( 'NONE', *, *, #18279, .F. ) ;
#9209 = ORIENTED_EDGE ( 'NONE', *, *, #22369, .F. ) ;
#9210 = CARTESIAN_POINT ( 'NONE',  ( -1.019300379054419947, -42.90269154183439326, -16.06793277091975369 ) ) ;
#9211 = FACE_OUTER_BOUND ( 'NONE', #2879, .T. ) ;
#9212 = DIRECTION ( 'NONE',  ( 0.7071067811865485719, 0.000000000000000000, -0.7071067811865465735 ) ) ;
#9213 = AXIS2_PLACEMENT_3D ( 'NONE', #16805, #27868, #12598 ) ;
#9214 = DIRECTION ( 'NONE',  ( -1.000000000000000000, -0.000000000000000000, -0.000000000000000000 ) ) ;
#9215 = B_SPLINE_CURVE_WITH_KNOTS ( 'NONE', 3,
 ( #26932, #15997, #7375, #22353, #12226, #16697, #14377, #20031, #22498, #13554, #745, #312, #18287 ),
 .UNSPECIFIED., .F., .F.,
 ( 4, 3, 3, 3, 4 ),
 ( 1.250926888277100149E-17, 0.0007657099931970565501, 0.001531419946797910915, 0.002296279302920149062, 0.003061450627205762869 ),
 .UNSPECIFIED. ) ;
#9216 = EDGE_LOOP ( 'NONE', ( #20684, #6243, #23224, #28029 ) ) ;
#9217 = CARTESIAN_POINT ( 'NONE',  ( 1.833485406944043827, 14.63699153649552365, -144.3694338680883789 ) ) ;
#9218 = B_SPLINE_CURVE_WITH_KNOTS ( 'NONE', 3,
 ( #21639, #19481, #7387, #18458, #20476, #20040 ),
 .UNSPECIFIED., .F., .F.,
 ( 4, 2, 4 ),
 ( 1.815771614269358398E-17, 0.0006311636237756957160, 0.001262327247551373434 ),
 .UNSPECIFIED. ) ;
#9219 = CARTESIAN_POINT ( 'NONE',  ( -20.57838717382308147, 10.78122205917039977, 27.96569011373074076 ) ) ;
#9220 = CARTESIAN_POINT ( 'NONE',  ( -7.078251931573406708, 38.93060825814230697, -34.59014398252930533 ) ) ;
#9221 = VERTEX_POINT ( 'NONE', #20733 ) ;
#9222 = AXIS2_PLACEMENT_3D ( 'NONE', #12264, #25526, #12129 ) ;
#9223 = CARTESIAN_POINT ( 'NONE',  ( -24.53239521893626218, 33.71193723315153790, 3.868435622621383629 ) ) ;
#9224 = VERTEX_POINT ( 'NONE', #16277 ) ;
#9225 = PLANE ( 'NONE',  #17998 ) ;
#9226 = CARTESIAN_POINT ( 'NONE',  ( 13.84597867724974130, -69.17016226638961029, -129.3717503931858062 ) ) ;
#9227 = CARTESIAN_POINT ( 'NONE',  ( -28.13707043255157103, 18.06394523322473944, 14.07296284901312688 ) ) ;
#9228 = CARTESIAN_POINT ( 'NONE',  ( -1.046936909428682894, 15.35929614323726256, 43.14407378092978718 ) ) ;
#9229 = CARTESIAN_POINT ( 'NONE',  ( 32.73300124599738581, -62.10906484417165530, -99.90245962373897726 ) ) ;
#9230 = CARTESIAN_POINT ( 'NONE',  ( 13.36082413113063083, -53.25066407421704895, -143.3553710183994951 ) ) ;
#9231 = CARTESIAN_POINT ( 'NONE',  ( -8.786685647604887350, -38.68584556812326980, -37.00619870957918778 ) ) ;
#9232 = FACE_OUTER_BOUND ( 'NONE', #15746, .T. ) ;
#9233 = EDGE_CURVE ( 'NONE', #710, #14740, #12590, .T. ) ;
#9234 = ADVANCED_FACE ( 'NONE', ( #10253 ), #5550, .F. ) ;
#9235 = CARTESIAN_POINT ( 'NONE',  ( 10.93730112725996051, 20.69552240458543224, -149.7554878793147282 ) ) ;
#9236 = CARTESIAN_POINT ( 'NONE',  ( -8.786685647604855376, -7.199674155859337787, -53.04920435127184675 ) ) ;
#9237 = CARTESIAN_POINT ( 'NONE',  ( -1.045287976400362417, 37.92705037016796155, 25.66401692419947977 ) ) ;
#9238 = ORIENTED_EDGE ( 'NONE', *, *, #17025, .F. ) ;
#9239 = VERTEX_POINT ( 'NONE', #25511 ) ;
#9241 = EDGE_CURVE ( 'NONE', #27092, #24861, #14715, .T. ) ;
#9240 = FACE_OUTER_BOUND ( 'NONE', #24243, .T. ) ;
#9242 = VECTOR ( 'NONE', #17011, 1000.000000000000000 ) ;
#9243 = CARTESIAN_POINT ( 'NONE',  ( -55.24728320129491266, 0.01362040845703433277, 0.005114031043468512429 ) ) ;
#9244 = ORIENTED_EDGE ( 'NONE', *, *, #21254, .F. ) ;
#9245 = CIRCLE ( 'NONE', #21661, 34.60786435723138510 ) ;
#9246 = VERTEX_POINT ( 'NONE', #16564 ) ;
#9247 = ORIENTED_EDGE ( 'NONE', *, *, #17764, .F. ) ;
#9248 = CIRCLE ( 'NONE', #20265, 53.53553390275978785 ) ;
#9249 = LINE ( 'NONE', #24806, #14719 ) ;
#9250 =( BOUNDED_SURFACE ( )  B_SPLINE_SURFACE ( 3, 1, ( 
 ( #5817, #16600 ),
 ( #18468, #11993 ),
 ( #16306, #25392 ),
 ( #9548, #905 ) ),
 .UNSPECIFIED., .F., .F., .F. ) 
 B_SPLINE_SURFACE_WITH_KNOTS ( ( 4, 4 ),
 ( 2, 2 ),
 ( 0.000000000000000000, 1.000000000000000000 ),
 ( 0.000000000000000000, 1.000000000000000000 ),
 .UNSPECIFIED. ) 
 GEOMETRIC_REPRESENTATION_ITEM ( )  RATIONAL_B_SPLINE_SURFACE ( (
 ( 1.000000000000000000, 1.000000000000000000),
 ( 0.7789835883360576307, 0.9689951854195403280),
 ( 0.7789835883360576307, 0.9689951854195403280),
 ( 1.000000000000000000, 1.000000000000000000) ) ) 
 REPRESENTATION_ITEM ( '' )  SURFACE ( )  );
#9251 = CARTESIAN_POINT ( 'NONE',  ( -1.049817751779883457, 43.39729912094399822, 14.63752841325003295 ) ) ;
#9252 = FACE_OUTER_BOUND ( 'NONE', #2648, .T. ) ;
#9253 = CARTESIAN_POINT ( 'NONE',  ( -55.24300891470650754, -0.008142823778061761275, -0.005486913146700541852 ) ) ;
#9254 = CARTESIAN_POINT ( 'NONE',  ( 119.2224693531408519, 70.00000000000000000, -20.00000000000001421 ) ) ;
#9255 = CARTESIAN_POINT ( 'NONE',  ( -1.045287976400362417, 43.05558670614268379, 15.59869763335023229 ) ) ;
#9256 = CARTESIAN_POINT ( 'NONE',  ( -55.24390624410018802, 0.007503127514278223366, 0.007245494385991344682 ) ) ;
#9257 = CONICAL_SURFACE ( 'NONE', #11106, 117.6351876552689504, 0.9945805576725580410 ) ;
#9258 = CARTESIAN_POINT ( 'NONE',  ( 32.73300124599738581, 3.836798148480494497, -117.5726003567928757 ) ) ;
#9259 = CIRCLE ( 'NONE', #11552, 34.60786435723138510 ) ;
#9260 = CARTESIAN_POINT ( 'NONE',  ( 109.1624594426973118, -0.01570508117120619426, -0.002863932759303039303 ) ) ;
#9261 = DIRECTION ( 'NONE',  ( -0.5946245182733607137, -0.4701913299128818169, 0.6521823330502973803 ) ) ;
#9262 = CARTESIAN_POINT ( 'NONE',  ( 8.186469829614306803, -146.7694295239426481, 27.65107825763907812 ) ) ;
#9263 = CARTESIAN_POINT ( 'NONE',  ( -1.583189561560255143, 25.21827308671289103, 38.94740041318266321 ) ) ;
#9264 = CIRCLE ( 'NONE', #15673, 117.6351876552689504 ) ;
#9265 = ORIENTED_EDGE ( 'NONE', *, *, #12850, .F. ) ;
#9266 = CARTESIAN_POINT ( 'NONE',  ( -7.078251931573400491, 44.92740138729166688, -26.33626633876239609 ) ) ;
#9267 = EDGE_CURVE ( 'NONE', #22024, #16670, #23210, .T. ) ;
#9268 = CARTESIAN_POINT ( 'NONE',  ( 2.433796855181219243, 142.0211193075560061, -31.67151202412830813 ) ) ;
#9269 = CARTESIAN_POINT ( 'NONE',  ( 109.1586059443104944, 0.005881369279880096536, 0.003930911098385099153 ) ) ;
#9270 = CARTESIAN_POINT ( 'NONE',  ( -55.24198130335446422, 0.001516807524704581441, 0.009170435128245077103 ) ) ;
#9271 = CARTESIAN_POINT ( 'NONE',  ( -21.41427618760457818, -25.94789270595494202, 16.60878262545447726 ) ) ;
#9272 = VERTEX_POINT ( 'NONE', #14544 ) ;
#9273 = CARTESIAN_POINT ( 'NONE',  ( 1.833809397773857430, -14.99109763364046799, -144.3333383260367953 ) ) ;
#9274 = ORIENTED_EDGE ( 'NONE', *, *, #3506, .T. ) ;
#9276 = EDGE_CURVE ( 'NONE', #7372, #22961, #23349, .T. ) ;
#9275 = CARTESIAN_POINT ( 'NONE',  ( 32.73300124599739291, -108.9684813982485707, -44.31599526638064646 ) ) ;
#9277 = CARTESIAN_POINT ( 'NONE',  ( 30.59141879584289470, -101.9665761624294049, 55.75104644134855647 ) ) ;
#9278 = B_SPLINE_CURVE_WITH_KNOTS ( 'NONE', 3,
 ( #6641, #15107, #17417, #2019, #8649, #2, #13235, #21603, #17557, #2148 ),
 .UNSPECIFIED., .F., .F.,
 ( 4, 3, 3, 4 ),
 ( 6.206335383118182794E-17, 0.0002669559177086440840, 0.0005339118354151246425, 0.001067817517169165117 ),
 .UNSPECIFIED. ) ;
#9279 = EDGE_LOOP ( 'NONE', ( #19221, #8450, #9727, #4153 ) ) ;
#9280 = ADVANCED_FACE ( 'NONE', ( #1447 ), #25769, .T. ) ;
#9281 = CARTESIAN_POINT ( 'NONE',  ( -1.058473599757816963, -28.32531354681309566, -35.99997772736203672 ) ) ;
#9282 = VERTEX_POINT ( 'NONE', #10632 ) ;
#9283 = CARTESIAN_POINT ( 'NONE',  ( -23.77929240705207192, -35.68044874544700207, -6.464423883190233866 ) ) ;
#9284 = B_SPLINE_CURVE_WITH_KNOTS ( 'NONE', 3,
 ( #16791, #5552, #3396, #8283, #23554, #27563 ),
 .UNSPECIFIED., .F., .F.,
 ( 4, 2, 4 ),
 ( 1.389302603484999005E-17, 0.0006311571484585952723, 0.001262314296917176884 ),
 .UNSPECIFIED. ) ;
#9285 = EDGE_LOOP ( 'NONE', ( #10671, #7490, #8432, #19051 ) ) ;
#9286 = VERTEX_POINT ( 'NONE', #6739 ) ;
#9287 = CARTESIAN_POINT ( 'NONE',  ( 30.59141879584290891, -116.1811685142589852, -2.701465575440967548 ) ) ;
#9289 = VECTOR ( 'NONE', #16605, 1000.000000000000114 ) ;
#9288 =( BOUNDED_SURFACE ( )  B_SPLINE_SURFACE ( 3, 1, ( 
 ( #4803, #26385 ),
 ( #19486, #15144 ),
 ( #22066, #13280 ),
 ( #10721, #17316 ) ),
 .UNSPECIFIED., .F., .F., .F. ) 
 B_SPLINE_SURFACE_WITH_KNOTS ( ( 4, 4 ),
 ( 2, 2 ),
 ( 0.000000000000000000, 1.000000000000000000 ),
 ( 0.000000000000000000, 1.000000000000000000 ),
 .UNSPECIFIED. ) 
 GEOMETRIC_REPRESENTATION_ITEM ( )  RATIONAL_B_SPLINE_SURFACE ( (
 ( 1.000000000000000000, 1.000000000000000000),
 ( 0.9956975270656955868, 0.8568959468854907557),
 ( 0.9956975270656955868, 0.8568959468854907557),
 ( 1.000000000000000000, 1.000000000000000000) ) ) 
 REPRESENTATION_ITEM ( '' )  SURFACE ( )  );
#9290 = B_SPLINE_CURVE_WITH_KNOTS ( 'NONE', 3,
 ( #6244, #14994, #8962, #15858, #19888, #24666, #15700, #15992, #2753, #15549 ),
 .UNSPECIFIED., .F., .F.,
 ( 4, 2, 2, 2, 4 ),
 ( 2.168404344971008868E-19, 0.0003346267210630925128, 0.0006692534421261848087, 0.001003880163189277159, 0.001338506884252369401 ),
 .UNSPECIFIED. ) ;
#9291 = CARTESIAN_POINT ( 'NONE',  ( -8.786685647604890903, 52.67761315067286176, -9.545808661480789326 ) ) ;
#9292 = CARTESIAN_POINT ( 'NONE',  ( -1.048171036023497038, -13.17819047681634537, -43.86077206077064261 ) ) ;
#9293 = CARTESIAN_POINT ( 'NONE',  ( -7.711401346138374358, 47.70038152767087780, -21.83927363365046048 ) ) ;
#9294 = CARTESIAN_POINT ( 'NONE',  ( 1.833603222531960508, -72.16916166673654232, -125.8904991419474442 ) ) ;
#9295 = CARTESIAN_POINT ( 'NONE',  ( 109.1586900883932856, -0.006130969560693691131, -0.003656351050324861858 ) ) ;
#9296 = B_SPLINE_CURVE_WITH_KNOTS ( 'NONE', 3,
 ( #15457, #13589, #24408, #2655, #785, #19936, #217, #11439, #498, #22686, #9292, #18051, #4957 ),
 .UNSPECIFIED., .F., .F.,
 ( 4, 3, 3, 3, 4 ),
 ( 6.938893903907227607E-18, 0.0007657099931970527554, 0.001531419946797919806, 0.002296279302920157302, 0.003061450627205762002 ),
 .UNSPECIFIED. ) ;
#9297 = B_SPLINE_CURVE_WITH_KNOTS ( 'NONE', 3,
 ( #22814, #7552, #15883, #11853, #24967, #14002, #16309 ),
 .UNSPECIFIED., .F., .F.,
 ( 4, 3, 4 ),
 ( 6.081733682261733487E-16, 0.02816610861753244405, 0.04000277880656275681 ),
 .UNSPECIFIED. ) ;
#9298 = CARTESIAN_POINT ( 'NONE',  ( 25.65782528836479770, -110.3293115225705492, -24.04194111108980181 ) ) ;
#9299 = CARTESIAN_POINT ( 'NONE',  ( -1.046936909428678675, 25.87632113675161349, -37.78538189376516954 ) ) ;
#9300 = CARTESIAN_POINT ( 'NONE',  ( 109.1586059443104944, 0.005067816690893742551, 0.004935564877218420222 ) ) ;
#9301 = ORIENTED_EDGE ( 'NONE', *, *, #18625, .T. ) ;
#9302 = CARTESIAN_POINT ( 'NONE',  ( -1.239374126674604337, -2.406737988130801309, 45.98822239537608425 ) ) ;
#9304 = CARTESIAN_POINT ( 'NONE',  ( -20.57838717382308147, -16.28767523336139078, -25.16001208503099917 ) ) ;
#9303 = FACE_OUTER_BOUND ( 'NONE', #19439, .T. ) ;
#9305 = ADVANCED_FACE ( 'NONE', ( #24296 ), #26133, .F. ) ;
#9306 = DIRECTION ( 'NONE',  ( 1.000000000000000000, -6.938893903907226837E-18, 1.734723475976806709E-18 ) ) ;
#9307 = CARTESIAN_POINT ( 'NONE',  ( 109.1586059443104944, 0.002622205828279748022, -0.006570129623063777728 ) ) ;
#9308 = FACE_OUTER_BOUND ( 'NONE', #5289, .T. ) ;
#9309 = VECTOR ( 'NONE', #16938, 999.9999999999998863 ) ;
#9310 = ORIENTED_EDGE ( 'NONE', *, *, #26933, .F. ) ;
#9311 = CARTESIAN_POINT ( 'NONE',  ( 2.063896406836605024, 126.4736179849657560, -71.46753739785881976 ) ) ;
#9312 = VECTOR ( 'NONE', #25816, 1000.000000000000114 ) ;
#9313 = CARTESIAN_POINT ( 'NONE',  ( -15.02187109954776290, -45.93032478317472567, -6.234056423739352759 ) ) ;
#9314 = CARTESIAN_POINT ( 'NONE',  ( 109.1587776205901861, 8.330235398536594530E-05, 0.007328861771499511728 ) ) ;
#9315 = VERTEX_POINT ( 'NONE', #26028 ) ;
#9316 = CARTESIAN_POINT ( 'NONE',  ( 32.73300124599734318, 92.86301839380026024, 72.21147546950587071 ) ) ;
#9317 = VERTEX_POINT ( 'NONE', #4556 ) ;
#9318 = CARTESIAN_POINT ( 'NONE',  ( -1.044556982611275497, -15.70482750345265899, -43.01635920718344153 ) ) ;
#9319 = DIRECTION ( 'NONE',  ( 0.000000000000000000, 0.000000000000000000, 1.000000000000000000 ) ) ;
#9320 = ORIENTED_EDGE ( 'NONE', *, *, #2319, .F. ) ;
#9321 = CARTESIAN_POINT ( 'NONE',  ( 25.64703792032472052, -112.9111140735908805, 0.1487959541337554870 ) ) ;
#9322 = ORIENTED_EDGE ( 'NONE', *, *, #4511, .T. ) ;
#9323 = CARTESIAN_POINT ( 'NONE',  ( 1.834118845439484335, 137.9527673765105646, 45.01070051384637338 ) ) ;
#9324 = ORIENTED_EDGE ( 'NONE', *, *, #18126, .T. ) ;
#9325 = CARTESIAN_POINT ( 'NONE',  ( 25.64700659047696973, 103.2418925369179732, -45.71714758798273692 ) ) ;
#9326 = CONICAL_SURFACE ( 'NONE', #18041, 34.60786435723138510, 0.8559913436420825139 ) ;
#9327 = ADVANCED_FACE ( 'NONE', ( #2389, #4140 ), #26573, .F. ) ;
#9328 = CARTESIAN_POINT ( 'NONE',  ( 24.22246935314087324, -90.00000000000005684, 39.99999999999997158 ) ) ;
#9329 = VECTOR ( 'NONE', #9184, 1000.000000000000000 ) ;
#9330 = CARTESIAN_POINT ( 'NONE',  ( 32.73300124599739291, 105.8473486001057466, -51.32617430724801721 ) ) ;
#9331 = DIRECTION ( 'NONE',  ( -0.5914120900931443270, 0.7643865440136140554, -0.2567974902965012296 ) ) ;
#9332 = CARTESIAN_POINT ( 'NONE',  ( -1.583189561560256253, -25.21827308671203838, 38.94740041318321744 ) ) ;
#9333 = CARTESIAN_POINT ( 'NONE',  ( 25.64660436782547848, -112.9095526718342342, 0.5800540083547919279 ) ) ;
#9334 = VERTEX_POINT ( 'NONE', #11048 ) ;
#9335 = B_SPLINE_CURVE_WITH_KNOTS ( 'NONE', 3,
 ( #26654, #9262, #13563, #2480 ),
 .UNSPECIFIED., .F., .F.,
 ( 4, 4 ),
 ( 0.000000000000000000, 0.01077107196513865661 ),
 .UNSPECIFIED. ) ;
#9336 = EDGE_CURVE ( 'NONE', #27723, #20203, #19815, .T. ) ;
#9337 = B_SPLINE_CURVE_WITH_KNOTS ( 'NONE', 3,
 ( #17567, #26355, #4472, #6797, #24356, #20593 ),
 .UNSPECIFIED., .F., .F.,
 ( 4, 2, 4 ),
 ( 0.000000000000000000, 0.0004335151646191496774, 0.0008670303292382993549 ),
 .UNSPECIFIED. ) ;
#9338 = CARTESIAN_POINT ( 'NONE',  ( 24.01988960052051780, -57.17607523395295743, 117.9135177031536585 ) ) ;
#9339 = CARTESIAN_POINT ( 'NONE',  ( 25.87036335909426654, 33.99475147239157025, -107.8283083010000212 ) ) ;
#9340 = CARTESIAN_POINT ( 'NONE',  ( 19.66333377628668799, -116.9853418557808169, -72.72773398758353380 ) ) ;
#9341 = VERTEX_POINT ( 'NONE', #8476 ) ;
#9342 = EDGE_CURVE ( 'NONE', #20822, #13087, #9259, .T. ) ;
#9343 = VERTEX_POINT ( 'NONE', #6455 ) ;
#9344 = EDGE_LOOP ( 'NONE', ( #24665, #11800, #24089, #1962 ) ) ;
#9345 = CARTESIAN_POINT ( 'NONE',  ( -1.583189561560253589, -44.83405390829680215, -11.94859433442884189 ) ) ;
#9346 = CARTESIAN_POINT ( 'NONE',  ( 30.59138290137912364, 44.78723476287443361, -107.2355347544031190 ) ) ;
#9347 = EDGE_CURVE ( 'NONE', #24750, #22385, #24985, .T. ) ;
#9348 = CARTESIAN_POINT ( 'NONE',  ( 32.73300124599738581, 39.98094346392455378, -110.6325518752269517 ) ) ;
#9349 = LINE ( 'NONE', #16235, #16200 ) ;
#9350 = CARTESIAN_POINT ( 'NONE',  ( 26.28373643307406837, -43.35364178852690031, -119.9673604189461429 ) ) ;
#9351 = CARTESIAN_POINT ( 'NONE',  ( -16.86833981943425442, 30.57013526701963713, 31.95666732167528323 ) ) ;
#9352 = EDGE_LOOP ( 'NONE', ( #1308, #15056, #20819, #24039 ) ) ;
#9353 = CARTESIAN_POINT ( 'NONE',  ( 1.833206310202334599, 145.1075835704899930, -0.7447039688730743290 ) ) ;
#9354 = CARTESIAN_POINT ( 'NONE',  ( -1.044556982611275497, -15.70482750345265899, -43.01635920718344153 ) ) ;
#9355 = CARTESIAN_POINT ( 'NONE',  ( 2.430230287190581429, -1.451610819318752688, 145.5073573687466819 ) ) ;
#9356 = CARTESIAN_POINT ( 'NONE',  ( -22.23226125620942284, 11.82389163795251541, 29.33577758406437042 ) ) ;
#9357 = CARTESIAN_POINT ( 'NONE',  ( 25.73574536432414561, -74.99093179013911481, -84.49061642666552530 ) ) ;
#9358 = ORIENTED_EDGE ( 'NONE', *, *, #27894, .T. ) ;
#9359 = FACE_OUTER_BOUND ( 'NONE', #15239, .T. ) ;
#9360 = AXIS2_PLACEMENT_3D ( 'NONE', #20867, #1151, #10372 ) ;
#9361 = AXIS2_PLACEMENT_3D ( 'NONE', #26033, #15487, #19678 ) ;
#9362 = ORIENTED_EDGE ( 'NONE', *, *, #27061, .T. ) ;
#9363 = CARTESIAN_POINT ( 'NONE',  ( -12.94347594948484037, 48.30328466416762723, 6.555928820869474372 ) ) ;
#9364 = CARTESIAN_POINT ( 'NONE',  ( -20.20898977204108604, -0.6607022527615499241, 29.59696883073212703 ) ) ;
#9365 = ORIENTED_EDGE ( 'NONE', *, *, #1533, .F. ) ;
#9366 = VERTEX_POINT ( 'NONE', #19673 ) ;
#9367 = ORIENTED_EDGE ( 'NONE', *, *, #16752, .T. ) ;
#9368 = CARTESIAN_POINT ( 'NONE',  ( 13.36082413113061307, 109.3026516754232773, 106.9547846563639126 ) ) ;
#9369 = CONICAL_SURFACE ( 'NONE', #10743, 34.60786435723138510, 0.8559913436420825139 ) ;
#9370 = CARTESIAN_POINT ( 'NONE',  ( 1.832998868059858122, 96.70023740551121705, 108.1944082009160724 ) ) ;
#9371 = EDGE_CURVE ( 'NONE', #7281, #10842, #22926, .T. ) ;
#9372 = CARTESIAN_POINT ( 'NONE',  ( -25.21435515916043713, 15.02493970636190745, 31.17620025257570759 ) ) ;
#9373 = B_SPLINE_CURVE_WITH_KNOTS ( 'NONE', 3,
 ( #2988, #11330, #7311, #25026, #22573, #26865 ),
 .UNSPECIFIED., .F., .F.,
 ( 4, 2, 4 ),
 ( 1.734723475976807094E-18, 0.0004335184443140250579, 0.0008670368886280483810 ),
 .UNSPECIFIED. ) ;
#9374 = DIRECTION ( 'NONE',  ( 0.000000000000000000, 0.000000000000000000, 1.000000000000000000 ) ) ;
#9375 = ORIENTED_EDGE ( 'NONE', *, *, #28321, .T. ) ;
#9376 = CARTESIAN_POINT ( 'NONE',  ( 5.340103556456504919, -140.9275371673309962, 43.36842540065445917 ) ) ;
#9377 = CARTESIAN_POINT ( 'NONE',  ( 25.64681081121880624, 35.28660243342550729, 107.2555980796242494 ) ) ;
#9378 = DIRECTION ( 'NONE',  ( 0.000000000000000000, 0.000000000000000000, 1.000000000000000000 ) ) ;
#9379 = ORIENTED_EDGE ( 'NONE', *, *, #20905, .T. ) ;
#9380 = EDGE_CURVE ( 'NONE', #17407, #11640, #17524, .T. ) ;
#9381 = ORIENTED_EDGE ( 'NONE', *, *, #27487, .T. ) ;
#9382 = CARTESIAN_POINT ( 'NONE',  ( -21.81686047589426991, -34.70276904128901663, -16.72402253294301744 ) ) ;
#9383 = CARTESIAN_POINT ( 'NONE',  ( -1.539760825549693068, 43.19716078875438825, -16.63252404870369006 ) ) ;
#9384 = CARTESIAN_POINT ( 'NONE',  ( -7.733045908741315699, 52.15131830128827062, 5.980865481988326238 ) ) ;
#9385 = CARTESIAN_POINT ( 'NONE',  ( 6.224689322667647851, 146.9579047224771955, -18.02516478983991988 ) ) ;
#9386 = CARTESIAN_POINT ( 'NONE',  ( 55.49584447822657296, 22.16497542184406200, 69.08290406177587784 ) ) ;
#9387 = FACE_OUTER_BOUND ( 'NONE', #26313, .T. ) ;
#9388 = EDGE_CURVE ( 'NONE', #20199, #4178, #11189, .T. ) ;
#9389 = CARTESIAN_POINT ( 'NONE',  ( 109.1624594426973260, -0.01318243916934109389, 0.009004164758061344864 ) ) ;
#9390 = CARTESIAN_POINT ( 'NONE',  ( -1.058197053496178874, 44.07533330186787168, -12.47644286888530019 ) ) ;
#9391 = CARTESIAN_POINT ( 'NONE',  ( 1.833485406944057594, 142.0485807715645876, 29.64752363041592531 ) ) ;
#9392 = CARTESIAN_POINT ( 'NONE',  ( -1.583189561560255143, -16.68617981233672509, 43.29471907393757846 ) ) ;
#9393 = LINE ( 'NONE', #23217, #21770 ) ;
#9394 = CARTESIAN_POINT ( 'NONE',  ( 26.11404676487259024, -108.0249973236465308, -33.91085499298486639 ) ) ;
#9395 = ORIENTED_EDGE ( 'NONE', *, *, #6227, .F. ) ;
#9396 = CARTESIAN_POINT ( 'NONE',  ( 32.73300124599732186, 0.000000000000000000, 0.000000000000000000 ) ) ;
#9397 = VERTEX_POINT ( 'NONE', #6875 ) ;
#9398 = ORIENTED_EDGE ( 'NONE', *, *, #14588, .T. ) ;
#9399 = VERTEX_POINT ( 'NONE', #15621 ) ;
#9400 = CARTESIAN_POINT ( 'NONE',  ( -1.031422197589716205, 12.69107518035563764, 44.01264471863834160 ) ) ;
#9401 = CARTESIAN_POINT ( 'NONE',  ( -1.050229599974464634, 43.47850826583074735, 14.39582765040416668 ) ) ;
#9402 = CARTESIAN_POINT ( 'NONE',  ( -8.786685647604885574, 6.096987947571466530E-17, -1.524246986892866633E-17 ) ) ;
#9403 = EDGE_CURVE ( 'NONE', #20917, #11289, #2828, .T. ) ;
#9404 = ADVANCED_FACE ( 'NONE', ( #19401 ), #23230, .F. ) ;
#9405 = FACE_OUTER_BOUND ( 'NONE', #21626, .T. ) ;
#9406 = CARTESIAN_POINT ( 'NONE',  ( -20.47566262905010248, -16.24827521404668929, -25.06314747784830388 ) ) ;
#9407 = DIRECTION ( 'NONE',  ( -1.000000000000000000, -0.000000000000000000, -0.000000000000000000 ) ) ;
#9408 = EDGE_CURVE ( 'NONE', #6634, #2788, #17733, .T. ) ;
#9409 = FACE_OUTER_BOUND ( 'NONE', #21153, .T. ) ;
#9410 = CARTESIAN_POINT ( 'NONE',  ( 25.64670758986457244, 112.9099239813695306, 0.4979020485381295269 ) ) ;
#9411 = EDGE_CURVE ( 'NONE', #23363, #16816, #22953, .T. ) ;
#9412 = CARTESIAN_POINT ( 'NONE',  ( 1.833206310202323941, 59.70089235435430197, 132.2594754479307255 ) ) ;
#9413 = CARTESIAN_POINT ( 'NONE',  ( -21.41427618760446094, -1.815001260755626733, 30.75468365310880259 ) ) ;
#9414 = ORIENTED_EDGE ( 'NONE', *, *, #24663, .F. ) ;
#9415 = CARTESIAN_POINT ( 'NONE',  ( -20.21097721712959938, -23.76068428613694294, -17.67178718142850258 ) ) ;
#9416 = CARTESIAN_POINT ( 'NONE',  ( 109.1592201516379674, 0.003661068210037295243, 0.006957642258146931775 ) ) ;
#9417 = LINE ( 'NONE', #20621, #6596 ) ;
#9418 = CARTESIAN_POINT ( 'NONE',  ( -55.24271866751342941, 0.004365563123935787236, 0.008433070970613791573 ) ) ;
#9419 = CARTESIAN_POINT ( 'NONE',  ( 1.833485406944043827, -107.4794113447415924, 97.49333871408656194 ) ) ;
#9420 = ORIENTED_EDGE ( 'NONE', *, *, #27846, .F. ) ;
#9421 = CARTESIAN_POINT ( 'NONE',  ( 1.833838850855489255, -15.07960613928529092, -144.3241377520100173 ) ) ;
#9422 = ORIENTED_EDGE ( 'NONE', *, *, #24664, .F. ) ;
#9423 = CARTESIAN_POINT ( 'NONE',  ( -20.24419206586952313, -29.61012937815440083, 1.282847120831551280 ) ) ;
#9424 = CARTESIAN_POINT ( 'NONE',  ( -55.24271866751342941, -0.009388511352197387999, -0.001425019990782294558 ) ) ;
#9425 = ORIENTED_EDGE ( 'NONE', *, *, #4453, .F. ) ;
#9426 = CARTESIAN_POINT ( 'NONE',  ( -1.464342487929856107, -29.09292098541686755, -35.90631960086405883 ) ) ;
#9427 =( BOUNDED_SURFACE ( )  B_SPLINE_SURFACE ( 3, 1, ( 
 ( #28090, #23521 ),
 ( #1479, #8254 ),
 ( #10287, #21615 ),
 ( #1617, #23670 ) ),
 .UNSPECIFIED., .F., .F., .F. ) 
 B_SPLINE_SURFACE_WITH_KNOTS ( ( 4, 4 ),
 ( 2, 2 ),
 ( 0.000000000000000000, 1.000000000000000000 ),
 ( 0.000000000000000000, 1.000000000000000000 ),
 .UNSPECIFIED. ) 
 GEOMETRIC_REPRESENTATION_ITEM ( )  RATIONAL_B_SPLINE_SURFACE ( (
 ( 1.000000000000000000, 1.000000000000000000),
 ( 0.7789835883360578528, 0.9689951854195403280),
 ( 0.7789835883360578528, 0.9689951854195403280),
 ( 1.000000000000000000, 1.000000000000000000) ) ) 
 REPRESENTATION_ITEM ( '' )  SURFACE ( )  );
#9428 = VERTEX_POINT ( 'NONE', #2837 ) ;
#9429 = ORIENTED_EDGE ( 'NONE', *, *, #4579, .T. ) ;
#9430 = B_SPLINE_CURVE_WITH_KNOTS ( 'NONE', 3,
 ( #18197, #20644, #24715, #5108, #22694, #652, #16189, #5252 ),
 .UNSPECIFIED., .F., .F.,
 ( 4, 2, 2, 4 ),
 ( 0.000000000000000000, 0.0002429588503611278814, 0.0004859177007222557627, 0.0009718354014444947203 ),
 .UNSPECIFIED. ) ;
#9431 = VERTEX_POINT ( 'NONE', #2986 ) ;
#9432 = EDGE_CURVE ( 'NONE', #6115, #3474, #6123, .T. ) ;
#9433 = CARTESIAN_POINT ( 'NONE',  ( 109.1586900883932856, -0.0006456433529162947105, -0.007109207791181750523 ) ) ;
#9434 = CARTESIAN_POINT ( 'NONE',  ( 109.1586900883932856, 0.006960773163852190457, -0.001582822706032850245 ) ) ;
#9435 = CARTESIAN_POINT ( 'NONE',  ( -55.24390624410018802, -0.01027195578987978239, -0.001811362924362686826 ) ) ;
#9436 = EDGE_CURVE ( 'NONE', #18370, #16400, #10901, .T. ) ;
#9437 = CARTESIAN_POINT ( 'NONE',  ( -23.79223135445720061, 3.207301057648340503, -33.03345552685145492 ) ) ;
#9438 = CARTESIAN_POINT ( 'NONE',  ( 16.05277956358231961, 75.66118899150499999, 121.7045645913016898 ) ) ;
#9439 = CARTESIAN_POINT ( 'NONE',  ( -20.57838717382308147, 18.89542499756500149, -23.26537097894111383 ) ) ;
#9440 = CARTESIAN_POINT ( 'NONE',  ( 25.86096068574581253, -0.9975172952966359086, 113.0494979885903888 ) ) ;
#9441 = CARTESIAN_POINT ( 'NONE',  ( 28.37644542392838432, -86.16884085958004391, 89.64009552702880512 ) ) ;
#9442 = ORIENTED_EDGE ( 'NONE', *, *, #28204, .F. ) ;
#9443 = CARTESIAN_POINT ( 'NONE',  ( -12.82751273423880178, -23.15139349681279057, 43.04932478553559605 ) ) ;
#9445 = CARTESIAN_POINT ( 'NONE',  ( -5.986830583229317604, -43.56094206392958768, -26.01297580803309728 ) ) ;
#9444 = CARTESIAN_POINT ( 'NONE',  ( 25.64681081121879203, 91.59071981940572016, 66.03065707438965148 ) ) ;
#9446 = CARTESIAN_POINT ( 'NONE',  ( 25.73574536432417403, -84.49061642666517002, 74.99093179013938482 ) ) ;
#9447 = CARTESIAN_POINT ( 'NONE',  ( 25.64681081121879203, -84.18689316039996129, -75.24277141833577787 ) ) ;
#9448 = ORIENTED_EDGE ( 'NONE', *, *, #12887, .T. ) ;
#9449 = DIRECTION ( 'NONE',  ( -0.5914120900931443270, -0.07630783613001361487, 0.8027508043202532528 ) ) ;
#9450 = CARTESIAN_POINT ( 'NONE',  ( -25.21435515916043713, 16.39063784838786475, 30.48034229288620622 ) ) ;
#9451 = CARTESIAN_POINT ( 'NONE',  ( 16.05277956358206737, -103.3141821208289031, 99.31161228512438299 ) ) ;
#9452 = ORIENTED_EDGE ( 'NONE', *, *, #11086, .T. ) ;
#9453 = CARTESIAN_POINT ( 'NONE',  ( 25.64681081121879203, 75.86069728269103507, -83.63051021305824406 ) ) ;
#9454 = ORIENTED_EDGE ( 'NONE', *, *, #13757, .F. ) ;
#9455 = B_SPLINE_CURVE_WITH_KNOTS ( 'NONE', 3,
 ( #10896, #19657, #4403, #8730, #21966, #2229, #11034 ),
 .UNSPECIFIED., .F., .F.,
 ( 4, 3, 4 ),
 ( 0.000000000000000000, 0.02398743853561323414, 0.04000277880656222251 ),
 .UNSPECIFIED. ) ;
#9456 = CARTESIAN_POINT ( 'NONE',  ( -20.57838717382308147, -29.92853265176832878, -1.611677988432255848 ) ) ;
#9457 =( BOUNDED_SURFACE ( )  B_SPLINE_SURFACE ( 3, 1, ( 
 ( #17770, #26546 ),
 ( #15904, #22250 ),
 ( #22392, #2659 ),
 ( #501, #354 ) ),
 .UNSPECIFIED., .F., .F., .F. ) 
 B_SPLINE_SURFACE_WITH_KNOTS ( ( 4, 4 ),
 ( 2, 2 ),
 ( 0.000000000000000000, 1.000000000000000000 ),
 ( 0.000000000000000000, 1.000000000000000000 ),
 .UNSPECIFIED. ) 
 GEOMETRIC_REPRESENTATION_ITEM ( )  RATIONAL_B_SPLINE_SURFACE ( (
 ( 1.000000000000000000, 1.000000000000000000),
 ( 0.9960225298536222738, 0.9999952330161893110),
 ( 0.9960225298536222738, 0.9999952330161893110),
 ( 1.000000000000000000, 1.000000000000000000) ) ) 
 REPRESENTATION_ITEM ( '' )  SURFACE ( )  );
#9458 = CARTESIAN_POINT ( 'NONE',  ( 28.37644542392841274, 8.957364412600206549, 124.0168596762486715 ) ) ;
#9459 = CARTESIAN_POINT ( 'NONE',  ( -20.20700224038492721, 16.58740185276746359, 24.51628800869029234 ) ) ;
#9460 = ORIENTED_EDGE ( 'NONE', *, *, #7535, .F. ) ;
#9461 = CARTESIAN_POINT ( 'NONE',  ( 109.1586900883932856, 0.0008465529156635116835, 0.007088091345229658585 ) ) ;
#9462 = ORIENTED_EDGE ( 'NONE', *, *, #2731, .T. ) ;
#9463 = CARTESIAN_POINT ( 'NONE',  ( -55.24271866751342941, -0.001545935011630304593, 0.009369360294295640129 ) ) ;
#9464 = EDGE_CURVE ( 'NONE', #18908, #19494, #18218, .T. ) ;
#9465 = VERTEX_POINT ( 'NONE', #20669 ) ;
#9466 = CARTESIAN_POINT ( 'NONE',  ( 0.000000000000000000, 0.000000000000000000, 0.000000000000000000 ) ) ;
#9467 = CARTESIAN_POINT ( 'NONE',  ( -22.23342874802668589, -20.31166691703108285, 24.24669006619395617 ) ) ;
#9468 = EDGE_CURVE ( 'NONE', #4669, #6221, #16405, .T. ) ;
#9469 = CARTESIAN_POINT ( 'NONE',  ( 10.93730112726002979, 104.7670965581027644, -108.9902118373731241 ) ) ;
#9470 = CARTESIAN_POINT ( 'NONE',  ( -1.539763995773694827, 16.63252574783043869, -43.19716353142335663 ) ) ;
#9471 = CARTESIAN_POINT ( 'NONE',  ( 1.833485406944043827, -125.4007332306540405, -73.01664920993097496 ) ) ;
#9472 = ADVANCED_FACE ( 'NONE', ( #9748 ), #25231, .F. ) ;
#9473 = ORIENTED_EDGE ( 'NONE', *, *, #24725, .F. ) ;
#9474 = CARTESIAN_POINT ( 'NONE',  ( -22.23226125620928784, -7.677408153693816573, 30.68305173820434462 ) ) ;
#9475 = CARTESIAN_POINT ( 'NONE',  ( 10.93730112725992676, -65.95960219663038515, -136.0306644680990473 ) ) ;
#9476 = CARTESIAN_POINT ( 'NONE',  ( -25.21435515916043002, 30.48034229288640162, -16.39063784838753790 ) ) ;
#9477 = ORIENTED_EDGE ( 'NONE', *, *, #19330, .T. ) ;
#9478 = ORIENTED_EDGE ( 'NONE', *, *, #9861, .T. ) ;
#9479 = CARTESIAN_POINT ( 'NONE',  ( -8.786685647604855376, -7.199674155859337787, -53.04920435127184675 ) ) ;
#9480 = FACE_OUTER_BOUND ( 'NONE', #24450, .T. ) ;
#9482 = CARTESIAN_POINT ( 'NONE',  ( 25.64670758986459376, -23.96231489924965885, 110.3390515846397477 ) ) ;
#9481 = CARTESIAN_POINT ( 'NONE',  ( 2.433796855181233454, 98.43889364293860922, 107.1581411821788947 ) ) ;
#9483 = B_SPLINE_CURVE_WITH_KNOTS ( 'NONE', 3,
 ( #23767, #3885, #19276, #19143, #10382, #12787 ),
 .UNSPECIFIED., .F., .F.,
 ( 4, 2, 4 ),
 ( 6.942281208919283290E-18, 0.0006311571484585998260, 0.001262314296917192713 ),
 .UNSPECIFIED. ) ;
#9484 = CARTESIAN_POINT ( 'NONE',  ( -2.904412668506668460, 47.56768199507434502, 2.864640348250799828 ) ) ;
#9485 = CARTESIAN_POINT ( 'NONE',  ( 25.64703792032471341, -83.80974623566345372, 75.66285916808271850 ) ) ;
#9486 = CARTESIAN_POINT ( 'NONE',  ( 2.433796855181205476, -86.69855925934052721, 116.8607839509053434 ) ) ;
#9487 = EDGE_LOOP ( 'NONE', ( #1671, #28050, #20665, #1871 ) ) ;
#9488 = CARTESIAN_POINT ( 'NONE',  ( 13.84597867724968623, -137.9700459519984861, -49.85807424839893542 ) ) ;
#9489 = CARTESIAN_POINT ( 'NONE',  ( -24.53237795827032741, 29.54731592868594348, 16.68575684089460864 ) ) ;
#9490 = CARTESIAN_POINT ( 'NONE',  ( 25.64704443564079384, 11.66968230815913898, 112.3065506427462310 ) ) ;
#9491 = CARTESIAN_POINT ( 'NONE',  ( -55.24198130335446422, 0.008310594958151115014, 0.004163123460805739397 ) ) ;
#9492 = CARTESIAN_POINT ( 'NONE',  ( 1.832998868059890096, -72.09222286251173273, 125.9352106559981621 ) ) ;
#9493 = CARTESIAN_POINT ( 'NONE',  ( 1.833485406944043827, 125.9346397303445286, -72.09189602597577107 ) ) ;
#9494 = ORIENTED_EDGE ( 'NONE', *, *, #23752, .T. ) ;
#9495 = CARTESIAN_POINT ( 'NONE',  ( 25.81918753295380498, -12.74259626488075980, -112.3053965977762800 ) ) ;
#9496 = ORIENTED_EDGE ( 'NONE', *, *, #27041, .F. ) ;
#9497 = CARTESIAN_POINT ( 'NONE',  ( 25.64681081121879203, 110.3564950173084895, -23.88203588907973085 ) ) ;
#9498 = CARTESIAN_POINT ( 'NONE',  ( 1.832998868059858122, 44.33343224355416368, -138.1720401012262585 ) ) ;
#9499 = ORIENTED_EDGE ( 'NONE', *, *, #909, .T. ) ;
#9500 = ORIENTED_EDGE ( 'NONE', *, *, #12996, .T. ) ;
#9501 = EDGE_CURVE ( 'NONE', #2306, #13087, #27724, .T. ) ;
#9502 = ORIENTED_EDGE ( 'NONE', *, *, #755, .F. ) ;
#9503 = ADVANCED_FACE ( 'NONE', ( #22570 ), #3525, .F. ) ;
#9504 =( BOUNDED_SURFACE ( )  B_SPLINE_SURFACE ( 3, 1, ( 
 ( #20318, #13555 ),
 ( #6960, #20606 ),
 ( #24807, #7532 ),
 ( #20464, #16292 ) ),
 .UNSPECIFIED., .F., .F., .F. ) 
 B_SPLINE_SURFACE_WITH_KNOTS ( ( 4, 4 ),
 ( 2, 2 ),
 ( 0.000000000000000000, 1.000000000000000000 ),
 ( 0.000000000000000000, 1.000000000000000000 ),
 .UNSPECIFIED. ) 
 GEOMETRIC_REPRESENTATION_ITEM ( )  RATIONAL_B_SPLINE_SURFACE ( (
 ( 1.000000000000000000, 1.000000000000000000),
 ( 0.9956975270656955868, 0.8568959468854907557),
 ( 0.9956975270656955868, 0.8568959468854907557),
 ( 1.000000000000000000, 1.000000000000000000) ) ) 
 REPRESENTATION_ITEM ( '' )  SURFACE ( )  );
#9505 = DIRECTION ( 'NONE',  ( -1.000000000000000000, -0.000000000000000000, -0.000000000000000000 ) ) ;
#9506 = CARTESIAN_POINT ( 'NONE',  ( 1.831572820252008738, 96.36280042115929234, 108.4969585352558141 ) ) ;
#9507 = DIRECTION ( 'NONE',  ( 0.000000000000000000, 0.000000000000000000, 1.000000000000000000 ) ) ;
#9508 = CARTESIAN_POINT ( 'NONE',  ( 55.49584447822657296, 54.09506550945626202, 48.34726110740004401 ) ) ;
#9509 = ORIENTED_EDGE ( 'NONE', *, *, #22969, .T. ) ;
#9510 = CARTESIAN_POINT ( 'NONE',  ( -12.94347594948480662, 35.22469990145658159, 33.69581619287838947 ) ) ;
#9511 = B_SPLINE_CURVE_WITH_KNOTS ( 'NONE', 3,
 ( #2857, #26883, #13502, #24616, #26594, #20690, #7191 ),
 .UNSPECIFIED., .F., .F.,
 ( 4, 3, 4 ),
 ( 0.000000000000000000, 0.006568092053401831769, 0.02506242213020820619 ),
 .UNSPECIFIED. ) ;
#9512 = CARTESIAN_POINT ( 'NONE',  ( 109.1587776205901577, -0.001605238040359084932, 0.007151389024634731938 ) ) ;
#9513 = CARTESIAN_POINT ( 'NONE',  ( -1.044557008772710072, -45.76404748504492659, -1.643388457097728184 ) ) ;
#9514 = ORIENTED_EDGE ( 'NONE', *, *, #13936, .F. ) ;
#9515 = ORIENTED_EDGE ( 'NONE', *, *, #16387, .F. ) ;
#9516 = CARTESIAN_POINT ( 'NONE',  ( -20.57838717382308147, 28.96176188950229502, 7.715628353033378239 ) ) ;
#9517 = FACE_OUTER_BOUND ( 'NONE', #22822, .T. ) ;
#9518 = CARTESIAN_POINT ( 'NONE',  ( 2.263178113027033866, 96.24282436106614114, 108.9830942735796953 ) ) ;
#9519 = CARTESIAN_POINT ( 'NONE',  ( 1.832998868059858122, 137.8420662456170191, 45.34898734666095521 ) ) ;
#9520 = B_SPLINE_CURVE_WITH_KNOTS ( 'NONE', 3,
 ( #8728, #26143, #4125, #8458 ),
 .UNSPECIFIED., .F., .F.,
 ( 4, 4 ),
 ( 0.000000000000000000, 0.01077107196513892549 ),
 .UNSPECIFIED. ) ;
#9521 = VERTEX_POINT ( 'NONE', #6007 ) ;
#9522 = CARTESIAN_POINT ( 'NONE',  ( -55.24271866751342941, -0.009369360294295348696, -0.001545935011630817420 ) ) ;
#9523 = CARTESIAN_POINT ( 'NONE',  ( 10.93730112725994275, -36.23586118136433498, -146.7718404940647190 ) ) ;
#9524 = CARTESIAN_POINT ( 'NONE',  ( -2.904412668506659578, -36.79926976721470311, -30.27712468694973325 ) ) ;
#9525 = CARTESIAN_POINT ( 'NONE',  ( 25.65782528836482257, -75.98558751977830639, 83.52701600504848045 ) ) ;
#9526 = CARTESIAN_POINT ( 'NONE',  ( -20.57838717382308147, 1.611677988432778319, 29.92853265176829325 ) ) ;
#9527 = ORIENTED_EDGE ( 'NONE', *, *, #26992, .F. ) ;
#9528 = CARTESIAN_POINT ( 'NONE',  ( 1.833603222531972055, 145.1089511853978422, 0.4449221977524496774 ) ) ;
#9529 = ORIENTED_EDGE ( 'NONE', *, *, #21053, .F. ) ;
#9530 = B_SPLINE_CURVE_WITH_KNOTS ( 'NONE', 3,
 ( #5703, #16484, #20802, #13890, #18645, #25132, #18784, #7430 ),
 .UNSPECIFIED., .F., .F.,
 ( 4, 2, 2, 4 ),
 ( 0.000000000000000000, 0.0002429588503611257672, 0.0004859177007222515343, 0.0009718354014445030687 ),
 .UNSPECIFIED. ) ;
#9531 = EDGE_LOOP ( 'NONE', ( #28270, #1455, #8131, #15249 ) ) ;
#9532 = EDGE_CURVE ( 'NONE', #16816, #27092, #21194, .T. ) ;
#9533 = VERTEX_POINT ( 'NONE', #25290 ) ;
#9534 = DIRECTION ( 'NONE',  ( 0.5914120900931444380, -0.09226095020378993761, 0.8010740644654227305 ) ) ;
#9535 = EDGE_CURVE ( 'NONE', #27686, #14763, #12050, .T. ) ;
#9536 = CARTESIAN_POINT ( 'NONE',  ( -1.049819825607592794, 43.71263398674771139, 13.66706894614392986 ) ) ;
#9537 = CARTESIAN_POINT ( 'NONE',  ( -1.031422197589716205, -43.06660437151320053, -15.60268798220621633 ) ) ;
#9538 = B_SPLINE_CURVE_WITH_KNOTS ( 'NONE', 3,
 ( #16866, #1028, #25650, #23354 ),
 .UNSPECIFIED., .F., .F.,
 ( 4, 4 ),
 ( 2.031330821370476332E-16, 0.008383748772659684392 ),
 .UNSPECIFIED. ) ;
#9539 = CARTESIAN_POINT ( 'NONE',  ( -25.21435515916043357, -34.29329011225959079, -4.655591116594231416 ) ) ;
#9540 = CARTESIAN_POINT ( 'NONE',  ( 1.832998868059858122, 142.0492247521726199, -29.64765804469933386 ) ) ;
#9541 = CARTESIAN_POINT ( 'NONE',  ( -20.57838717382308147, -27.96569011373093971, -10.78122205916989529 ) ) ;
#9542 = CARTESIAN_POINT ( 'NONE',  ( 25.70243777736190438, 107.6443926015135304, -34.20488708977986647 ) ) ;
#9543 = CARTESIAN_POINT ( 'NONE',  ( 109.1586900883932856, -0.005833932871491344374, -0.004113747440992306104 ) ) ;
#9544 = CARTESIAN_POINT ( 'NONE',  ( 2.430230287190572103, 13.76600171652642857, 144.8619874886007324 ) ) ;
#9545 = CARTESIAN_POINT ( 'NONE',  ( -18.41936578851708717, 30.66520733838696344, 29.33493038358041360 ) ) ;
#9546 = CARTESIAN_POINT ( 'NONE',  ( -1.539760825549689516, -25.17088484262114179, 38.84664866728805066 ) ) ;
#9547 = CARTESIAN_POINT ( 'NONE',  ( 25.64708228042118421, -66.33571787052753166, -91.37028996123333968 ) ) ;
#9548 = CARTESIAN_POINT ( 'NONE',  ( -55.25719721206881729, 0.004044147484878754875, 0.01041086141212503938 ) ) ;
#9549 = CARTESIAN_POINT ( 'NONE',  ( -1.050231094221207417, -36.90262059116448512, 27.12595454131546191 ) ) ;
#9550 = CARTESIAN_POINT ( 'NONE',  ( -1.056502255334265339, 0.5104472526220019679, -45.80535052436397336 ) ) ;
#9551 = CARTESIAN_POINT ( 'NONE',  ( 109.1778270068192853, 0.009177562596826678576, -0.001591747944959453478 ) ) ;
#9552 = ORIENTED_EDGE ( 'NONE', *, *, #2468, .F. ) ;
#9553 = CARTESIAN_POINT ( 'NONE',  ( 28.43349137099836810, 29.78331910005492489, 120.6297847406436858 ) ) ;
#9554 = EDGE_CURVE ( 'NONE', #27588, #13723, #14478, .T. ) ;
#9555 = ORIENTED_EDGE ( 'NONE', *, *, #10269, .F. ) ;
#9556 = CARTESIAN_POINT ( 'NONE',  ( 25.73574536432417759, 103.5288236655401732, -45.21157800100201030 ) ) ;
#9557 = CARTESIAN_POINT ( 'NONE',  ( 25.86096068574580187, -12.80894308910809976, 112.3259320600844404 ) ) ;
#9558 = ORIENTED_EDGE ( 'NONE', *, *, #2658, .T. ) ;
#9559 = EDGE_CURVE ( 'NONE', #2065, #23678, #22088, .T. ) ;
#9560 = ORIENTED_EDGE ( 'NONE', *, *, #12599, .F. ) ;
#9561 = ORIENTED_EDGE ( 'NONE', *, *, #19406, .T. ) ;
#9562 = EDGE_CURVE ( 'NONE', #17914, #1034, #1615, .T. ) ;
#9563 = CARTESIAN_POINT ( 'NONE',  ( 109.1624594426973260, 0.009754804742273283369, -0.01263706729758985563 ) ) ;
#9564 = ADVANCED_FACE ( 'NONE', ( #23284 ), #20075, .F. ) ;
#9565 = DIRECTION ( 'NONE',  ( 0.000000000000000000, 0.000000000000000000, 1.000000000000000000 ) ) ;
#9566 = CARTESIAN_POINT ( 'NONE',  ( 1.833809397773857208, 144.3333383260368805, -14.99109763363995818 ) ) ;
#9567 = CARTESIAN_POINT ( 'NONE',  ( -8.259864102781675044, 52.06232470801727885, 9.986657004933084281 ) ) ;
#9568 = CARTESIAN_POINT ( 'NONE',  ( -8.786685647604890903, 25.35688121747502066, -47.14957014837363403 ) ) ;
#9569 = FACE_OUTER_BOUND ( 'NONE', #26120, .T. ) ;
#9570 = CARTESIAN_POINT ( 'NONE',  ( 8.186469777910877710, -102.4860666868856924, -108.6390983781767972 ) ) ;
#9571 = B_SPLINE_CURVE_WITH_KNOTS ( 'NONE', 3,
 ( #8206, #16974, #1578, #25765, #6058, #8350, #23623, #21432, #6197, #25499 ),
 .UNSPECIFIED., .F., .F.,
 ( 4, 2, 2, 2, 4 ),
 ( 2.976713740813343128E-16, 0.0003346187017559147311, 0.0006692374035115318488, 0.001003856105267148966, 0.001338474807022765976 ),
 .UNSPECIFIED. ) ;
#9572 = CARTESIAN_POINT ( 'NONE',  ( -25.21435515916025594, 34.29329011225976842, -4.655591116594504086 ) ) ;
#9573 = CARTESIAN_POINT ( 'NONE',  ( 2.430230287190572103, -132.3371620660946917, -60.50928654924886985 ) ) ;
#9574 = CARTESIAN_POINT ( 'NONE',  ( 28.37603512858454735, -48.29936889363892760, -104.0705994281842095 ) ) ;
#9575 = ORIENTED_EDGE ( 'NONE', *, *, #21012, .F. ) ;
#9576 = ORIENTED_EDGE ( 'NONE', *, *, #6249, .F. ) ;
#9577 = CARTESIAN_POINT ( 'NONE',  ( -1.045287976400379737, 44.00138577190644185, -12.68782741917337198 ) ) ;
#9579 = CARTESIAN_POINT ( 'NONE',  ( -25.21435515916043357, 6.169479169075458458, -34.05351380035335751 ) ) ;
#9578 = CARTESIAN_POINT ( 'NONE',  ( 10.93730112726002623, 65.95960219663321311, -136.0306644680977683 ) ) ;
#9580 = CARTESIAN_POINT ( 'NONE',  ( 10.93730112725993919, -42.00474393596157086, -145.2260730187406352 ) ) ;
#9581 = CARTESIAN_POINT ( 'NONE',  ( 28.37644542392844826, 29.80435743554116712, -120.7150203538605240 ) ) ;
#9582 = CARTESIAN_POINT ( 'NONE',  ( 32.73300124599739291, -113.0038235389599635, -32.68291970228351317 ) ) ;
#9583 = CARTESIAN_POINT ( 'NONE',  ( -55.24390624410018802, 0.004896917417128144288, 0.009209468562451129242 ) ) ;
#9584 =( BOUNDED_SURFACE ( )  B_SPLINE_SURFACE ( 3, 1, ( 
 ( #15072, #2250 ),
 ( #23894, #22284 ),
 ( #13490, #11332 ),
 ( #28179, #12920 ) ),
 .UNSPECIFIED., .F., .F., .F. ) 
 B_SPLINE_SURFACE_WITH_KNOTS ( ( 4, 4 ),
 ( 2, 2 ),
 ( 0.000000000000000000, 1.000000000000000000 ),
 ( 0.000000000000000000, 1.000000000000000000 ),
 .UNSPECIFIED. ) 
 GEOMETRIC_REPRESENTATION_ITEM ( )  RATIONAL_B_SPLINE_SURFACE ( (
 ( 1.000000000000000000, 1.000000000000000000),
 ( 0.9934239774497837239, 0.8357310067453919133),
 ( 0.9934239774497837239, 0.8357310067453919133),
 ( 1.000000000000000000, 1.000000000000000000) ) ) 
 REPRESENTATION_ITEM ( '' )  SURFACE ( )  );
#9585 = VERTEX_POINT ( 'NONE', #1380 ) ;
#9586 = DIRECTION ( 'NONE',  ( -1.000000000000000000, -0.000000000000000000, -0.000000000000000000 ) ) ;
#9587 = CARTESIAN_POINT ( 'NONE',  ( 10.93730112725992853, -56.95489579269655422, -140.0398180619117738 ) ) ;
#9588 = CARTESIAN_POINT ( 'NONE',  ( 28.43349137099833968, -89.57679848841864612, 86.10800331998756008 ) ) ;
#9589 = ORIENTED_EDGE ( 'NONE', *, *, #16621, .T. ) ;
#9590 = CARTESIAN_POINT ( 'NONE',  ( -1.583189561560252701, -43.29471907393753582, -16.68617981233686365 ) ) ;
#9591 = ADVANCED_FACE ( 'NONE', ( #19095 ), #17018, .T. ) ;
#9592 = ORIENTED_EDGE ( 'NONE', *, *, #21808, .T. ) ;
#9593 = CARTESIAN_POINT ( 'NONE',  ( 30.58324630866339433, -119.8048187378265226, 16.55818995381107683 ) ) ;
#9594 = EDGE_CURVE ( 'NONE', #24974, #2917, #8295, .T. ) ;
#9595 = CARTESIAN_POINT ( 'NONE',  ( -55.25297051322618813, -0.01306918787467238607, -0.007247191603129069307 ) ) ;
#9596 = CARTESIAN_POINT ( 'NONE',  ( 2.263178607246675078, -132.2496131833833601, 60.41552769843774939 ) ) ;
#9597 = ORIENTED_EDGE ( 'NONE', *, *, #7796, .F. ) ;
#9598 = DIRECTION ( 'NONE',  ( -1.000000000000000000, -0.000000000000000000, -0.000000000000000000 ) ) ;
#9599 = ORIENTED_EDGE ( 'NONE', *, *, #27252, .F. ) ;
#9600 = CARTESIAN_POINT ( 'NONE',  ( -25.21435515916044423, -16.39063784838720395, 30.48034229288656505 ) ) ;
#9601 = VERTEX_POINT ( 'NONE', #21388 ) ;
#9602 = CARTESIAN_POINT ( 'NONE',  ( -20.37983603106074071, 28.74620395171562492, -7.753708011498657626 ) ) ;
#9603 = CARTESIAN_POINT ( 'NONE',  ( -1.464342487929844783, -38.76467504336602588, -25.15873223207679743 ) ) ;
#9604 = CARTESIAN_POINT ( 'NONE',  ( 25.64704443564078318, 107.4261196778967502, -34.76451658509423481 ) ) ;
#9605 = CARTESIAN_POINT ( 'NONE',  ( 24.01988960052056754, 130.9749633972838296, 4.273195451969105108 ) ) ;
#9606 = DIRECTION ( 'NONE',  ( -1.000000000000000000, 6.938893903907226837E-18, -1.734723475976806709E-18 ) ) ;
#9607 = ORIENTED_EDGE ( 'NONE', *, *, #8489, .F. ) ;
#9608 = B_SPLINE_CURVE_WITH_KNOTS ( 'NONE', 3,
 ( #14595, #8139, #2478, #467 ),
 .UNSPECIFIED., .F., .F.,
 ( 4, 4 ),
 ( 1.977889076651310254E-16, 0.001982023823822937677 ),
 .UNSPECIFIED. ) ;
#9609 = DIRECTION ( 'NONE',  ( -1.000000000000000000, -0.000000000000000000, -0.000000000000000000 ) ) ;
#9610 = CARTESIAN_POINT ( 'NONE',  ( -1.239374126674604337, -44.48112152129338170, 11.92219841463876229 ) ) ;
#9611 = CARTESIAN_POINT ( 'NONE',  ( 25.69398547355838502, 98.18017599249837701, 55.82723250638802881 ) ) ;
#9612 = EDGE_LOOP ( 'NONE', ( #23976, #26859, #5236, #2889 ) ) ;
#9613 = ORIENTED_EDGE ( 'NONE', *, *, #17412, .T. ) ;
#9614 = ORIENTED_EDGE ( 'NONE', *, *, #23662, .F. ) ;
#9615 = CARTESIAN_POINT ( 'NONE',  ( -1.048994561756802169, 36.59609844253166244, 27.53485040342854262 ) ) ;
#9616 = CARTESIAN_POINT ( 'NONE',  ( -55.24271866751342941, 0.006757859501010507128, -0.006671293903668127322 ) ) ;
#9618 = FACE_OUTER_BOUND ( 'NONE', #1133, .T. ) ;
#9617 = CARTESIAN_POINT ( 'NONE',  ( -8.786685647604892679, -53.04920435127177569, 7.199674155859498548 ) ) ;
#9619 = CARTESIAN_POINT ( 'NONE',  ( -1.619063947482197729, -35.99532424477357750, 29.22875152547795707 ) ) ;
#9620 = CARTESIAN_POINT ( 'NONE',  ( -55.24300891470650754, 0.007734635432136952211, -0.006048736206179535120 ) ) ;
#9621 = CARTESIAN_POINT ( 'NONE',  ( 25.64704443564076897, -83.99864088993820133, 75.45310550990124909 ) ) ;
#9622 = CARTESIAN_POINT ( 'NONE',  ( -6.588769196390765970, -50.13301368233292976, 11.07780292579747083 ) ) ;
#9623 = ORIENTED_EDGE ( 'NONE', *, *, #12539, .F. ) ;
#9624 = CARTESIAN_POINT ( 'NONE',  ( 10.93730112726002623, 65.95960219663321311, -136.0306644680977683 ) ) ;
#9625 = CARTESIAN_POINT ( 'NONE',  ( -20.24419206586950892, -23.20105925399712987, 18.44224248888897577 ) ) ;
#9626 =( BOUNDED_SURFACE ( )  B_SPLINE_SURFACE ( 3, 1, ( 
 ( #20015, #13384 ),
 ( #6936, #15257 ),
 ( #23933, #4336 ),
 ( #4193, #26208 ) ),
 .UNSPECIFIED., .F., .F., .F. ) 
 B_SPLINE_SURFACE_WITH_KNOTS ( ( 4, 4 ),
 ( 2, 2 ),
 ( 0.000000000000000000, 1.000000000000000000 ),
 ( 0.000000000000000000, 1.000000000000000000 ),
 .UNSPECIFIED. ) 
 GEOMETRIC_REPRESENTATION_ITEM ( )  RATIONAL_B_SPLINE_SURFACE ( (
 ( 1.000000000000000000, 1.000000000000000000),
 ( 0.9956975270656954757, 0.8568959468854893125),
 ( 0.9956975270656954757, 0.8568959468854893125),
 ( 1.000000000000000000, 1.000000000000000000) ) ) 
 REPRESENTATION_ITEM ( '' )  SURFACE ( )  );
#9627 = CARTESIAN_POINT ( 'NONE',  ( 26.11404676487257603, 36.06104232266594067, -107.3263591096426666 ) ) ;
#9628 = CARTESIAN_POINT ( 'NONE',  ( -1.056502255334265339, -36.75727364034752043, -27.33667001641156702 ) ) ;
#9629 = CARTESIAN_POINT ( 'NONE',  ( 32.73300124599741423, 114.2056417606551406, -28.19767303745493336 ) ) ;
#9630 = CARTESIAN_POINT ( 'NONE',  ( -55.24390624410018802, 0.007503127514278223366, 0.007245494385991344682 ) ) ;
#9631 = EDGE_CURVE ( 'NONE', #16962, #6242, #4724, .T. ) ;
#9632 = ORIENTED_EDGE ( 'NONE', *, *, #26538, .T. ) ;
#9633 = CARTESIAN_POINT ( 'NONE',  ( 25.98552792386800192, -12.89843290883451665, -112.3992180166320765 ) ) ;
#9634 = CARTESIAN_POINT ( 'NONE',  ( -8.786685647604890903, 52.67761315067286176, -9.545808661480789326 ) ) ;
#9635 = EDGE_CURVE ( 'NONE', #26995, #10146, #7500, .T. ) ;
#9636 = CARTESIAN_POINT ( 'NONE',  ( -7.078251931573406708, 50.86685171665428840, 11.16394717458623731 ) ) ;
#9637 = ORIENTED_EDGE ( 'NONE', *, *, #14189, .T. ) ;
#9638 = ADVANCED_FACE ( 'NONE', ( #12321 ), #18056, .F. ) ;
#9639 = ORIENTED_EDGE ( 'NONE', *, *, #15225, .F. ) ;
#9640 = AXIS2_PLACEMENT_3D ( 'NONE', #19422, #19693, #25773 ) ;
#9641 = ORIENTED_EDGE ( 'NONE', *, *, #4816, .T. ) ;
#9642 = CARTESIAN_POINT ( 'NONE',  ( -28.13707043255157103, -18.06394523322463641, -14.07296284901326189 ) ) ;
#9643 = CARTESIAN_POINT ( 'NONE',  ( 109.1721716018069515, 0.007126480965767985690, -0.01550977894511847664 ) ) ;
#9644 = CARTESIAN_POINT ( 'NONE',  ( -20.24419206586951603, 24.70913649113854049, 16.36655224501340555 ) ) ;
#9645 = CARTESIAN_POINT ( 'NONE',  ( -2.265401668238152588, 45.46007138824041505, -11.98901689611057009 ) ) ;
#9646 = CARTESIAN_POINT ( 'NONE',  ( 25.64670758986457244, 66.76959937251574217, -91.05338785329374218 ) ) ;
#9647 = CARTESIAN_POINT ( 'NONE',  ( 25.64692232868534560, -103.0161468101950533, 46.22343382108700638 ) ) ;
#9648 = ADVANCED_FACE ( 'NONE', ( #19506 ), #23063, .F. ) ;
#9649 = CARTESIAN_POINT ( 'NONE',  ( 26.11404676487259024, 22.43340081644921113, -110.9778746459744667 ) ) ;
#9650 = ORIENTED_EDGE ( 'NONE', *, *, #6227, .T. ) ;
#9651 = ORIENTED_EDGE ( 'NONE', *, *, #16071, .F. ) ;
#9652 = CARTESIAN_POINT ( 'NONE',  ( -55.24390624410018802, 0.01027195578988056128, 0.001811362924362418811 ) ) ;
#9653 = PRODUCT_DEFINITION ( 'UNKNOWN', '', #28195, #28079 ) ;
#9654 = CARTESIAN_POINT ( 'NONE',  ( -1.050230346682677007, -37.05264119692671443, 26.91946103437146931 ) ) ;
#9655 = CARTESIAN_POINT ( 'NONE',  ( -55.24271866751342941, -0.009369360294294061531, 0.001545935011626861600 ) ) ;
#9656 = LINE ( 'NONE', #20154, #24863 ) ;
#9657 = CARTESIAN_POINT ( 'NONE',  ( 1.893872463202060707, -84.54426271294347828, -117.9862474593105617 ) ) ;
#9658 = ADVANCED_FACE ( 'NONE', ( #10877 ), #19325, .F. ) ;
#9659 = LINE ( 'NONE', #14241, #11651 ) ;
#9660 = B_SPLINE_CURVE_WITH_KNOTS ( 'NONE', 3,
 ( #26770, #15845, #24652, #11522, #20298, #18719, #23060 ),
 .UNSPECIFIED., .F., .F.,
 ( 4, 3, 4 ),
 ( 0.000000000000000000, 0.009512539173626427882, 0.02506242213020844906 ),
 .UNSPECIFIED. ) ;
#9661 = VERTEX_POINT ( 'NONE', #13301 ) ;
#9662 = CARTESIAN_POINT ( 'NONE',  ( 25.64681081121879203, 84.18689316040146764, -75.24277141833410099 ) ) ;
#9663 = CARTESIAN_POINT ( 'NONE',  ( -1.046936909428679563, -1.275306677858562221, -45.77873603877005593 ) ) ;
#9664 = ADVANCED_FACE ( 'NONE', ( #15167 ), #19013, .F. ) ;
#9665 = CARTESIAN_POINT ( 'NONE',  ( 109.1589550718174877, -0.0002241941239240967485, 0.007571935245604908063 ) ) ;
#9666 = CARTESIAN_POINT ( 'NONE',  ( -6.588769196390754423, -44.25609997968886233, 26.02756986588589072 ) ) ;
#9667 = EDGE_CURVE ( 'NONE', #21777, #28456, #24313, .T. ) ;
#9668 = CARTESIAN_POINT ( 'NONE',  ( 1.833485406944043827, -137.8414413349082110, -45.34878176254374438 ) ) ;
#9669 = ORIENTED_EDGE ( 'NONE', *, *, #22365, .F. ) ;
#9670 = CARTESIAN_POINT ( 'NONE',  ( 28.43349137099837165, -102.8504004831930843, -69.71646995966284521 ) ) ;
#9671 = ORIENTED_EDGE ( 'NONE', *, *, #25112, .F. ) ;
#9672 =( BOUNDED_SURFACE ( )  B_SPLINE_SURFACE ( 3, 1, ( 
 ( #18969, #27748 ),
 ( #8179, #16520 ),
 ( #5878, #25600 ),
 ( #5585, #25733 ) ),
 .UNSPECIFIED., .F., .F., .F. ) 
 B_SPLINE_SURFACE_WITH_KNOTS ( ( 4, 4 ),
 ( 2, 2 ),
 ( 0.000000000000000000, 1.000000000000000000 ),
 ( 0.000000000000000000, 1.000000000000000000 ),
 .UNSPECIFIED. ) 
 GEOMETRIC_REPRESENTATION_ITEM ( )  RATIONAL_B_SPLINE_SURFACE ( (
 ( 1.000000000000000000, 1.000000000000000000),
 ( 0.9934239774497838349, 0.8357310067453913582),
 ( 0.9934239774497838349, 0.8357310067453913582),
 ( 1.000000000000000000, 1.000000000000000000) ) ) 
 REPRESENTATION_ITEM ( '' )  SURFACE ( )  );
#9673 = VERTEX_POINT ( 'NONE', #6282 ) ;
#9674 = ORIENTED_EDGE ( 'NONE', *, *, #12882, .T. ) ;
#9675 = AXIS2_PLACEMENT_3D ( 'NONE', #23889, #26162, #15205 ) ;
#9676 = AXIS2_PLACEMENT_3D ( 'NONE', #18193, #4683, #22691 ) ;
#9677 = CARTESIAN_POINT ( 'NONE',  ( 24.01988960052068833, 117.9135177031536159, 57.17607523395246716 ) ) ;
#9678 = CARTESIAN_POINT ( 'NONE',  ( 109.1624594426973260, 0.003771499231549574858, -0.01551217196236920511 ) ) ;
#9679 = CARTESIAN_POINT ( 'NONE',  ( 2.433796855181205476, -98.43889364293931976, 107.1581411821782268 ) ) ;
#9680 = LINE ( 'NONE', #25092, #21667 ) ;
#9681 = CARTESIAN_POINT ( 'NONE',  ( -28.41354790283022069, 1.249099604787400564, 23.16239616762929288 ) ) ;
#9682 = CARTESIAN_POINT ( 'NONE',  ( 2.063896406836609909, 137.7380992975108995, -46.16709813092479919 ) ) ;
#9683 = DIRECTION ( 'NONE',  ( 0.000000000000000000, 0.000000000000000000, 1.000000000000000000 ) ) ;
#9684 = EDGE_CURVE ( 'NONE', #26638, #18375, #28035, .T. ) ;
#9685 = CARTESIAN_POINT ( 'NONE',  ( 32.73300124599740002, 110.6325518752278896, -39.98094346392192477 ) ) ;
#9686 = DIRECTION ( 'NONE',  ( -1.000000000000000000, -0.000000000000000000, -0.000000000000000000 ) ) ;
#9687 = CARTESIAN_POINT ( 'NONE',  ( 25.73574536432413851, -55.78561308781419115, -98.23578516675019046 ) ) ;
#9688 = EDGE_CURVE ( 'NONE', #10668, #26700, #9857, .T. ) ;
#9689 = CARTESIAN_POINT ( 'NONE',  ( 25.64681081121879203, -66.03065707438874199, -91.59071981940638807 ) ) ;
#9690 = AXIS2_PLACEMENT_3D ( 'NONE', #10786, #4008, #11055 ) ;
#9691 = EDGE_CURVE ( 'NONE', #14673, #4178, #14985, .T. ) ;
#9692 = CARTESIAN_POINT ( 'NONE',  ( 25.69398547355841345, 76.12333255527515519, 83.43419615433019487 ) ) ;
#9693 = CARTESIAN_POINT ( 'NONE',  ( 2.433796855181205476, -71.49415740224986848, -126.7346379669263001 ) ) ;
#9694 = CARTESIAN_POINT ( 'NONE',  ( 109.1624594426973260, 0.01438905500501226620, 0.006914244825461683328 ) ) ;
#9695 = ORIENTED_EDGE ( 'NONE', *, *, #6002, .T. ) ;
#9696 = CARTESIAN_POINT ( 'NONE',  ( 9.884929003653626367, 150.4771565009630478, -4.203795436552884013 ) ) ;
#9697 = VECTOR ( 'NONE', #3228, 1000.000000000000114 ) ;
#9698 = EDGE_LOOP ( 'NONE', ( #8002, #17022, #26286, #7774, #5857, #6700, #8035, #26974, #5036, #5052, #18357, #26361, #12964, #8821, #372, #19364, #305, #28405, #20382, #20376, #13465, #6467, #11389, #18496, #3194, #13978, #1551, #20954, #12371, #18641, #2259, #3725, #485, #1483, #18930, #4065, #10534, #851, #15890, #20309, #16061, #6150, #14097, #5275, #10206, #12360, #18676, #10909, #25464, #15431, #23464, #15675, #27542, #21300, #26574, #2727, #22431, #9641, #10176, #9589, #10578, #4610, #2987, #11455, #22469, #5870, #2992, #27195, #1460, #4386, #25738, #5840, #4102, #23057, #5326, #17266, #21209, #17821, #11119, #11156, #27847, #15103, #16143, #22877, #7303, #24546, #15126, #17723, #5261, #5043, #25286, #27422, #17743, #24481, #9367, #22129, #14008, #20746, #25970, #18627, #17298, #6260, #21503, #25577, #22511, #10396, #11604, #24303, #19965, #25843, #28069, #26963, #6699, #14825, #5015, #19688, #16549, #20333, #2348, #12655, #21448, #22292, #24829, #2278, #25334, #20352, #11286, #7407, #11083, #26612, #922, #24323, #21047, #12111, #23558, #22444, #8854, #20052, #20851, #20769, #23675, #16020, #15839, #7102, #3416, #2034, #17279, #5033, #23350, #11970, #13867, #14848, #263, #9494, #1631, #2476, #5203, #14651, #7818, #13157, #4575, #28239, #21459, #14440, #20591, #18761, #25166, #2172, #5231, #23168, #5994, #22194, #9637, #15783, #21279, #24800, #28423, #5492, #15635, #3317, #10333, #15600, #10673, #21683 ) ) ;
#9699 = CARTESIAN_POINT ( 'NONE',  ( 1.832998868059890096, 14.63705790014200936, -144.3700883710215521 ) ) ;
#9700 = CARTESIAN_POINT ( 'NONE',  ( 109.1721716018069657, -0.01629455849720094079, -0.005082060336469356072 ) ) ;
#9701 = ORIENTED_EDGE ( 'NONE', *, *, #17304, .F. ) ;
#9702 = B_SPLINE_CURVE_WITH_KNOTS ( 'NONE', 3,
 ( #11784, #11480, #24317, #13639, #20407, #20117 ),
 .UNSPECIFIED., .F., .F.,
 ( 4, 2, 4 ),
 ( 1.734723475976807094E-18, 0.0004335151646191503279, 0.0008670303292382989212 ),
 .UNSPECIFIED. ) ;
#9703 = VERTEX_POINT ( 'NONE', #21492 ) ;
#9704 =( BOUNDED_SURFACE ( )  B_SPLINE_SURFACE ( 3, 1, ( 
 ( #16386, #10069 ),
 ( #5304, #27601 ),
 ( #27464, #16685 ),
 ( #19121, #18982 ) ),
 .UNSPECIFIED., .F., .F., .F. ) 
 B_SPLINE_SURFACE_WITH_KNOTS ( ( 4, 4 ),
 ( 2, 2 ),
 ( 0.000000000000000000, 1.000000000000000000 ),
 ( 0.000000000000000000, 1.000000000000000000 ),
 .UNSPECIFIED. ) 
 GEOMETRIC_REPRESENTATION_ITEM ( )  RATIONAL_B_SPLINE_SURFACE ( (
 ( 1.000000000000000000, 1.000000000000000000),
 ( 0.9956975270656954757, 0.8568959468854893125),
 ( 0.9956975270656954757, 0.8568959468854893125),
 ( 1.000000000000000000, 1.000000000000000000) ) ) 
 REPRESENTATION_ITEM ( '' )  SURFACE ( )  );
#9705 = VERTEX_POINT ( 'NONE', #1763 ) ;
#9706 = AXIS2_PLACEMENT_3D ( 'NONE', #14265, #2924, #18606 ) ;
#9707 = EDGE_CURVE ( 'NONE', #9246, #23016, #16730, .T. ) ;
#9708 = ORIENTED_EDGE ( 'NONE', *, *, #350, .T. ) ;
#9709 = CARTESIAN_POINT ( 'NONE',  ( 6.224689322667647851, 89.08920297664211319, 118.2566963816774290 ) ) ;
#9710 = CARTESIAN_POINT ( 'NONE',  ( 109.1586059443104944, 0.006344953511159727791, -0.003127959656221018965 ) ) ;
#9711 = VECTOR ( 'NONE', #13463, 1000.000000000000114 ) ;
#9712 = AXIS2_PLACEMENT_3D ( 'NONE', #13885, #22398, #2664 ) ;
#9713 = CARTESIAN_POINT ( 'NONE',  ( -7.078251931573400491, 26.33626633876288636, 44.92740138729136135 ) ) ;
#9714 = CARTESIAN_POINT ( 'NONE',  ( 25.64708010899966695, -66.32331961783448548, 91.37928813995148403 ) ) ;
#9715 = CIRCLE ( 'NONE', #6500, 53.53553390275978785 ) ;
#9716 = EDGE_CURVE ( 'NONE', #14341, #23222, #23502, .T. ) ;
#9717 = CARTESIAN_POINT ( 'NONE',  ( 32.73300124599735739, -81.52272205837257957, 84.80615050150346690 ) ) ;
#9718 = B_SPLINE_CURVE_WITH_KNOTS ( 'NONE', 3,
 ( #11619, #20533, #18363, #17795 ),
 .UNSPECIFIED., .F., .F.,
 ( 4, 4 ),
 ( 1.906343156168367839E-16, 0.0009910334943227156780 ),
 .UNSPECIFIED. ) ;
#9719 = CARTESIAN_POINT ( 'NONE',  ( 109.1589550718175161, -0.003980125429509265116, -0.006445391216541633550 ) ) ;
#9720 = DIRECTION ( 'NONE',  ( 0.7563875759206388771, 0.4122509917856751471, -0.5078650950445667833 ) ) ;
#9721 = CARTESIAN_POINT ( 'NONE',  ( 55.49584447822657296, 48.34726110739985927, 54.09506550945642545 ) ) ;
#9723 = CARTESIAN_POINT ( 'NONE',  ( -1.048171036023497038, -13.17819047681634537, -43.86077206077064261 ) ) ;
#9722 = CARTESIAN_POINT ( 'NONE',  ( -4.473127245936431073, -45.82513704981557368, -18.25038884639852199 ) ) ;
#9724 = CARTESIAN_POINT ( 'NONE',  ( 119.2224693531408803, 90.00000000000005684, -19.99999999999998934 ) ) ;
#9725 = EDGE_CURVE ( 'NONE', #4266, #9035, #8903, .T. ) ;
#9726 = VERTEX_POINT ( 'NONE', #7032 ) ;
#9727 = ORIENTED_EDGE ( 'NONE', *, *, #7695, .F. ) ;
#9728 = CARTESIAN_POINT ( 'NONE',  ( -55.24271866751342941, -0.006671293903668846365, 0.006757859501006202411 ) ) ;
#9730 = CARTESIAN_POINT ( 'NONE',  ( 25.64708228042118421, -91.37028996123309810, 66.33571787052784430 ) ) ;
#9729 = CARTESIAN_POINT ( 'NONE',  ( 25.64700659047694842, 66.55152787776250989, -91.21315746821456116 ) ) ;
#9731 = B_SPLINE_CURVE_WITH_KNOTS ( 'NONE', 3,
 ( #20981, #5752, #14648, #14077, #14510, #3295, #5303, #990, #18834, #3568 ),
 .UNSPECIFIED., .F., .F.,
 ( 4, 2, 2, 2, 4 ),
 ( 2.168404344971008868E-19, 0.0003346267210630925128, 0.0006692534421261848087, 0.001003880163189277159, 0.001338506884252369401 ),
 .UNSPECIFIED. ) ;
#9732 = CARTESIAN_POINT ( 'NONE',  ( 1.833721034905632985, -85.00517831633766264, 117.6051524288280916 ) ) ;
#9733 = CARTESIAN_POINT ( 'NONE',  ( 94.22246935314088034, -151.1871800109700246, -6.938893903907228378E-15 ) ) ;
#9734 = CARTESIAN_POINT ( 'NONE',  ( 10.93730112726002623, 56.95489579269933955, -140.0398180619107507 ) ) ;
#9735 = EDGE_CURVE ( 'NONE', #1672, #10456, #2623, .T. ) ;
#9736 = EDGE_LOOP ( 'NONE', ( #6166, #12418, #19257, #20877 ) ) ;
#9737 = CARTESIAN_POINT ( 'NONE',  ( 25.86096068574582674, 98.40249579084591858, -55.66087367585303980 ) ) ;
#9738 = CARTESIAN_POINT ( 'NONE',  ( 1.832998868059858122, 144.2584710144580242, 15.69902610990423319 ) ) ;
#9739 = CARTESIAN_POINT ( 'NONE',  ( 55.49584447822657296, -29.26468316696818306, 66.38758986585106925 ) ) ;
#9740 = VERTEX_POINT ( 'NONE', #8574 ) ;
#9741 = CARTESIAN_POINT ( 'NONE',  ( 94.22246935314088034, -151.1871800109700246, 12.49999999999999467 ) ) ;
#9742 = AXIS2_PLACEMENT_3D ( 'NONE', #4707, #1832, #8607 ) ;
#9743 = DIRECTION ( 'NONE',  ( 0.7071067811865464625, -2.207942520024055603E-15, 0.7071067811865485719 ) ) ;
#9744 = CONICAL_SURFACE ( 'NONE', #17530, 117.6351876552689504, 0.9945805576725580410 ) ;
#9745 = ORIENTED_EDGE ( 'NONE', *, *, #23752, .F. ) ;
#9746 = CARTESIAN_POINT ( 'NONE',  ( -55.24340739397742084, -0.01010924026184288269, -0.0007387096945739216438 ) ) ;
#9747 = ORIENTED_EDGE ( 'NONE', *, *, #1276, .T. ) ;
#9748 = FACE_OUTER_BOUND ( 'NONE', #22041, .T. ) ;
#9749 = ORIENTED_EDGE ( 'NONE', *, *, #26566, .T. ) ;
#9750 = CARTESIAN_POINT ( 'NONE',  ( 881.1325374217881290, 957.9834503758418123, 1393.142638658674286 ) ) ;
#9751 = CARTESIAN_POINT ( 'NONE',  ( -55.24340739397742084, -0.002421372372453905585, -0.009842732675352267036 ) ) ;
#9752 = EDGE_CURVE ( 'NONE', #18844, #14777, #12229, .T. ) ;
#9753 = B_SPLINE_CURVE_WITH_KNOTS ( 'NONE', 3,
 ( #13928, #27453, #5152, #3003, #22882, #11785, #9617 ),
 .UNSPECIFIED., .F., .F.,
 ( 4, 3, 4 ),
 ( 0.000000000000000000, 0.006568092053401802279, 0.02506242213020847681 ),
 .UNSPECIFIED. ) ;
#9754 = CARTESIAN_POINT ( 'NONE',  ( -1.048996300304495310, 14.87787369922229708, 43.31387123529964356 ) ) ;
#9755 = CARTESIAN_POINT ( 'NONE',  ( 1.833838850093517880, 0.08898415480168050951, -145.1097630783160923 ) ) ;
#9756 = CARTESIAN_POINT ( 'NONE',  ( 109.1592201516379674, 0.002720803050361310545, -0.007376275279030886783 ) ) ;
#9757 = ADVANCED_FACE ( 'NONE', ( #2213 ), #24906, .F. ) ;
#9758 = VERTEX_POINT ( 'NONE', #24267 ) ;
#9759 = B_SPLINE_CURVE_WITH_KNOTS ( 'NONE', 3,
 ( #24727, #26850, #13468, #7158, #11454, #22708, #27280 ),
 .UNSPECIFIED., .F., .F.,
 ( 4, 3, 4 ),
 ( 1.913235636441834259E-16, 0.02816610861753247180, 0.04000277880656216006 ),
 .UNSPECIFIED. ) ;
#9761 =( BOUNDED_SURFACE ( )  B_SPLINE_SURFACE ( 3, 1, ( 
 ( #23600, #3859 ),
 ( #17229, #12624 ),
 ( #1684, #17088 ),
 ( #25881, #14925 ) ),
 .UNSPECIFIED., .F., .F., .F. ) 
 B_SPLINE_SURFACE_WITH_KNOTS ( ( 4, 4 ),
 ( 2, 2 ),
 ( 0.000000000000000000, 1.000000000000000000 ),
 ( 0.000000000000000000, 1.000000000000000000 ),
 .UNSPECIFIED. ) 
 GEOMETRIC_REPRESENTATION_ITEM ( )  RATIONAL_B_SPLINE_SURFACE ( (
 ( 1.000000000000000000, 1.000000000000000000),
 ( 0.9960225298536222738, 0.9999952330161893110),
 ( 0.9960225298536222738, 0.9999952330161893110),
 ( 1.000000000000000000, 1.000000000000000000) ) ) 
 REPRESENTATION_ITEM ( '' )  SURFACE ( )  );
#9760 = AXIS2_PLACEMENT_3D ( 'NONE', #7081, #8798, #13238 ) ;
#9762 = CARTESIAN_POINT ( 'NONE',  ( -1.045287976400362417, -15.59869763335038506, 43.05558670614261985 ) ) ;
#9763 = CARTESIAN_POINT ( 'NONE',  ( 2.430230287190592531, -137.9371479820465254, 46.34481016236778572 ) ) ;
#9764 = CARTESIAN_POINT ( 'NONE',  ( 10.93730112726006176, 142.1801301103792809, -51.37919228020152929 ) ) ;
#9765 = VERTEX_POINT ( 'NONE', #26128 ) ;
#9766 = AXIS2_PLACEMENT_3D ( 'NONE', #21186, #1470, #24209 ) ;
#9767 = EDGE_CURVE ( 'NONE', #4266, #10555, #27602, .T. ) ;
#9768 = VERTEX_POINT ( 'NONE', #9008 ) ;
#9769 = ORIENTED_EDGE ( 'NONE', *, *, #19441, .F. ) ;
#9770 = DIRECTION ( 'NONE',  ( 1.000000000000000000, -6.938893903907226837E-18, -5.541455922705464902E-20 ) ) ;
#9771 = CARTESIAN_POINT ( 'NONE',  ( 24.01988960052073452, 73.52806416354073349, 108.4726924928698679 ) ) ;
#9773 = CARTESIAN_POINT ( 'NONE',  ( 25.64692232868534560, 11.47740546588784483, -112.3263170481596234 ) ) ;
#9772 = CARTESIAN_POINT ( 'NONE',  ( 13.84597867724989229, 115.8103190066271679, 90.05293531772652216 ) ) ;
#9774 = CARTESIAN_POINT ( 'NONE',  ( 25.64681081121879203, 56.81519825470891760, -97.57530875170544959 ) ) ;
#9775 = CARTESIAN_POINT ( 'NONE',  ( 55.49584447822657296, -71.02133150427263786, 14.82242356767912561 ) ) ;
#9776 = CARTESIAN_POINT ( 'NONE',  ( -20.47566338032522637, -18.81547714195493626, -23.19796701701864805 ) ) ;
#9778 = ADVANCED_FACE ( 'NONE', ( #22249 ), #21014, .F. ) ;
#9777 = CARTESIAN_POINT ( 'NONE',  ( -55.24300891470650754, 0.009812809446893281523, -0.0003472257464216086005 ) ) ;
#9779 = ORIENTED_EDGE ( 'NONE', *, *, #6002, .F. ) ;
#9780 = CARTESIAN_POINT ( 'NONE',  ( 30.59141879584275969, 105.0379937202713734, 49.72305007553475775 ) ) ;
#9781 = CARTESIAN_POINT ( 'NONE',  ( -1.155031165708878094, -16.13806347973029176, -42.97366960678595404 ) ) ;
#9782 = CARTESIAN_POINT ( 'NONE',  ( 25.64670758986457244, 110.3390515846398472, 23.96231489924928937 ) ) ;
#9783 = CARTESIAN_POINT ( 'NONE',  ( 25.69398547355837437, -66.98507266663692405, -90.93418986874874577 ) ) ;
#9784 = CARTESIAN_POINT ( 'NONE',  ( 60.46576798286869803, 12.50000000000000000, 1.635699886147040789E-15 ) ) ;
#9785 = CARTESIAN_POINT ( 'NONE',  ( -20.24399999263414784, 16.36687688782894412, 24.70869149526185282 ) ) ;
#9786 = CARTESIAN_POINT ( 'NONE',  ( 26.28373643307438101, 118.1623717393431008, 48.05579805965559359 ) ) ;
#9787 = ORIENTED_EDGE ( 'NONE', *, *, #13803, .F. ) ;
#9788 = CARTESIAN_POINT ( 'NONE',  ( 1.834118845439484335, 58.85894970555094829, -132.6369225636068165 ) ) ;
#9789 = CARTESIAN_POINT ( 'NONE',  ( -25.21435515916043002, 34.05351380035335040, -6.169479169075572145 ) ) ;
#9791 = CARTESIAN_POINT ( 'NONE',  ( -1.113548883309542603, 12.28732181966579695, 44.18588492042577798 ) ) ;
#9790 = B_SPLINE_CURVE_WITH_KNOTS ( 'NONE', 3,
 ( #6746, #6461, #10642, #28043, #14941, #113 ),
 .UNSPECIFIED., .F., .F.,
 ( 4, 2, 4 ),
 ( 1.528920360908313465E-16, 0.003570751334075640462, 0.007141502668151127400 ),
 .UNSPECIFIED. ) ;
#9792 = AXIS2_PLACEMENT_3D ( 'NONE', #6750, #26038, #19828 ) ;
#9793 = VERTEX_POINT ( 'NONE', #28412 ) ;
#9794 = ORIENTED_EDGE ( 'NONE', *, *, #3193, .F. ) ;
#9795 = CIRCLE ( 'NONE', #17133, 37.50000000000002132 ) ;
#9796 = DIRECTION ( 'NONE',  ( 0.5946245182733607137, -0.08697490616139977315, 0.7992853357633863398 ) ) ;
#9797 = LINE ( 'NONE', #17102, #11409 ) ;
#9798 = CARTESIAN_POINT ( 'NONE',  ( 1.833206308920083183, 73.19872517709890758, -125.2945011813198164 ) ) ;
#9799 = CARTESIAN_POINT ( 'NONE',  ( -1.046935749539995131, -15.35946454248365711, 43.14401153755482454 ) ) ;
#9800 = CARTESIAN_POINT ( 'NONE',  ( 2.263178607246687069, 57.85473702627292170, -133.3897506477015895 ) ) ;
#9801 = CARTESIAN_POINT ( 'NONE',  ( 25.98552792386799482, 97.43552975939697092, -57.50018541500323721 ) ) ;
#9802 = ORIENTED_EDGE ( 'NONE', *, *, #11438, .F. ) ;
#9803 = CARTESIAN_POINT ( 'NONE',  ( -15.02187109954783928, 20.12219089991090115, -41.75590530176315696 ) ) ;
#9804 = EDGE_CURVE ( 'NONE', #22601, #8915, #10205, .T. ) ;
#9805 = CARTESIAN_POINT ( 'NONE',  ( 1.833485406944043827, 45.34878176254417070, -137.8414413349080974 ) ) ;
#9806 = CARTESIAN_POINT ( 'NONE',  ( -20.20612091757420004, -27.77903622052264865, -10.22177757278304888 ) ) ;
#9807 = ORIENTED_EDGE ( 'NONE', *, *, #8291, .F. ) ;
#9808 =( BOUNDED_SURFACE ( )  B_SPLINE_SURFACE ( 3, 1, ( 
 ( #27584, #25161 ),
 ( #1249, #7905 ),
 ( #972, #23432 ),
 ( #1120, #9763 ) ),
 .UNSPECIFIED., .F., .F., .F. ) 
 B_SPLINE_SURFACE_WITH_KNOTS ( ( 4, 4 ),
 ( 2, 2 ),
 ( 0.000000000000000000, 1.000000000000000000 ),
 ( 0.000000000000000000, 1.000000000000000000 ),
 .UNSPECIFIED. ) 
 GEOMETRIC_REPRESENTATION_ITEM ( )  RATIONAL_B_SPLINE_SURFACE ( (
 ( 1.000000000000000000, 1.000000000000000000),
 ( 0.6386103224230316178, 0.9954351624131538845),
 ( 0.6386103224230316178, 0.9954351624131538845),
 ( 1.000000000000000000, 1.000000000000000000) ) ) 
 REPRESENTATION_ITEM ( '' )  SURFACE ( )  );
#9809 = EDGE_CURVE ( 'NONE', #11495, #11877, #27362, .T. ) ;
#9810 = ORIENTED_EDGE ( 'NONE', *, *, #4383, .T. ) ;
#9811 = CARTESIAN_POINT ( 'NONE',  ( -25.21435515916043713, -31.17620025257598471, -15.02493970636134613 ) ) ;
#9812 = LINE ( 'NONE', #3745, #11620 ) ;
#9813 = CARTESIAN_POINT ( 'NONE',  ( 1.834118845439484335, 132.4921483272736396, -59.18411796426921967 ) ) ;
#9814 = ADVANCED_FACE ( 'NONE', ( #5246 ), #25978, .F. ) ;
#9815 = CARTESIAN_POINT ( 'NONE',  ( 2.263178113027032978, 144.4462808674010148, 16.59120315151625746 ) ) ;
#9816 = CARTESIAN_POINT ( 'NONE',  ( -4.162674018437137136, 37.46098494546635038, 31.44946543094254920 ) ) ;
#9817 = ORIENTED_EDGE ( 'NONE', *, *, #2155, .F. ) ;
#9818 = CARTESIAN_POINT ( 'NONE',  ( 25.86096068574579121, 84.67961880569399113, -74.90357932134547525 ) ) ;
#9819 = CARTESIAN_POINT ( 'NONE',  ( 2.430230287190581429, -137.9371479820459570, -46.34481016236964734 ) ) ;
#9820 = AXIS2_PLACEMENT_3D ( 'NONE', #3984, #12756, #26145 ) ;
#9821 = LINE ( 'NONE', #20888, #23 ) ;
#9822 = CARTESIAN_POINT ( 'NONE',  ( 2.430230287190589422, -57.85706160874236303, 133.5180086894989415 ) ) ;
#9823 = CARTESIAN_POINT ( 'NONE',  ( -1.045287976400362417, 43.05558670614268379, 15.59869763335023229 ) ) ;
#9824 = EDGE_LOOP ( 'NONE', ( #3101, #2916, #18624, #28207 ) ) ;
#9825 = CARTESIAN_POINT ( 'NONE',  ( -1.619063947482201282, 44.80407745103784123, -11.94059994246174838 ) ) ;
#9826 = ORIENTED_EDGE ( 'NONE', *, *, #10740, .T. ) ;
#9827 = ORIENTED_EDGE ( 'NONE', *, *, #8331, .T. ) ;
#9828 = VECTOR ( 'NONE', #12804, 1000.000000000000000 ) ;
#9829 = ORIENTED_EDGE ( 'NONE', *, *, #15631, .T. ) ;
#9830 = CARTESIAN_POINT ( 'NONE',  ( 1.831572820252009626, 125.1738732943820480, -73.40899645745874125 ) ) ;
#9831 = CARTESIAN_POINT ( 'NONE',  ( 30.58324630866346183, 45.56259622822511801, -112.0331114996530459 ) ) ;
#9832 = VECTOR ( 'NONE', #2127, 1000.000000000000000 ) ;
#9833 = ADVANCED_FACE ( 'NONE', ( #5099 ), #4154, .T. ) ;
#9834 = CARTESIAN_POINT ( 'NONE',  ( 109.1586059443104944, 0.005555961672780061582, 0.004378796245583053796 ) ) ;
#9835 = CARTESIAN_POINT ( 'NONE',  ( 1.831572820252008738, 142.1425225354583688, -29.20415387690428233 ) ) ;
#9836 = EDGE_CURVE ( 'NONE', #21724, #6278, #645, .T. ) ;
#9837 = B_SPLINE_CURVE_WITH_KNOTS ( 'NONE', 3,
 ( #15401, #23801, #19725, #4335 ),
 .UNSPECIFIED., .F., .F.,
 ( 4, 4 ),
 ( 0.000000000000000000, 0.01077107196513872600 ),
 .UNSPECIFIED. ) ;
#9838 = CARTESIAN_POINT ( 'NONE',  ( 25.64670758986458665, 107.5375791514047705, -34.41755235608631125 ) ) ;
#9839 = B_SPLINE_CURVE_WITH_KNOTS ( 'NONE', 3,
 ( #20149, #9223, #15841, #24648, #2293, #22874 ),
 .UNSPECIFIED., .F., .F.,
 ( 4, 2, 4 ),
 ( 9.341771812940338307E-18, 0.003576372551510817021, 0.007152745103021624501 ),
 .UNSPECIFIED. ) ;
#9840 = CARTESIAN_POINT ( 'NONE',  ( 1.833838848569443458, -85.43736077718784827, -117.2916552720327275 ) ) ;
#9842 = AXIS2_PLACEMENT_3D ( 'NONE', #17758, #19355, #15585 ) ;
#9841 = CARTESIAN_POINT ( 'NONE',  ( 25.64700659047693776, -75.38309044531831660, -84.06149911284524023 ) ) ;
#9843 = CARTESIAN_POINT ( 'NONE',  ( 32.73300124599732186, 0.000000000000000000, 0.000000000000000000 ) ) ;
#9844 = CARTESIAN_POINT ( 'NONE',  ( 25.64681081121879203, -83.63051021305953725, 75.86069728268962820 ) ) ;
#9845 = CARTESIAN_POINT ( 'NONE',  ( 25.64660436782549979, -22.90783756890928302, 110.5628080555245987 ) ) ;
#9846 = CARTESIAN_POINT ( 'NONE',  ( 55.49584447822657296, -66.38758986585096977, -29.26468316696839622 ) ) ;
#9847 = CARTESIAN_POINT ( 'NONE',  ( 25.64692232868534205, 83.69035111837304441, -75.79483800045692021 ) ) ;
#9848 =( BOUNDED_SURFACE ( )  B_SPLINE_SURFACE ( 3, 1, ( 
 ( #20891, #20599 ),
 ( #14554, #1177 ),
 ( #18733, #27506 ),
 ( #7815, #5645 ) ),
 .UNSPECIFIED., .F., .F., .F. ) 
 B_SPLINE_SURFACE_WITH_KNOTS ( ( 4, 4 ),
 ( 2, 2 ),
 ( 0.000000000000000000, 1.000000000000000000 ),
 ( 0.000000000000000000, 1.000000000000000000 ),
 .UNSPECIFIED. ) 
 GEOMETRIC_REPRESENTATION_ITEM ( )  RATIONAL_B_SPLINE_SURFACE ( (
 ( 1.000000000000000000, 1.000000000000000000),
 ( 0.9960225298536222738, 0.9999952330161893110),
 ( 0.9960225298536222738, 0.9999952330161893110),
 ( 1.000000000000000000, 1.000000000000000000) ) ) 
 REPRESENTATION_ITEM ( '' )  SURFACE ( )  );
#9849 = ORIENTED_EDGE ( 'NONE', *, *, #8778, .F. ) ;
#9850 = CARTESIAN_POINT ( 'NONE',  ( -20.20997486282892552, 1.395963739018065216E-16, 29.60348406988233450 ) ) ;
#9851 = ORIENTED_EDGE ( 'NONE', *, *, #20499, .T. ) ;
#9852 = DIRECTION ( 'NONE',  ( 0.000000000000000000, 5.223019709708233256E-21, -1.000000000000000000 ) ) ;
#9853 = CARTESIAN_POINT ( 'NONE',  ( 2.433796855181219243, -74.00833731765649759, 125.2830755159751703 ) ) ;
#9854 = EDGE_LOOP ( 'NONE', ( #9965, #6835, #13295, #18106 ) ) ;
#9855 = ORIENTED_EDGE ( 'NONE', *, *, #3260, .T. ) ;
#9856 = ORIENTED_EDGE ( 'NONE', *, *, #24763, .T. ) ;
#9857 = B_SPLINE_CURVE_WITH_KNOTS ( 'NONE', 3,
 ( #21783, #24092, #4355, #2175, #17588, #12839 ),
 .UNSPECIFIED., .F., .F.,
 ( 4, 2, 4 ),
 ( 1.041737195591640451E-17, 0.0006311571484586062228, 0.001262314296917201820 ),
 .UNSPECIFIED. ) ;
#9858 = LINE ( 'NONE', #27402, #24843 ) ;
#9859 = EDGE_CURVE ( 'NONE', #18908, #7560, #23254, .T. ) ;
#9860 = AXIS2_PLACEMENT_3D ( 'NONE', #6701, #19928, #4098 ) ;
#9861 = EDGE_CURVE ( 'NONE', #4452, #8562, #11440, .T. ) ;
#9862 = EDGE_CURVE ( 'NONE', #1581, #15484, #9154, .T. ) ;
#9863 = ADVANCED_FACE ( 'NONE', ( #5531 ), #16217, .F. ) ;
#9864 = CARTESIAN_POINT ( 'NONE',  ( -55.24340739397742794, -0.005344433640973866861, 0.008612749836242647450 ) ) ;
#9865 = DIRECTION ( 'NONE',  ( 0.000000000000000000, 0.000000000000000000, -1.000000000000000000 ) ) ;
#9866 = CARTESIAN_POINT ( 'NONE',  ( -55.24198130335446422, -0.004163123460802295971, -0.008310594958153156783 ) ) ;
#9867 = CARTESIAN_POINT ( 'NONE',  ( 30.59138290137884653, -99.26509990456052890, 60.43009393261933582 ) ) ;
#9868 = CARTESIAN_POINT ( 'NONE',  ( 109.1592201516379674, -0.004867031887019586216, -0.006174480289199391417 ) ) ;
#9869 = CARTESIAN_POINT ( 'NONE',  ( -1.259972190295308936, 25.19627397134298263, -38.49631882650656678 ) ) ;
#9870 = CARTESIAN_POINT ( 'NONE',  ( -20.21097721712958517, 17.13687106192379161, 24.14932359587270483 ) ) ;
#9872 = CARTESIAN_POINT ( 'NONE',  ( 109.1624594426973118, 0.01033277910989004525, -0.01216903288310966155 ) ) ;
#9871 = CARTESIAN_POINT ( 'NONE',  ( -20.38016308990357928, 10.62413300761025425, 27.81387210821410250 ) ) ;
#9873 = CARTESIAN_POINT ( 'NONE',  ( -1.619063947482197729, -43.26576862488445130, -16.67502769180545386 ) ) ;
#9874 = ORIENTED_EDGE ( 'NONE', *, *, #21320, .F. ) ;
#9875 = ORIENTED_EDGE ( 'NONE', *, *, #24327, .T. ) ;
#9876 = CARTESIAN_POINT ( 'NONE',  ( -1.046935749539997573, -27.93995161054667875, 36.28605774377793125 ) ) ;
#9878 = CARTESIAN_POINT ( 'NONE',  ( 1.832998868059858122, 125.9352106559983895, 72.09222286251124956 ) ) ;
#9877 = CARTESIAN_POINT ( 'NONE',  ( 32.73300124599732186, 0.000000000000000000, 0.000000000000000000 ) ) ;
#9879 = CARTESIAN_POINT ( 'NONE',  ( 1.833838850093477690, -85.29337590730617080, 117.3962664098819886 ) ) ;
#9880 = SURFACE_STYLE_USAGE ( .BOTH. , #1092 ) ;
#9881 = CARTESIAN_POINT ( 'NONE',  ( -1.044557008772710516, -36.05793264791363129, -28.22896138707358205 ) ) ;
#9882 = ORIENTED_EDGE ( 'NONE', *, *, #6141, .F. ) ;
#9883 = CARTESIAN_POINT ( 'NONE',  ( 25.65782528836482257, 98.07785559018951460, -55.95807498711376837 ) ) ;
#9884 =( BOUNDED_SURFACE ( )  B_SPLINE_SURFACE ( 3, 1, ( 
 ( #22755, #18248 ),
 ( #16101, #11493 ),
 ( #20565, #11797 ),
 ( #16247, #2719 ) ),
 .UNSPECIFIED., .F., .F., .F. ) 
 B_SPLINE_SURFACE_WITH_KNOTS ( ( 4, 4 ),
 ( 2, 2 ),
 ( 0.000000000000000000, 1.000000000000000000 ),
 ( 0.000000000000000000, 1.000000000000000000 ),
 .UNSPECIFIED. ) 
 GEOMETRIC_REPRESENTATION_ITEM ( )  RATIONAL_B_SPLINE_SURFACE ( (
 ( 1.000000000000000000, 1.000000000000000000),
 ( 0.6386103224230316178, 0.9954351624131538845),
 ( 0.6386103224230316178, 0.9954351624131538845),
 ( 1.000000000000000000, 1.000000000000000000) ) ) 
 REPRESENTATION_ITEM ( '' )  SURFACE ( )  );
#9885 = CARTESIAN_POINT ( 'NONE',  ( -55.25297051322618813, -0.001818774723749082148, -0.01483298743814642773 ) ) ;
#9886 = CARTESIAN_POINT ( 'NONE',  ( -55.24271866751342941, -0.001425019990781919424, 0.009388511352197656881 ) ) ;
#9887 = ORIENTED_EDGE ( 'NONE', *, *, #7796, .T. ) ;
#9888 = CARTESIAN_POINT ( 'NONE',  ( 25.64692232868534560, -97.62014907493917804, 56.73833653200207294 ) ) ;
#9889 = CARTESIAN_POINT ( 'NONE',  ( 109.1586900883932856, 0.002810909342011593849, 0.006561743627143341688 ) ) ;
#9890 = EDGE_CURVE ( 'NONE', #14469, #16227, #4671, .T. ) ;
#9891 = B_SPLINE_CURVE_WITH_KNOTS ( 'NONE', 3,
 ( #16354, #11612, #22718, #22566, #9895, #20818 ),
 .UNSPECIFIED., .F., .F.,
 ( 4, 2, 4 ),
 ( 0.000000000000000000, 0.0004335151646191517374, 0.0008670303292383034748 ),
 .UNSPECIFIED. ) ;
#9892 = B_SPLINE_CURVE_WITH_KNOTS ( 'NONE', 3,
 ( #3465, #27640, #21015, #18425, #18722, #1299, #18868, #16563 ),
 .UNSPECIFIED., .F., .F.,
 ( 4, 2, 2, 4 ),
 ( 0.000000000000000000, 0.002761524886576650645, 0.005523049773153301291, 0.01104609954630661299 ),
 .UNSPECIFIED. ) ;
#9893 = B_SPLINE_CURVE_WITH_KNOTS ( 'NONE', 3,
 ( #3629, #17686, #15235, #133, #1478, #8119, #13219, #10286 ),
 .UNSPECIFIED., .F., .F.,
 ( 4, 2, 2, 4 ),
 ( 0.000000000000000000, 0.0002429588503611232193, 0.0004859177007222464386, 0.0009718354014444878898 ),
 .UNSPECIFIED. ) ;
#9894 = ORIENTED_EDGE ( 'NONE', *, *, #10805, .T. ) ;
#9895 = CARTESIAN_POINT ( 'NONE',  ( -20.20612091757420004, -27.77903622052264865, -10.22177757278304888 ) ) ;
#9896 = EDGE_CURVE ( 'NONE', #27156, #1087, #6082, .T. ) ;
#9897 = EDGE_CURVE ( 'NONE', #14763, #18716, #12918, .T. ) ;
#9898 = ORIENTED_EDGE ( 'NONE', *, *, #9003, .T. ) ;
#9899 = CARTESIAN_POINT ( 'NONE',  ( -1.259920593601971950, -43.01175804832021043, -16.33409644610535594 ) ) ;
#9900 = DIRECTION ( 'NONE',  ( 0.7637818620346800147, 0.2198041754873883424, -0.6068965246771037547 ) ) ;
#9901 = EDGE_LOOP ( 'NONE', ( #539, #19619 ) ) ;
#9902 = CARTESIAN_POINT ( 'NONE',  ( -55.24300891470650754, -0.003362556190412219030, -0.009225237711101438864 ) ) ;
#9903 = CARTESIAN_POINT ( 'NONE',  ( -4.473127245936431073, 31.51789735524192793, -37.94261489385728936 ) ) ;
#9904 = CARTESIAN_POINT ( 'NONE',  ( 55.49584447822657296, -54.09506550945658887, 48.34726110739968163 ) ) ;
#9905 = CARTESIAN_POINT ( 'NONE',  ( 1.833838848569429247, -107.9566558236570160, -96.96512505224337986 ) ) ;
#9906 = ORIENTED_EDGE ( 'NONE', *, *, #153, .T. ) ;
#9907 = CARTESIAN_POINT ( 'NONE',  ( 13.36082413113061307, -9.660980093453659379, -152.6206443696329700 ) ) ;
#9909 = CARTESIAN_POINT ( 'NONE',  ( 10.93730112725945247, 97.44200844886275092, 115.5857507957704087 ) ) ;
#9908 = DIRECTION ( 'NONE',  ( 1.000000000000000000, -6.938893903907226837E-18, 1.734723475976806709E-18 ) ) ;
#9910 = CARTESIAN_POINT ( 'NONE',  ( -12.82751273423878757, -33.78816682541312844, -35.32125660155435298 ) ) ;
#9911 = ORIENTED_EDGE ( 'NONE', *, *, #23665, .T. ) ;
#9912 = ORIENTED_EDGE ( 'NONE', *, *, #26601, .F. ) ;
#9913 = ORIENTED_EDGE ( 'NONE', *, *, #74, .F. ) ;
#9914 = DIRECTION ( 'NONE',  ( 0.000000000000000000, 5.223019709708116647E-21, -1.000000000000000000 ) ) ;
#9915 = DIRECTION ( 'NONE',  ( 0.000000000000000000, 0.000000000000000000, 1.000000000000000000 ) ) ;
#9917 = CARTESIAN_POINT ( 'NONE',  ( 25.64692872815575342, 12.12228186621208259, -112.2585610031152186 ) ) ;
#9916 = CARTESIAN_POINT ( 'NONE',  ( 1.833838850855474822, 107.8971100408363100, -97.03125735562127829 ) ) ;
#9918 = CARTESIAN_POINT ( 'NONE',  ( 10.93730112725996051, -4.928439153519255989, -151.0983828010092793 ) ) ;
#9919 = CARTESIAN_POINT ( 'NONE',  ( 55.49584447822657296, -62.69727227546376014, -36.50733923851264251 ) ) ;
#9920 = VERTEX_POINT ( 'NONE', #17760 ) ;
#9921 = FACE_OUTER_BOUND ( 'NONE', #10652, .T. ) ;
#9922 = DIRECTION ( 'NONE',  ( 0.5914120900931444380, 0.1598001217819306763, 0.7903769105750361179 ) ) ;
#9923 = ORIENTED_EDGE ( 'NONE', *, *, #24422, .F. ) ;
#9924 = CARTESIAN_POINT ( 'NONE',  ( -21.81686047589425570, 33.92779429964205917, -18.24499610240053116 ) ) ;
#9925 = CARTESIAN_POINT ( 'NONE',  ( 109.1587776205901861, -0.004375189885423146942, -0.005880209827414109407 ) ) ;
#9926 = CARTESIAN_POINT ( 'NONE',  ( -1.049819825607589685, 13.66706894614437928, -43.71263398674757639 ) ) ;
#9927 = CARTESIAN_POINT ( 'NONE',  ( 109.1778270068192853, -0.001591747944959357852, -0.009177562596826695923 ) ) ;
#9928 = AXIS2_PLACEMENT_3D ( 'NONE', #20289, #860, #26905 ) ;
#9929 = FACE_OUTER_BOUND ( 'NONE', #21969, .T. ) ;
#9930 = LINE ( 'NONE', #12627, #12114 ) ;
#9931 = CARTESIAN_POINT ( 'NONE',  ( 2.063896406836605024, -144.3268707900446088, -16.52087515463925627 ) ) ;
#9932 = ORIENTED_EDGE ( 'NONE', *, *, #3578, .T. ) ;
#9933 = DIRECTION ( 'NONE',  ( -1.000000000000000000, -0.000000000000000000, -0.000000000000000000 ) ) ;
#9934 = EDGE_CURVE ( 'NONE', #12511, #21273, #7392, .T. ) ;
#9935 = FACE_OUTER_BOUND ( 'NONE', #26240, .T. ) ;
#9936 = LINE ( 'NONE', #11937, #28166 ) ;
#9937 = ADVANCED_FACE ( 'NONE', ( #11293 ), #4448, .F. ) ;
#9938 = B_SPLINE_CURVE_WITH_KNOTS ( 'NONE', 3,
 ( #5218, #22946, #20903, #16153 ),
 .UNSPECIFIED., .F., .F.,
 ( 4, 4 ),
 ( 0.000000000000000000, 0.01077107196513883008 ),
 .UNSPECIFIED. ) ;
#9939 = ORIENTED_EDGE ( 'NONE', *, *, #17627, .T. ) ;
#9940 = ORIENTED_EDGE ( 'NONE', *, *, #13846, .T. ) ;
#9941 = EDGE_CURVE ( 'NONE', #15546, #211, #15308, .T. ) ;
#9942 = CARTESIAN_POINT ( 'NONE',  ( -1.045287976400365970, -45.76855895860947498, -1.530335034933654859 ) ) ;
#9943 =( BOUNDED_SURFACE ( )  B_SPLINE_SURFACE ( 3, 1, ( 
 ( #1307, #15096 ),
 ( #21313, #14829 ),
 ( #1594, #14964 ),
 ( #10394, #23644 ) ),
 .UNSPECIFIED., .F., .F., .F. ) 
 B_SPLINE_SURFACE_WITH_KNOTS ( ( 4, 4 ),
 ( 2, 2 ),
 ( 0.000000000000000000, 1.000000000000000000 ),
 ( 0.000000000000000000, 1.000000000000000000 ),
 .UNSPECIFIED. ) 
 GEOMETRIC_REPRESENTATION_ITEM ( )  RATIONAL_B_SPLINE_SURFACE ( (
 ( 1.000000000000000000, 1.000000000000000000),
 ( 0.9960225298536222738, 0.9999952330161893110),
 ( 0.9960225298536222738, 0.9999952330161893110),
 ( 1.000000000000000000, 1.000000000000000000) ) ) 
 REPRESENTATION_ITEM ( '' )  SURFACE ( )  );
#9944 = CARTESIAN_POINT ( 'NONE',  ( 2.430230287190589422, -74.01081053031012402, -125.2872625092170153 ) ) ;
#9945 = EDGE_CURVE ( 'NONE', #18731, #10482, #9837, .T. ) ;
#9946 = VERTEX_POINT ( 'NONE', #15743 ) ;
#9947 = CARTESIAN_POINT ( 'NONE',  ( -1.031422197589716205, 1.530725436378091553, 45.78027046666442601 ) ) ;
#9948 = CARTESIAN_POINT ( 'NONE',  ( 25.64703792032472052, -23.32999623362200126, 110.4746717456748542 ) ) ;
#9949 = CARTESIAN_POINT ( 'NONE',  ( -2.904412668506679118, 46.12477647685274462, -11.97478724945526629 ) ) ;
#9950 = APPLICATION_CONTEXT ( 'automotive_design' ) ;
#9951 = CARTESIAN_POINT ( 'NONE',  ( 25.64681081121879203, 97.57530875170606066, 56.81519825470789442 ) ) ;
#9952 = CARTESIAN_POINT ( 'NONE',  ( 1.833838850855476599, -59.10274688031942958, 132.5281727421684366 ) ) ;
#9953 = CARTESIAN_POINT ( 'NONE',  ( 2.063896406836609909, -133.2511741302116945, -57.85593781835549265 ) ) ;
#9954 = ORIENTED_EDGE ( 'NONE', *, *, #23489, .T. ) ;
#9955 = ORIENTED_EDGE ( 'NONE', *, *, #23216, .T. ) ;
#9956 = CARTESIAN_POINT ( 'NONE',  ( -28.13707043255157103, 7.802116958609002673, -21.52861750560941800 ) ) ;
#9957 = B_SPLINE_CURVE_WITH_KNOTS ( 'NONE', 3,
 ( #8043, #18809, #25157, #12326 ),
 .UNSPECIFIED., .F., .F.,
 ( 4, 4 ),
 ( 1.904170172768910460E-16, 0.001982023823822945917 ),
 .UNSPECIFIED. ) ;
#9958 = CARTESIAN_POINT ( 'NONE',  ( -1.583189561560256253, -46.33203782964459805, 2.490696082060350314 ) ) ;
#9959 = CARTESIAN_POINT ( 'NONE',  ( 109.1624594426973118, -0.01033277910988996545, 0.01216903288310973094 ) ) ;
#9960 = DIRECTION ( 'NONE',  ( 0.5946245182733607137, 0.4045541647807479602, -0.6948076064830646104 ) ) ;
#9961 = CARTESIAN_POINT ( 'NONE',  ( -1.619063947482197729, 2.489035965910801895, 46.30105812165545842 ) ) ;
#9962 = LINE ( 'NONE', #5481, #5682 ) ;
#9963 = B_SPLINE_CURVE_WITH_KNOTS ( 'NONE', 3,
 ( #2180, #4362, #24680, #6820 ),
 .UNSPECIFIED., .F., .F.,
 ( 4, 4 ),
 ( 3.465291969645973218E-16, 0.01077107486149812138 ),
 .UNSPECIFIED. ) ;
#9964 = CARTESIAN_POINT ( 'NONE',  ( -1.045287976400365970, -45.76855895860947498, -1.530335034933654859 ) ) ;
#9965 = ORIENTED_EDGE ( 'NONE', *, *, #17212, .T. ) ;
#9966 = CARTESIAN_POINT ( 'NONE',  ( 1.833721034905634095, 59.34646046113778084, 132.4192200895884355 ) ) ;
#9967 = CARTESIAN_POINT ( 'NONE',  ( -12.94347594948484037, -35.22469990145630447, -33.69581619287863106 ) ) ;
#9968 = CARTESIAN_POINT ( 'NONE',  ( 25.65782528836480481, -11.22838748007539955, -112.3587790429871660 ) ) ;
#9969 = CARTESIAN_POINT ( 'NONE',  ( -20.47566262905010248, -16.24827521404668929, -25.06314747784830388 ) ) ;
#9970 = CARTESIAN_POINT ( 'NONE',  ( 25.64704443564079028, 0.1334765861219636696, -112.9111375659905718 ) ) ;
#9971 = ORIENTED_EDGE ( 'NONE', *, *, #2351, .F. ) ;
#9972 = CARTESIAN_POINT ( 'NONE',  ( 25.64681081121879203, -56.81519825470687834, -97.57530875170664331 ) ) ;
#9973 = CARTESIAN_POINT ( 'NONE',  ( -21.81686047589426636, -5.181745222995193245, 38.17230180719262478 ) ) ;
#9974 = ORIENTED_EDGE ( 'NONE', *, *, #5946, .T. ) ;
#9975 = EDGE_CURVE ( 'NONE', #16334, #13261, #28358, .T. ) ;
#9976 = VERTEX_POINT ( 'NONE', #26488 ) ;
#9977 = ORIENTED_EDGE ( 'NONE', *, *, #15891, .F. ) ;
#9978 = EDGE_CURVE ( 'NONE', #6273, #19910, #8, .T. ) ;
#9979 = B_SPLINE_CURVE_WITH_KNOTS ( 'NONE', 3,
 ( #9017, #19652, #2089, #1954 ),
 .UNSPECIFIED., .F., .F.,
 ( 4, 4 ),
 ( 0.000000000000000000, 0.01077107196513880927 ),
 .UNSPECIFIED. ) ;
#9980 = CARTESIAN_POINT ( 'NONE',  ( 25.64681081121879203, 66.03065707439057519, -91.59071981940505225 ) ) ;
#9981 = CARTESIAN_POINT ( 'NONE',  ( 10.93730112725982195, -145.2260730187404079, 42.00474393596209666 ) ) ;
#9982 =( BOUNDED_SURFACE ( )  B_SPLINE_SURFACE ( 3, 1, ( 
 ( #21989, #19827 ),
 ( #256, #15492 ),
 ( #26582, #28320 ),
 ( #8756, #21859 ) ),
 .UNSPECIFIED., .F., .F., .F. ) 
 B_SPLINE_SURFACE_WITH_KNOTS ( ( 4, 4 ),
 ( 2, 2 ),
 ( 0.000000000000000000, 1.000000000000000000 ),
 ( 0.000000000000000000, 1.000000000000000000 ),
 .UNSPECIFIED. ) 
 GEOMETRIC_REPRESENTATION_ITEM ( )  RATIONAL_B_SPLINE_SURFACE ( (
 ( 1.000000000000000000, 1.000000000000000000),
 ( 0.6386103224230316178, 0.9954351624131538845),
 ( 0.6386103224230316178, 0.9954351624131538845),
 ( 1.000000000000000000, 1.000000000000000000) ) ) 
 REPRESENTATION_ITEM ( '' )  SURFACE ( )  );
#9983 = CARTESIAN_POINT ( 'NONE',  ( 6.224689322667647851, -89.08920297664128896, -118.2566963816780259 ) ) ;
#9984 = CARTESIAN_POINT ( 'NONE',  ( 109.1586900883932856, 0.006130969560693665978, 0.003656351050324904359 ) ) ;
#9985 = CARTESIAN_POINT ( 'NONE',  ( 30.58324630866350802, 120.6294372749319734, 8.712468656081018281 ) ) ;
#9986 = CARTESIAN_POINT ( 'NONE',  ( 25.70243777736190438, 112.9457924277214005, 0.7331659071599172517 ) ) ;
#9987 = CARTESIAN_POINT ( 'NONE',  ( -4.178947244162635855, 3.367451375481794074, 48.81675275154071869 ) ) ;
#9988 = CARTESIAN_POINT ( 'NONE',  ( 2.433796855181205476, -137.9325382748282038, -46.34326152018883249 ) ) ;
#9989 = CARTESIAN_POINT ( 'NONE',  ( 25.64681081121879203, 84.18689316040146764, -75.24277141833410099 ) ) ;
#9990 = CARTESIAN_POINT ( 'NONE',  ( 1.833485406944043827, -0.5339064996894915538, 145.1085452359073145 ) ) ;
#9991 = CARTESIAN_POINT ( 'NONE',  ( 10.93730112725972958, -84.82621002473526062, 125.1380233598475229 ) ) ;
#9992 = CARTESIAN_POINT ( 'NONE',  ( -1.259920593601972838, -2.243284667987463621, 45.95412615877144447 ) ) ;
#9993 = CARTESIAN_POINT ( 'NONE',  ( 28.37599760073042532, -86.45296943207071649, 75.42809173301579051 ) ) ;
#9994 = DIRECTION ( 'NONE',  ( -1.000000000000000000, -0.000000000000000000, -0.000000000000000000 ) ) ;
#9995 = CARTESIAN_POINT ( 'NONE',  ( 10.93730112726006354, 145.2260730187408626, -42.00474393596100953 ) ) ;
#9996 = ORIENTED_EDGE ( 'NONE', *, *, #10953, .T. ) ;
#9997 = CARTESIAN_POINT ( 'NONE',  ( -1.539760825549678636, 25.17088484262142956, -38.84664866728784460 ) ) ;
#9998 = ORIENTED_EDGE ( 'NONE', *, *, #1624, .T. ) ;
#9999 = CARTESIAN_POINT ( 'NONE',  ( -20.37983603106074426, 7.753708011498974706, 28.74620395171554321 ) ) ;
#10000 = LINE ( 'NONE', #16765, #24503 ) ;
#10001 = ORIENTED_EDGE ( 'NONE', *, *, #11435, .F. ) ;
#10002 = EDGE_CURVE ( 'NONE', #11368, #9397, #21610, .T. ) ;
#10003 = VERTEX_POINT ( 'NONE', #8801 ) ;
#10004 = ORIENTED_EDGE ( 'NONE', *, *, #10601, .F. ) ;
#10005 = ADVANCED_FACE ( 'NONE', ( #17285 ), #13108, .F. ) ;
#10006 = EDGE_CURVE ( 'NONE', #23613, #20885, #19779, .T. ) ;
#10007 = B_SPLINE_CURVE_WITH_KNOTS ( 'NONE', 3,
 ( #10129, #1053, #3206, #7986, #16747, #13853, #2928, #9840, #18610, #22661 ),
 .UNSPECIFIED., .F., .F.,
 ( 4, 3, 3, 4 ),
 ( 3.925231146709437917E-17, 0.0002669559177086094437, 0.0005339118354150799734, 0.001067817517169168152 ),
 .UNSPECIFIED. ) ;
#10008 = B_SPLINE_CURVE_WITH_KNOTS ( 'NONE', 3,
 ( #17014, #25684, #28471, #5959, #27679, #25395, #8776, #14711 ),
 .UNSPECIFIED., .F., .F.,
 ( 4, 2, 2, 4 ),
 ( 0.000000000000000000, 0.0002429588503611195872, 0.0004859177007222391744, 0.0009718354014444835530 ),
 .UNSPECIFIED. ) ;
#10009 = CARTESIAN_POINT ( 'NONE',  ( 32.73300124599735739, 75.82012867748483131, 89.94078864464094636 ) ) ;
#10010 = CARTESIAN_POINT ( 'NONE',  ( -21.81686047589426991, 37.90526371014259155, -6.867757412720813193 ) ) ;
#10011 = CARTESIAN_POINT ( 'NONE',  ( -20.57838717382308147, 23.26537097894132344, 18.89542499756474569 ) ) ;
#10012 = CARTESIAN_POINT ( 'NONE',  ( 109.1592201516379674, -0.005027640251764426034, 0.006044422199831456753 ) ) ;
#10013 = CARTESIAN_POINT ( 'NONE',  ( 109.1586900883932856, -0.006757191295056145380, 0.002301750759607874407 ) ) ;
#10014 =( BOUNDED_SURFACE ( )  B_SPLINE_SURFACE ( 3, 1, ( 
 ( #21206, #23107 ),
 ( #14583, #27242 ),
 ( #7403, #27683 ),
 ( #7704, #10143 ) ),
 .UNSPECIFIED., .F., .F., .F. ) 
 B_SPLINE_SURFACE_WITH_KNOTS ( ( 4, 4 ),
 ( 2, 2 ),
 ( 0.000000000000000000, 1.000000000000000000 ),
 ( 0.000000000000000000, 1.000000000000000000 ),
 .UNSPECIFIED. ) 
 GEOMETRIC_REPRESENTATION_ITEM ( )  RATIONAL_B_SPLINE_SURFACE ( (
 ( 1.000000000000000000, 1.000000000000000000),
 ( 0.9956975270656954757, 0.8568959468854893125),
 ( 0.9956975270656954757, 0.8568959468854893125),
 ( 1.000000000000000000, 1.000000000000000000) ) ) 
 REPRESENTATION_ITEM ( '' )  SURFACE ( )  );
#10015 = CARTESIAN_POINT ( 'NONE',  ( 109.1586900883932856, -0.004113747441000958037, -0.005833932871487499359 ) ) ;
#10017 = CARTESIAN_POINT ( 'NONE',  ( 1.831572820252008738, -145.1082523917587253, -0.9871191512929762268 ) ) ;
#10016 = CARTESIAN_POINT ( 'NONE',  ( -20.57838717382308147, 10.78122205917039977, 27.96569011373074076 ) ) ;
#10018 = CARTESIAN_POINT ( 'NONE',  ( -6.588769196390761529, -47.06982923582523171, -20.50531526814544847 ) ) ;
#10019 = EDGE_LOOP ( 'NONE', ( #19772, #10873, #20375, #3505 ) ) ;
#10020 = ORIENTED_EDGE ( 'NONE', *, *, #27328, .F. ) ;
#10021 = CARTESIAN_POINT ( 'NONE',  ( 1.832998868059858122, 0.5339089137768276982, -145.1092030902949830 ) ) ;
#10023 = CARTESIAN_POINT ( 'NONE',  ( 25.64681081121879203, 56.81519825470891760, -97.57530875170544959 ) ) ;
#10022 = CARTESIAN_POINT ( 'NONE',  ( -1.323439229708139875, 28.92147054731892908, 35.86372896917441722 ) ) ;
#10024 = CARTESIAN_POINT ( 'NONE',  ( 2.433796855181205476, 13.76554153471693454, 144.8571464219890004 ) ) ;
#10025 = CARTESIAN_POINT ( 'NONE',  ( 25.64660436782554598, 11.22538561722038253, -112.3516544824818908 ) ) ;
#10026 = CARTESIAN_POINT ( 'NONE',  ( -55.24728320129491266, 0.01214321324516798306, 0.008013189884950450148 ) ) ;
#10027 = ADVANCED_FACE ( 'NONE', ( #20014 ), #13438, .F. ) ;
#10028 = ORIENTED_EDGE ( 'NONE', *, *, #20710, .F. ) ;
#10029 = DIRECTION ( 'NONE',  ( 0.000000000000000000, 0.000000000000000000, 1.000000000000000000 ) ) ;
#10030 = CARTESIAN_POINT ( 'NONE',  ( 25.81918753295376945, -35.81374485821542208, -107.2019194967339217 ) ) ;
#10031 = CARTESIAN_POINT ( 'NONE',  ( 1.833485406944043827, -15.69895494453482598, 144.2578170162062463 ) ) ;
#10032 = ORIENTED_EDGE ( 'NONE', *, *, #6231, .F. ) ;
#10033 = CARTESIAN_POINT ( 'NONE',  ( -20.20700224038492010, 16.58740185276710832, -24.51628800869052682 ) ) ;
#10034 = EDGE_CURVE ( 'NONE', #9343, #2712, #21493, .T. ) ;
#10035 = CARTESIAN_POINT ( 'NONE',  ( 2.430230287190581429, -28.83279105684324861, -142.6294793592101087 ) ) ;
#10036 = ORIENTED_EDGE ( 'NONE', *, *, #27227, .T. ) ;
#10037 = CARTESIAN_POINT ( 'NONE',  ( -20.20700224038492721, 28.44216453106536946, -8.199606986804427677 ) ) ;
#10038 = EDGE_LOOP ( 'NONE', ( #26783, #28158, #6950, #15121, #795, #9238, #9499, #14997, #21748, #24717, #20838, #21490, #3987, #4947, #21659, #16996, #26928, #16852, #12450, #15455, #13755, #24945, #19261, #23446, #3053, #11202, #1526, #26334, #6612, #3292, #9592, #28169, #529, #514, #22418, #20798, #20774, #4832, #24494, #14408, #18881, #3243, #4744, #24018, #13325, #22268, #9855, #21054, #6708, #25848, #1756, #3423, #17217, #23283, #20024, #18858, #19631, #1540, #27913, #6308, #18436, #27128, #6130, #14838 ) ) ;
#10039 = CARTESIAN_POINT ( 'NONE',  ( 30.59138290137886429, -116.1811451928593613, 2.701446546447824115 ) ) ;
#10040 = B_SPLINE_CURVE_WITH_KNOTS ( 'NONE', 3,
 ( #3232, #3511, #18633, #2693 ),
 .UNSPECIFIED., .F., .F.,
 ( 4, 4 ),
 ( 1.962615573354718958E-17, 0.008383560773332699931 ),
 .UNSPECIFIED. ) ;
#10041 = DIRECTION ( 'NONE',  ( 1.765987723262725394E-16, -0.9908497996140103181, -0.1349691616810137496 ) ) ;
#10042 = B_SPLINE_CURVE_WITH_KNOTS ( 'NONE', 3,
 ( #7163, #18078, #14043, #20815, #11458, #9593, #13616 ),
 .UNSPECIFIED., .F., .F.,
 ( 4, 3, 4 ),
 ( 5.645319006159137796E-16, 0.02816610861753248221, 0.04000277880656271517 ),
 .UNSPECIFIED. ) ;
#10043 = CARTESIAN_POINT ( 'NONE',  ( -28.41354790283022069, -22.41474081377996441, 5.969609727608259142 ) ) ;
#10044 = CARTESIAN_POINT ( 'NONE',  ( 25.86096068574581608, -46.89265070732192697, 102.8701285401540275 ) ) ;
#10045 = CARTESIAN_POINT ( 'NONE',  ( 2.063896406836609909, 31.51663808384556731, 141.8093313989361661 ) ) ;
#10046 = ORIENTED_EDGE ( 'NONE', *, *, #5717, .F. ) ;
#10047 = CARTESIAN_POINT ( 'NONE',  ( -4.473127245936431073, 47.80062405537802306, -12.17046501147532567 ) ) ;
#10049 = CARTESIAN_POINT ( 'NONE',  ( 109.1592201516379674, 0.003476928926134712113, 0.007051465909552774060 ) ) ;
#10048 = CARTESIAN_POINT ( 'NONE',  ( -1.239374126674604337, 38.61989855450939046, -25.08410696974256027 ) ) ;
#10050 = DIRECTION ( 'NONE',  ( 0.000000000000000000, 5.223019709707975211E-21, -1.000000000000000000 ) ) ;
#10051 = ORIENTED_EDGE ( 'NONE', *, *, #23561, .T. ) ;
#10052 = ORIENTED_EDGE ( 'NONE', *, *, #1276, .F. ) ;
#10053 = ORIENTED_EDGE ( 'NONE', *, *, #135, .T. ) ;
#10054 = CARTESIAN_POINT ( 'NONE',  ( -1.619063947482197729, 2.489035965910159298, -46.30105812165548684 ) ) ;
#10055 = CARTESIAN_POINT ( 'NONE',  ( 28.37644542392847669, 69.76573497039082383, 102.9230687709010681 ) ) ;
#10057 = CARTESIAN_POINT ( 'NONE',  ( 25.64699802086722968, 11.56593161917464485, -112.3172869996024446 ) ) ;
#10056 = CARTESIAN_POINT ( 'NONE',  ( 1.833485406944057594, 107.4794113447422603, -97.49333871408586560 ) ) ;
#10058 = CARTESIAN_POINT ( 'NONE',  ( 2.433796855181233454, 133.5135467655518369, 57.85512797797937168 ) ) ;
#10059 = CARTESIAN_POINT ( 'NONE',  ( 32.73300124599738581, 75.82012867748602503, -89.94078864463983791 ) ) ;
#10060 = EDGE_LOOP ( 'NONE', ( #18146, #14973, #1953, #25637 ) ) ;
#10061 = CARTESIAN_POINT ( 'NONE',  ( -55.24300891470650754, 0.009439835024159288004, 0.002702093572893217704 ) ) ;
#10062 = VECTOR ( 'NONE', #1331, 1000.000000000000227 ) ;
#10063 = CARTESIAN_POINT ( 'NONE',  ( 8.186469829614228644, -90.56875932797659345, 118.7566730983345309 ) ) ;
#10064 = EDGE_CURVE ( 'NONE', #20693, #16059, #11915, .T. ) ;
#10065 = VERTEX_POINT ( 'NONE', #4192 ) ;
#10066 = CARTESIAN_POINT ( 'NONE',  ( -7.733045908741333463, 45.70676731105722723, -25.81515396910878479 ) ) ;
#10067 = VECTOR ( 'NONE', #14579, 1000.000000000000341 ) ;
#10068 = CARTESIAN_POINT ( 'NONE',  ( 13.36082413113063083, 143.3553710183996941, -53.25066407421655157 ) ) ;
#10069 = CARTESIAN_POINT ( 'NONE',  ( 2.430230287190589422, 116.8646894862423835, -86.70145658344540607 ) ) ;
#10070 = EDGE_CURVE ( 'NONE', #15181, #733, #20698, .T. ) ;
#10071 = DIRECTION ( 'NONE',  ( 0.5946245182733607137, -0.7637359336799405263, -0.2512550613902199692 ) ) ;
#10072 = CARTESIAN_POINT ( 'NONE',  ( -55.25297051322618813, 0.007247191603129411047, -0.01306918787467283537 ) ) ;
#10073 = CARTESIAN_POINT ( 'NONE',  ( 109.1624594426973260, -0.002129375066970737307, 0.01582142368018301520 ) ) ;
#10074 = ORIENTED_EDGE ( 'NONE', *, *, #347, .F. ) ;
#10075 = CARTESIAN_POINT ( 'NONE',  ( 28.37644542392839853, -29.80435743554031092, 120.7150203538607940 ) ) ;
#10076 = CARTESIAN_POINT ( 'NONE',  ( 1.833691583653482171, -29.82175144857997395, -142.0122737882512354 ) ) ;
#10077 = FACE_OUTER_BOUND ( 'NONE', #12124, .T. ) ;
#10078 = EDGE_LOOP ( 'NONE', ( #23748, #4723, #12559, #28072 ) ) ;
#10079 = CARTESIAN_POINT ( 'NONE',  ( -1.044557008772710516, -1.643388457097570088, 45.76404748504492659 ) ) ;
#10080 = EDGE_LOOP ( 'NONE', ( #23501, #13320, #7043, #14445 ) ) ;
#10081 = CARTESIAN_POINT ( 'NONE',  ( -1.046935749539990468, -45.77872888003169294, -1.275486069320314497 ) ) ;
#10082 = CARTESIAN_POINT ( 'NONE',  ( 25.87036335909427365, -102.8789780196092352, 46.88819766600075667 ) ) ;
#10083 = CARTESIAN_POINT ( 'NONE',  ( -55.24271866751342941, -0.004365563123935077734, -0.008433070970613952902 ) ) ;
#10084 = AXIS2_PLACEMENT_3D ( 'NONE', #21010, #14677, #12936 ) ;
#10085 = CARTESIAN_POINT ( 'NONE',  ( 30.59138290137920890, 109.6600423140547633, -38.47117663195857773 ) ) ;
#10086 = CARTESIAN_POINT ( 'NONE',  ( -55.24390624410018802, -0.001451500391952595045, 0.01032895241566660592 ) ) ;
#10087 = CARTESIAN_POINT ( 'NONE',  ( 1.833750490713684345, 141.8829662951652608, 30.43107162405918942 ) ) ;
#10088 = CARTESIAN_POINT ( 'NONE',  ( 1.833838848569443458, -125.7577269771227009, -72.40075357737779882 ) ) ;
#10089 = CARTESIAN_POINT ( 'NONE',  ( 25.64681081121879203, 112.2483031020015147, -12.21581276189692211 ) ) ;
#10090 = LINE ( 'NONE', #27631, #6757 ) ;
#10091 = ORIENTED_EDGE ( 'NONE', *, *, #10307, .T. ) ;
#10092 = EDGE_CURVE ( 'NONE', #3668, #18167, #10828, .T. ) ;
#10093 = EDGE_LOOP ( 'NONE', ( #20315, #12772, #10944, #16399 ) ) ;
#10094 = CARTESIAN_POINT ( 'NONE',  ( 6.224689322667647851, 57.86870174583612680, -136.2818611715185000 ) ) ;
#10095 = ADVANCED_FACE ( 'NONE', ( #9084 ), #16398, .F. ) ;
#10096 = DIRECTION ( 'NONE',  ( 1.000000000000000000, -6.938893903907226837E-18, 1.734723475976806709E-18 ) ) ;
#10097 = CARTESIAN_POINT ( 'NONE',  ( 26.11404676487259024, -112.7148551500679616, -10.71016160607683432 ) ) ;
#10098 = CARTESIAN_POINT ( 'NONE',  ( 1.833206308920071193, 144.2348261777516143, 15.90849808441927671 ) ) ;
#10099 = CARTESIAN_POINT ( 'NONE',  ( 5.340103579038292025, 108.0219267094759630, -100.3626145943024284 ) ) ;
#10100 = DIRECTION ( 'NONE',  ( -1.000000000000000000, 6.938893903907226837E-18, -1.734723475976806709E-18 ) ) ;
#10101 = ORIENTED_EDGE ( 'NONE', *, *, #11159, .F. ) ;
#10102 = CARTESIAN_POINT ( 'NONE',  ( -15.02187109954786060, -8.264310930412701595, -45.60876405941874623 ) ) ;
#10103 = CARTESIAN_POINT ( 'NONE',  ( 26.11404676487259024, -112.7148551500679616, -10.71016160607683432 ) ) ;
#10104 = CARTESIAN_POINT ( 'NONE',  ( -20.20612091757420359, -23.26073043121646933, -18.30568244821369817 ) ) ;
#10105 = EDGE_CURVE ( 'NONE', #5234, #9758, #13675, .T. ) ;
#10106 = CARTESIAN_POINT ( 'NONE',  ( -8.786685647604885574, 6.069026232697080105E-17, 53.53553390275978785 ) ) ;
#10107 = ADVANCED_FACE ( 'NONE', ( #13823 ), #6312, .F. ) ;
#10108 = ORIENTED_EDGE ( 'NONE', *, *, #22784, .F. ) ;
#10109 = ORIENTED_EDGE ( 'NONE', *, *, #14938, .T. ) ;
#10110 = CARTESIAN_POINT ( 'NONE',  ( 25.64660436782535058, -56.95711784271921374, -97.49251393956843970 ) ) ;
#10111 = B_SPLINE_CURVE_WITH_KNOTS ( 'NONE', 3,
 ( #7961, #12668, #16990, #14686, #21453, #23492, #12384, #19431 ),
 .UNSPECIFIED., .F., .F.,
 ( 4, 2, 2, 4 ),
 ( 7.857287273937903510E-18, 0.0002429592666046824793, 0.0004859185332093570982, 0.0009718370664186868745 ),
 .UNSPECIFIED. ) ;
#10112 = CARTESIAN_POINT ( 'NONE',  ( 109.1587776205901577, 0.003736572840486944002, -0.006305329297952431099 ) ) ;
#10113 = ORIENTED_EDGE ( 'NONE', *, *, #7894, .T. ) ;
#10114 = ORIENTED_EDGE ( 'NONE', *, *, #20987, .T. ) ;
#10115 = ORIENTED_EDGE ( 'NONE', *, *, #28046, .F. ) ;
#10116 =( REPRESENTATION_RELATIONSHIP ('NONE','NONE', #15430, #747 ) REPRESENTATION_RELATIONSHIP_WITH_TRANSFORMATION ( #24233 )SHAPE_REPRESENTATION_RELATIONSHIP( ) );
#10117 = CARTESIAN_POINT ( 'NONE',  ( -9.156249394959713683, 24.29252099376560281, 48.78605533024713026 ) ) ;
#10118 = CARTESIAN_POINT ( 'NONE',  ( 14.74894986621300141, 12.50000000000000000, 1.596046867330078713E-15 ) ) ;
#10119 = CARTESIAN_POINT ( 'NONE',  ( 1.833485406944043827, 30.69200235379130959, -141.8265699653863976 ) ) ;
#10120 = CARTESIAN_POINT ( 'NONE',  ( 1.833485406944043827, -97.49333871408762775, 107.4794113447406119 ) ) ;
#10121 = AXIS2_PLACEMENT_3D ( 'NONE', #25179, #20855, #5891 ) ;
#10122 = CARTESIAN_POINT ( 'NONE',  ( -1.323439229708125886, 2.317790194800380288, 46.01398008004440499 ) ) ;
#10123 = EDGE_LOOP ( 'NONE', ( #17720, #1729, #3794, #3431, #22435, #26984 ) ) ;
#10124 = EDGE_CURVE ( 'NONE', #10550, #6273, #14967, .T. ) ;
#10125 = B_SPLINE_CURVE_WITH_KNOTS ( 'NONE', 3,
 ( #26106, #327, #22222, #24540, #6539, #26522, #6688, #15432, #2485, #4500 ),
 .UNSPECIFIED., .F., .F.,
 ( 4, 3, 3, 4 ),
 ( 0.000000000000000000, 0.0002669560319015632562, 0.0005492286108966289854, 0.0008315040496093541135 ),
 .UNSPECIFIED. ) ;
#10126 = CARTESIAN_POINT ( 'NONE',  ( 13.36082413113063083, 6.345145185218039607, 152.7944199136427699 ) ) ;
#10127 = CARTESIAN_POINT ( 'NONE',  ( -5.986830583229484581, 4.559539818181838733, 50.53158596890435916 ) ) ;
#10128 = EDGE_CURVE ( 'NONE', #15825, #2900, #26219, .T. ) ;
#10129 = CARTESIAN_POINT ( 'NONE',  ( 1.833485406944043827, -84.86072343962486286, -117.7091014914958578 ) ) ;
#10130 = CARTESIAN_POINT ( 'NONE',  ( 28.37599760073042532, -33.74340001061027294, -109.6580863494833409 ) ) ;
#10131 = CARTESIAN_POINT ( 'NONE',  ( 25.64681081121879203, -11.38886654529750331, 112.3352186517030447 ) ) ;
#10132 = EDGE_CURVE ( 'NONE', #24473, #12568, #8451, .T. ) ;
#10133 = CARTESIAN_POINT ( 'NONE',  ( -55.25719721206881729, 0.008651607285660455754, 0.007063345920777159767 ) ) ;
#10134 = CARTESIAN_POINT ( 'NONE',  ( 25.81918753295380498, 76.32043280377813232, 83.36706424720470920 ) ) ;
#10136 = CARTESIAN_POINT ( 'NONE',  ( 25.64681081121879203, -91.10197563707900770, -66.70335573067958990 ) ) ;
#10135 = CARTESIAN_POINT ( 'NONE',  ( 25.64699802086721547, -0.2377811728589946105, -112.9109702078780657 ) ) ;
#10137 = CARTESIAN_POINT ( 'NONE',  ( -8.786685647604890903, -9.545808661480982948, -52.67761315067281913 ) ) ;
#10138 = CARTESIAN_POINT ( 'NONE',  ( 10.93730112725978110, -119.3442956573278479, 92.80059208661636205 ) ) ;
#10139 = CARTESIAN_POINT ( 'NONE',  ( 19.66333377628714985, 132.3257119126255077, -38.27269871460917017 ) ) ;
#10140 = EDGE_LOOP ( 'NONE', ( #8049, #23881, #16067, #23246 ) ) ;
#10141 = CARTESIAN_POINT ( 'NONE',  ( 2.430230287190592531, 31.67257033707503311, 142.0258656395022570 ) ) ;
#10142 = ORIENTED_EDGE ( 'NONE', *, *, #18278, .T. ) ;
#10143 = CARTESIAN_POINT ( 'NONE',  ( 1.832998868059858122, 141.8272129421612817, -30.69214149073875930 ) ) ;
#10145 = ORIENTED_EDGE ( 'NONE', *, *, #23686, .T. ) ;
#10144 = CARTESIAN_POINT ( 'NONE',  ( 26.11404676487259024, 36.06104232266452669, 107.3263591096431639 ) ) ;
#10146 = VERTEX_POINT ( 'NONE', #3044 ) ;
#10147 = AXIS2_PLACEMENT_3D ( 'NONE', #27694, #10558, #5969 ) ;
#10148 = VERTEX_POINT ( 'NONE', #7359 ) ;
#10149 = ORIENTED_EDGE ( 'NONE', *, *, #22243, .F. ) ;
#10150 = B_SPLINE_CURVE_WITH_KNOTS ( 'NONE', 3,
 ( #9679, #24953, #16444, #11982, #5064, #10120 ),
 .UNSPECIFIED., .F., .F.,
 ( 4, 2, 4 ),
 ( 6.505213034913026604E-18, 0.0006311636237756815130, 0.001262327247551356738 ),
 .UNSPECIFIED. ) ;
#10151 = B_SPLINE_CURVE_WITH_KNOTS ( 'NONE', 3,
 ( #25502, #27785, #3592, #12370, #21150, #1436 ),
 .UNSPECIFIED., .F., .F.,
 ( 4, 2, 4 ),
 ( 9.745765416140531346E-18, 0.0006311636237756778267, 0.001262327247551345679 ),
 .UNSPECIFIED. ) ;
#10152 = CARTESIAN_POINT ( 'NONE',  ( -25.21435515916043713, -34.05351380035337883, -6.169479169075319014 ) ) ;
#10153 = CARTESIAN_POINT ( 'NONE',  ( -18.41936578851709427, -38.22933728004704790, -18.42310649277614232 ) ) ;
#10154 = VECTOR ( 'NONE', #499, 1000.000000000000000 ) ;
#10155 = CARTESIAN_POINT ( 'NONE',  ( 1.834118845439484335, 125.7578880615055255, -72.40084790867199160 ) ) ;
#10156 = EDGE_CURVE ( 'NONE', #13750, #13485, #4765, .T. ) ;
#10157 = AXIS2_PLACEMENT_3D ( 'NONE', #20924, #7568, #18323 ) ;
#10158 = CARTESIAN_POINT ( 'NONE',  ( -22.23226125620930205, 31.55376588768478285, -2.179935373562563061 ) ) ;
#10160 = CARTESIAN_POINT ( 'NONE',  ( -8.786685647604885574, 6.096987947571466530E-17, -1.524246986892866633E-17 ) ) ;
#10159 = CARTESIAN_POINT ( 'NONE',  ( -1.323439229708128106, -44.47813215539053999, -12.01475235539429143 ) ) ;
#10161 = CARTESIAN_POINT ( 'NONE',  ( -20.57838717382308147, -7.715628353033481268, 28.96176188950225949 ) ) ;
#10162 = VECTOR ( 'NONE', #7608, 1000.000000000000000 ) ;
#10163 = EDGE_CURVE ( 'NONE', #21210, #14489, #17918, .T. ) ;
#10164 = ORIENTED_EDGE ( 'NONE', *, *, #9501, .T. ) ;
#10165 = DIRECTION ( 'NONE',  ( -1.000000000000000000, -0.000000000000000000, -0.000000000000000000 ) ) ;
#10167 = CARTESIAN_POINT ( 'NONE',  ( 25.64692232868534560, -91.15460455808870677, 66.63160215461235225 ) ) ;
#10166 = CARTESIAN_POINT ( 'NONE',  ( 10.93730112725971892, -10.89264110825104837, 150.7858122213660863 ) ) ;
#10168 = EDGE_CURVE ( 'NONE', #12213, #14162, #9656, .T. ) ;
#10169 = CARTESIAN_POINT ( 'NONE',  ( 1.833485406944043827, -85.72460230293772554, 117.0814567582541201 ) ) ;
#10170 = CARTESIAN_POINT ( 'NONE',  ( 109.1592201516379674, 0.007845213074660002325, 0.0005146241775907644525 ) ) ;
#10171 = CARTESIAN_POINT ( 'NONE',  ( 25.86096068574579832, 92.04529103340867380, -65.64181925268235318 ) ) ;
#10172 = ORIENTED_EDGE ( 'NONE', *, *, #9559, .F. ) ;
#10173 = CARTESIAN_POINT ( 'NONE',  ( 32.73300124599732186, 0.000000000000000000, 0.000000000000000000 ) ) ;
#10174 = CARTESIAN_POINT ( 'NONE',  ( -1.619063947482194177, 35.99532424477422410, 29.22875152547716482 ) ) ;
#10175 = FACE_OUTER_BOUND ( 'NONE', #7127, .T. ) ;
#10176 = ORIENTED_EDGE ( 'NONE', *, *, #25192, .T. ) ;
#10177 = CARTESIAN_POINT ( 'NONE',  ( -1.583189561560253589, 11.94859433442901597, -44.83405390829675952 ) ) ;
#10178 = CARTESIAN_POINT ( 'NONE',  ( -1.464342487929856107, -29.09292098541686755, -35.90631960086405883 ) ) ;
#10179 = ORIENTED_EDGE ( 'NONE', *, *, #16257, .T. ) ;
#10180 = ORIENTED_EDGE ( 'NONE', *, *, #23231, .F. ) ;
#10181 = CIRCLE ( 'NONE', #28073, 34.60786435723138510 ) ;
#10182 = VECTOR ( 'NONE', #12611, 1000.000000000000000 ) ;
#10183 = B_SPLINE_CURVE_WITH_KNOTS ( 'NONE', 3,
 ( #3440, #1557, #23453, #12352, #5603, #8325, #25884, #6181 ),
 .UNSPECIFIED., .F., .F.,
 ( 4, 2, 2, 4 ),
 ( 3.469446951953614189E-18, 0.0002429588503611278543, 0.0004859177007222522391, 0.0009718354014444750963 ),
 .UNSPECIFIED. ) ;
#10184 = CARTESIAN_POINT ( 'NONE',  ( 2.263178607246654206, -86.59154415224521983, -116.7985473178711970 ) ) ;
#10185 = VECTOR ( 'NONE', #28010, 999.9999999999998863 ) ;
#10186 = EDGE_LOOP ( 'NONE', ( #2138, #27562, #8371, #827 ) ) ;
#10187 = CARTESIAN_POINT ( 'NONE',  ( -1.619063947482197729, -43.26576862488445130, -16.67502769180545386 ) ) ;
#10188 = DIRECTION ( 'NONE',  ( -1.000000000000000000, -0.000000000000000000, -0.000000000000000000 ) ) ;
#10189 = DIRECTION ( 'NONE',  ( 1.000000000000000000, 0.000000000000000000, 0.000000000000000000 ) ) ;
#10190 = CARTESIAN_POINT ( 'NONE',  ( 32.73300124599734318, 81.52272205837205377, 84.80615050150403533 ) ) ;
#10191 =( BOUNDED_SURFACE ( )  B_SPLINE_SURFACE ( 3, 1, ( 
 ( #7360, #9519 ),
 ( #18270, #5190 ),
 ( #3045, #20589 ),
 ( #25072, #3598 ) ),
 .UNSPECIFIED., .F., .F., .F. ) 
 B_SPLINE_SURFACE_WITH_KNOTS ( ( 4, 4 ),
 ( 2, 2 ),
 ( 0.000000000000000000, 1.000000000000000000 ),
 ( 0.000000000000000000, 1.000000000000000000 ),
 .UNSPECIFIED. ) 
 GEOMETRIC_REPRESENTATION_ITEM ( )  RATIONAL_B_SPLINE_SURFACE ( (
 ( 1.000000000000000000, 1.000000000000000000),
 ( 0.9956975270656955868, 0.8568959468854907557),
 ( 0.9956975270656955868, 0.8568959468854907557),
 ( 1.000000000000000000, 1.000000000000000000) ) ) 
 REPRESENTATION_ITEM ( '' )  SURFACE ( )  );
#10192 = CARTESIAN_POINT ( 'NONE',  ( -4.473127245936434626, 49.22197550883368677, -3.196405119333975087 ) ) ;
#10193 = CARTESIAN_POINT ( 'NONE',  ( 25.64681081121879203, 66.70335573067866619, 91.10197563707968982 ) ) ;
#10194 = CARTESIAN_POINT ( 'NONE',  ( -55.24390624410018802, -0.007245494385991085341, 0.007503127514277716827 ) ) ;
#10195 = CARTESIAN_POINT ( 'NONE',  ( 1.833603222531974275, -107.5392551439147582, -97.42748212378386086 ) ) ;
#10196 = EDGE_CURVE ( 'NONE', #11003, #1646, #27200, .T. ) ;
#10197 = ORIENTED_EDGE ( 'NONE', *, *, #22095, .F. ) ;
#10198 = CARTESIAN_POINT ( 'NONE',  ( 9.884929003653608603, -11.54837932062929440, -150.0922431698406285 ) ) ;
#10200 = CARTESIAN_POINT ( 'NONE',  ( 24.22246935314087324, -90.00000000000005684, -40.00000000000002842 ) ) ;
#10199 = CARTESIAN_POINT ( 'NONE',  ( -1.031422197589711764, 37.93675465142472802, -25.67058493451456158 ) ) ;
#10201 = CARTESIAN_POINT ( 'NONE',  ( -28.41354790283022069, 5.969609727608021998, -22.41474081378002836 ) ) ;
#10202 = ORIENTED_EDGE ( 'NONE', *, *, #6903, .T. ) ;
#10203 = VECTOR ( 'NONE', #26618, 1000.000000000000114 ) ;
#10204 = ORIENTED_EDGE ( 'NONE', *, *, #2222, .F. ) ;
#10206 = ORIENTED_EDGE ( 'NONE', *, *, #12267, .T. ) ;
#10205 = B_SPLINE_CURVE_WITH_KNOTS ( 'NONE', 3,
 ( #8713, #24839, #20207, #352, #9714, #13733, #14153, #25120, #22687, #7569 ),
 .UNSPECIFIED., .F., .F.,
 ( 4, 3, 3, 4 ),
 ( 1.387778780781445676E-17, 0.0002669560319015616299, 0.0005492286108966353822, 0.0008315040496093367662 ),
 .UNSPECIFIED. ) ;
#10207 = CARTESIAN_POINT ( 'NONE',  ( 5.340103579038268933, -47.74933483136786805, -139.5040934216405333 ) ) ;
#10208 = B_SPLINE_CURVE_WITH_KNOTS ( 'NONE', 3,
 ( #20715, #19136, #7789, #10082, #5617, #23194, #16702, #18849 ),
 .UNSPECIFIED., .F., .F.,
 ( 4, 2, 2, 4 ),
 ( 3.469446951953614189E-18, 0.0002429592666046686829, 0.0004859185332093338963, 0.0009718370664186767914 ),
 .UNSPECIFIED. ) ;
#10209 = CARTESIAN_POINT ( 'NONE',  ( -20.57838717382308147, -27.96569011373078339, 10.78122205917029675 ) ) ;
#10211 = CARTESIAN_POINT ( 'NONE',  ( 25.64681081121879203, 12.21581276189956711, -112.2483031020012305 ) ) ;
#10210 = CARTESIAN_POINT ( 'NONE',  ( -2.904412668506669348, -46.12477647685265936, 11.97478724945559136 ) ) ;
#10212=STYLED_ITEM('',(#28500),#8673);
#10213 = CARTESIAN_POINT ( 'NONE',  ( -21.41427618760457818, 28.68857606049983744, 11.22988868156155640 ) ) ;
#10214 = CARTESIAN_POINT ( 'NONE',  ( -1.323830074806773061, -12.01461446423233781, -44.47857376182264488 ) ) ;
#10215 = CARTESIAN_POINT ( 'NONE',  ( -1.044557008772713624, 12.57891310333411106, 44.03203053429556491 ) ) ;
#10216 = CARTESIAN_POINT ( 'NONE',  ( -1.323830074806776391, -44.47857376182260936, 12.01461446423248169 ) ) ;
#10217 = ORIENTED_EDGE ( 'NONE', *, *, #15518, .F. ) ;
#10218 = CARTESIAN_POINT ( 'NONE',  ( -2.904412668506670681, 40.16685646686207889, -25.64203923793588302 ) ) ;
#10219 = CARTESIAN_POINT ( 'NONE',  ( -20.20700224038492010, 16.58740185276710832, -24.51628800869052682 ) ) ;
#10220 = AXIS2_PLACEMENT_3D ( 'NONE', #13387, #19728, #2748 ) ;
#10221 = CARTESIAN_POINT ( 'NONE',  ( 28.37599760073040400, 37.15642189426546338, -108.5491283158098383 ) ) ;
#10222 = CARTESIAN_POINT ( 'NONE',  ( 10.93730112725932635, 0.000000000000000000, 0.000000000000000000 ) ) ;
#10223 = CARTESIAN_POINT ( 'NONE',  ( -7.078251931573400491, -50.86685171665403260, 11.16394717458729957 ) ) ;
#10224 = CARTESIAN_POINT ( 'NONE',  ( 1.831572820252008738, -126.1609924456735143, 71.69925593429763921 ) ) ;
#10225 = EDGE_LOOP ( 'NONE', ( #21915, #16208, #24122, #6584 ) ) ;
#10226 = CARTESIAN_POINT ( 'NONE',  ( 13.36082413113063083, 9.660980093456728923, -152.6206443696327710 ) ) ;
#10227 = CARTESIAN_POINT ( 'NONE',  ( 109.1586059443104944, -0.005983234375919703821, -0.003774052605959013398 ) ) ;
#10228 = CARTESIAN_POINT ( 'NONE',  ( 28.43349137099830060, 111.8014342888394594, -54.21282462801664792 ) ) ;
#10229 = VERTEX_POINT ( 'NONE', #26771 ) ;
#10230 = CARTESIAN_POINT ( 'NONE',  ( 32.73300124599738581, 16.10546300444979195, -116.5274707358853163 ) ) ;
#10231 = VERTEX_POINT ( 'NONE', #5331 ) ;
#10232 = CARTESIAN_POINT ( 'NONE',  ( 30.59141879584286983, -70.47510900703845493, 92.40465812955523006 ) ) ;
#10233 = B_SPLINE_CURVE_WITH_KNOTS ( 'NONE', 3,
 ( #9450, #15917, #13467, #24857, #22707, #13748 ),
 .UNSPECIFIED., .F., .F.,
 ( 4, 2, 4 ),
 ( 4.341940435234061368E-16, 0.003576372551511239426, 0.007152745103022045171 ),
 .UNSPECIFIED. ) ;
#10234 = CARTESIAN_POINT ( 'NONE',  ( 109.1587776205901577, 0.001442274045003904149, 0.007186028091163438464 ) ) ;
#10235 = EDGE_CURVE ( 'NONE', #23267, #21777, #26657, .T. ) ;
#10236 = AXIS2_PLACEMENT_3D ( 'NONE', #12000, #18619, #1062 ) ;
#10237 = EDGE_CURVE ( 'NONE', #20294, #14489, #19458, .T. ) ;
#10238 = DIRECTION ( 'NONE',  ( -0.7637818620346801257, 0.6068965246771014233, -0.2198041754873946707 ) ) ;
#10239 = CARTESIAN_POINT ( 'NONE',  ( -55.25719721206881729, 0.01041086141212315547, 0.004044147484874825726 ) ) ;
#10240 = CARTESIAN_POINT ( 'NONE',  ( 1.833838848569415925, 141.9757689770221987, 29.99593366454804055 ) ) ;
#10241 = EDGE_CURVE ( 'NONE', #3267, #27654, #7089, .T. ) ;
#10242 = CARTESIAN_POINT ( 'NONE',  ( 5.340103579038241399, -75.71042924122960471, -126.5279493327092837 ) ) ;
#10243 = DIRECTION ( 'NONE',  ( 0.000000000000000000, -5.223019709708233256E-21, 1.000000000000000000 ) ) ;
#10244 = CARTESIAN_POINT ( 'NONE',  ( -1.259972190295307382, 28.82609802125311660, 35.85909728507018457 ) ) ;
#10245 = ORIENTED_EDGE ( 'NONE', *, *, #6840, .T. ) ;
#10246 = ORIENTED_EDGE ( 'NONE', *, *, #25410, .T. ) ;
#10247 = CARTESIAN_POINT ( 'NONE',  ( 25.98107933586735996, -97.42660475433896750, -57.50946808479330485 ) ) ;
#10248 = CARTESIAN_POINT ( 'NONE',  ( -55.24340739397742084, 0.007744344507855094144, 0.006539691034612383526 ) ) ;
#10249 = FACE_OUTER_BOUND ( 'NONE', #24208, .T. ) ;
#10250 = CARTESIAN_POINT ( 'NONE',  ( 25.64699802086724034, -84.06830990999276310, -75.37548011155811878 ) ) ;
#10251 = CARTESIAN_POINT ( 'NONE',  ( 25.64660436782551756, -91.68669413043107852, -65.89729635303008592 ) ) ;
#10252 = CARTESIAN_POINT ( 'NONE',  ( 25.64692232868535982, -91.53874134430752463, -66.10288322707289410 ) ) ;
#10253 = FACE_OUTER_BOUND ( 'NONE', #26360, .T. ) ;
#10254 = ORIENTED_EDGE ( 'NONE', *, *, #2162, .T. ) ;
#10255 = CARTESIAN_POINT ( 'NONE',  ( 1.833485406944043827, -144.3694338680886062, 14.63699153649312201 ) ) ;
#10256 = CARTESIAN_POINT ( 'NONE',  ( -1.239374126674604337, 28.97829083655491544, 35.79060836339782270 ) ) ;
#10257 = CARTESIAN_POINT ( 'NONE',  ( 25.86096068574579832, -10.82483750674526668, -112.5344699600050262 ) ) ;
#10258 = CARTESIAN_POINT ( 'NONE',  ( -55.25297051322618813, 0.006313402748433540913, -0.01354497706059917470 ) ) ;
#10259 = CARTESIAN_POINT ( 'NONE',  ( 55.49584447822657296, -15.34602024131236497, -70.91003759562332220 ) ) ;
#10260 = VECTOR ( 'NONE', #12193, 1000.000000000000000 ) ;
#10261 = CARTESIAN_POINT ( 'NONE',  ( 55.79472521941428198, -68.96476385670678155, 23.17337251492740080 ) ) ;
#10262 = CIRCLE ( 'NONE', #20323, 151.1787379149930359 ) ;
#10263 = ORIENTED_EDGE ( 'NONE', *, *, #12637, .F. ) ;
#10264 = CARTESIAN_POINT ( 'NONE',  ( -2.904412668506659578, -36.79926976721470311, -30.27712468694973325 ) ) ;
#10265 = CARTESIAN_POINT ( 'NONE',  ( -1.619063947482194177, -46.30105812165547974, 2.489035965910640247 ) ) ;
#10266 = VERTEX_POINT ( 'NONE', #23207 ) ;
#10267 = VERTEX_POINT ( 'NONE', #23061 ) ;
#10268 = VERTEX_POINT ( 'NONE', #7662 ) ;
#10269 = EDGE_CURVE ( 'NONE', #6096, #2848, #6067, .T. ) ;
#10270 = B_SPLINE_CURVE_WITH_KNOTS ( 'NONE', 3,
 ( #13036, #1800, #28416, #13167 ),
 .UNSPECIFIED., .F., .F.,
 ( 4, 4 ),
 ( 0.000000000000000000, 0.008383560773332715543 ),
 .UNSPECIFIED. ) ;
#10271 = B_SPLINE_CURVE_WITH_KNOTS ( 'NONE', 3,
 ( #4582, #10933, #17680, #26459, #15649, #24466, #4731 ),
 .UNSPECIFIED., .F., .F.,
 ( 4, 3, 4 ),
 ( 0.000000000000000000, 0.02398743853561285944, 0.04000277880656218782 ),
 .UNSPECIFIED. ) ;
#10272 = B_SPLINE_CURVE_WITH_KNOTS ( 'NONE', 3,
 ( #24064, #22462, #4456, #4324, #10947, #13368 ),
 .UNSPECIFIED., .F., .F.,
 ( 4, 2, 4 ),
 ( 3.409603294638168262E-16, 0.003576372551511143149, 0.007152745103021945425 ),
 .UNSPECIFIED. ) ;
#10273 = LINE ( 'NONE', #14260, #27575 ) ;
#10274 = CARTESIAN_POINT ( 'NONE',  ( 25.64681081121879203, 97.99105938547923245, 56.09509703373377931 ) ) ;
#10275 = EDGE_CURVE ( 'NONE', #17261, #20966, #18071, .T. ) ;
#10276 = DIRECTION ( 'NONE',  ( 0.000000000000000000, 0.000000000000000000, 1.000000000000000000 ) ) ;
#10277 = AXIS2_PLACEMENT_3D ( 'NONE', #21265, #10610, #25735 ) ;
#10278 = AXIS2_PLACEMENT_3D ( 'NONE', #1398, #7912, #7470 ) ;
#10279 = CARTESIAN_POINT ( 'NONE',  ( 109.1721716018069515, -0.01695288006056417524, -0.001984900887706834635 ) ) ;
#10280 = CARTESIAN_POINT ( 'NONE',  ( 9.884929003653626367, 4.203795436552358211, 150.4771565009630763 ) ) ;
#10282 = B_SPLINE_CURVE_WITH_KNOTS ( 'NONE', 3,
 ( #25053, #27326, #3019, #3157, #11935, #23188, #27611 ),
 .UNSPECIFIED., .F., .F.,
 ( 4, 3, 4 ),
 ( 0.000000000000000000, 0.02398743853561341455, 0.04000277880656216700 ),
 .UNSPECIFIED. ) ;
#10281 = CARTESIAN_POINT ( 'NONE',  ( -8.259864102781676820, 6.590267880897663133, 52.60025989855196116 ) ) ;
#10283 = CARTESIAN_POINT ( 'NONE',  ( 1.833485406944043827, -138.1714136985311256, 44.33323125129879116 ) ) ;
#10284 = CARTESIAN_POINT ( 'NONE',  ( 25.64692872815577473, -75.31297890941213780, -84.12425003484119657 ) ) ;
#10285 = CARTESIAN_POINT ( 'NONE',  ( 109.1624594426973118, 0.003771499231554082537, 0.01551217196237752310 ) ) ;
#10286 = CARTESIAN_POINT ( 'NONE',  ( 26.11404676487257603, -113.2169081140373947, -1.130420376098323576 ) ) ;
#10287 = CARTESIAN_POINT ( 'NONE',  ( -55.24728320129491266, -0.01402509393918105647, -0.003868537197316873795 ) ) ;
#10288 = B_SPLINE_CURVE_WITH_KNOTS ( 'NONE', 3,
 ( #21542, #25876, #14921, #21408, #8319, #12483 ),
 .UNSPECIFIED., .F., .F.,
 ( 4, 2, 4 ),
 ( 1.491862189340054101E-16, 0.003570751334075637860, 0.007141502668151126533 ),
 .UNSPECIFIED. ) ;
#10289 = CARTESIAN_POINT ( 'NONE',  ( 25.64670758986457955, 112.2393466678478262, 12.29747533046004548 ) ) ;
#10290 = CARTESIAN_POINT ( 'NONE',  ( 32.73300124599738581, -62.10906484417165530, -99.90245962373897726 ) ) ;
#10291 = CARTESIAN_POINT ( 'NONE',  ( 2.433796855181233454, 31.67151202412969724, 142.0211193075556935 ) ) ;
#10292 = CARTESIAN_POINT ( 'NONE',  ( 25.65782528836480481, 102.9197507294676086, 46.45532072021219960 ) ) ;
#10293 = ORIENTED_EDGE ( 'NONE', *, *, #18, .T. ) ;
#10294 = CIRCLE ( 'NONE', #24514, 117.6351876552689504 ) ;
#10295 = ORIENTED_EDGE ( 'NONE', *, *, #18998, .F. ) ;
#10296 = CARTESIAN_POINT ( 'NONE',  ( -20.47566262905010603, 23.19796652405701565, 18.81547655725221091 ) ) ;
#10297 = CARTESIAN_POINT ( 'NONE',  ( -25.21435515916025594, 1.749597353048488237E-16, -4.373993382621220594E-17 ) ) ;
#10298 = EDGE_LOOP ( 'NONE', ( #2341, #5980, #21174, #24942 ) ) ;
#10299 = VECTOR ( 'NONE', #6291, 1000.000000000000114 ) ;
#10300 = ORIENTED_EDGE ( 'NONE', *, *, #15831, .F. ) ;
#10301 = VECTOR ( 'NONE', #10238, 1000.000000000000000 ) ;
#10302 = ORIENTED_EDGE ( 'NONE', *, *, #1078, .T. ) ;
#10303 = ADVANCED_FACE ( 'NONE', ( #3321 ), #1444, .T. ) ;
#10304 = EDGE_CURVE ( 'NONE', #2416, #21273, #22213, .T. ) ;
#10305 = EDGE_CURVE ( 'NONE', #19603, #15408, #21304, .T. ) ;
#10306 = CARTESIAN_POINT ( 'NONE',  ( 1.833603222531974719, -142.0304769734131014, 29.73464781350211084 ) ) ;
#10307 = EDGE_CURVE ( 'NONE', #23680, #27723, #7439, .T. ) ;
#10308 = CARTESIAN_POINT ( 'NONE',  ( -1.031422197589716205, -25.67058493451416368, 37.93675465142500514 ) ) ;
#10309 = LINE ( 'NONE', #23540, #5658 ) ;
#10310 = LINE ( 'NONE', #21362, #8395 ) ;
#10311 = CARTESIAN_POINT ( 'NONE',  ( -55.24390624410018802, -0.007245494385991085341, 0.007503127514277716827 ) ) ;
#10312 = CARTESIAN_POINT ( 'NONE',  ( -1.619063947482197729, -44.80407745103793360, -11.94059994246142331 ) ) ;
#10313 = CARTESIAN_POINT ( 'NONE',  ( 55.49584447822657296, -68.91748907713603955, 22.67407039687217818 ) ) ;
#10314 = ORIENTED_EDGE ( 'NONE', *, *, #22204, .T. ) ;
#10315 = ORIENTED_EDGE ( 'NONE', *, *, #1801, .F. ) ;
#10316 = B_SPLINE_CURVE_WITH_KNOTS ( 'NONE', 3,
 ( #22911, #11948, #20720, #22324 ),
 .UNSPECIFIED., .F., .F.,
 ( 4, 4 ),
 ( 3.417011720166793662E-16, 0.01077107486149841975 ),
 .UNSPECIFIED. ) ;
#10318 = CARTESIAN_POINT ( 'NONE',  ( -1.056502255334264895, -13.66916755949820583, 43.72121397317236102 ) ) ;
#10317 = DIRECTION ( 'NONE',  ( -1.000000000000000000, -0.000000000000000000, -0.000000000000000000 ) ) ;
#10319 = FACE_OUTER_BOUND ( 'NONE', #24220, .T. ) ;
#10320 = CARTESIAN_POINT ( 'NONE',  ( -20.20700224038492365, 8.199606986804329978, -28.44216453106539078 ) ) ;
#10321 = CARTESIAN_POINT ( 'NONE',  ( -25.21435515916025594, 1.749597353048488237E-16, -4.373993382621220594E-17 ) ) ;
#10322 = EDGE_LOOP ( 'NONE', ( #12485, #5372, #25307, #14144 ) ) ;
#10323 = CARTESIAN_POINT ( 'NONE',  ( 2.063896406836605024, -46.16709813092717241, 137.7380992975101037 ) ) ;
#10324 = CARTESIAN_POINT ( 'NONE',  ( 109.1589550718175161, -0.007132058561966966165, 0.002553077953681008247 ) ) ;
#10325 = CARTESIAN_POINT ( 'NONE',  ( 26.28373643307440588, 125.5716026420343212, 22.43832507403690713 ) ) ;
#10326 = ORIENTED_EDGE ( 'NONE', *, *, #25831, .F. ) ;
#10327 = ORIENTED_EDGE ( 'NONE', *, *, #23843, .T. ) ;
#10328 = CARTESIAN_POINT ( 'NONE',  ( 1.832998868059858122, -29.64765804469970334, -142.0492247521725631 ) ) ;
#10329 = ORIENTED_EDGE ( 'NONE', *, *, #18214, .F. ) ;
#10330 = VERTEX_POINT ( 'NONE', #27349 ) ;
#10331 = EDGE_CURVE ( 'NONE', #8671, #14673, #24261, .T. ) ;
#10332 = CARTESIAN_POINT ( 'NONE',  ( 32.73300124599734318, 89.94078864464067635, 75.82012867748514395 ) ) ;
#10333 = ORIENTED_EDGE ( 'NONE', *, *, #16970, .T. ) ;
#10334 = EDGE_CURVE ( 'NONE', #7372, #4882, #26276, .T. ) ;
#10335 = CARTESIAN_POINT ( 'NONE',  ( -20.20612092514784663, 8.058517256681097862, -28.48192215759668855 ) ) ;
#10336 = CARTESIAN_POINT ( 'NONE',  ( 25.69398547355839568, 112.3990349503585264, 11.06723946918797097 ) ) ;
#10337 = CARTESIAN_POINT ( 'NONE',  ( 1.833206308920102057, -59.70089323729826702, 132.2594750499823704 ) ) ;
#10338 = DIRECTION ( 'NONE',  ( 0.7563875759206388771, 0.5078650950445714463, 0.4122509917856694850 ) ) ;
#10339 = CARTESIAN_POINT ( 'NONE',  ( 25.64700659047694842, 83.75695331063735694, 75.72132282458898089 ) ) ;
#10340 = CARTESIAN_POINT ( 'NONE',  ( 109.1587776205901861, -0.007280006032835099547, 0.0008489206734501343870 ) ) ;
#10341 = CYLINDRICAL_SURFACE ( 'NONE', #461, 12.50000000000000000 ) ;
#10342 = CARTESIAN_POINT ( 'NONE',  ( -25.21435515916043002, 34.05351380035335040, -6.169479169075572145 ) ) ;
#10344 = CARTESIAN_POINT ( 'NONE',  ( -1.045287976400379737, 44.00138577190644185, -12.68782741917337198 ) ) ;
#10343 = CARTESIAN_POINT ( 'NONE',  ( -8.786685647604885574, 6.096987947571466530E-17, -1.524246986892866633E-17 ) ) ;
#10345 = CARTESIAN_POINT ( 'NONE',  ( -1.058197053496163109, 28.32422455455077781, -36.00048521498961662 ) ) ;
#10346 = ORIENTED_EDGE ( 'NONE', *, *, #5650, .F. ) ;
#10347 = ORIENTED_EDGE ( 'NONE', *, *, #232, .F. ) ;
#10348 = CARTESIAN_POINT ( 'NONE',  ( -7.711401346138401003, -52.11446537925908018, 6.030154970217441956 ) ) ;
#10349 = CARTESIAN_POINT ( 'NONE',  ( -15.02187109954782507, -32.04062513125090561, 33.49412687891607021 ) ) ;
#10351 = CARTESIAN_POINT ( 'NONE',  ( 1.894214914920951287, 45.75988301372644429, 137.7482714433625972 ) ) ;
#10350 = CARTESIAN_POINT ( 'NONE',  ( 13.36082413113061307, -25.56125765253342763, -150.7747251079864839 ) ) ;
#10352 = CARTESIAN_POINT ( 'NONE',  ( 1.833206310202334821, 132.8652722326998514, 58.34025049824994369 ) ) ;
#10353 = CARTESIAN_POINT ( 'NONE',  ( 16.05277956358211000, -10.32496049470181454, 142.9335921074871294 ) ) ;
#10354 = ORIENTED_EDGE ( 'NONE', *, *, #12566, .T. ) ;
#10355 = CARTESIAN_POINT ( 'NONE',  ( -55.24340739397742084, 0.009386184976286932047, 0.003826481709803695053 ) ) ;
#10356 = DIRECTION ( 'NONE',  ( 5.541455922705464902E-20, -5.223019709708320524E-21, 1.000000000000000000 ) ) ;
#10357 = ORIENTED_EDGE ( 'NONE', *, *, #428, .T. ) ;
#10358 = CARTESIAN_POINT ( 'NONE',  ( -55.24198130335446422, -0.004276389980775889554, -0.008252882783650218948 ) ) ;
#10359 = CARTESIAN_POINT ( 'NONE',  ( 1.832998868059890096, 85.72499093308253748, -117.0819875546687143 ) ) ;
#10360 = CARTESIAN_POINT ( 'NONE',  ( 10.93730112725972781, -92.80059208661754155, 119.3442956573269100 ) ) ;
#10361 = DIRECTION ( 'NONE',  ( 0.000000000000000000, 0.000000000000000000, -1.000000000000000000 ) ) ;
#10362 = DIRECTION ( 'NONE',  ( 0.5914120900931444380, -0.7870418015781046606, -0.1754905759872871784 ) ) ;
#10363 = ORIENTED_EDGE ( 'NONE', *, *, #23282, .F. ) ;
#10364 = CARTESIAN_POINT ( 'NONE',  ( -1.019300379054419725, -28.53917295602924042, -35.83762006677390133 ) ) ;
#10365 = CARTESIAN_POINT ( 'NONE',  ( 2.108985857320890389, -137.7807691131291108, 46.11505917359396278 ) ) ;
#10366 = EDGE_CURVE ( 'NONE', #23109, #18351, #7953, .T. ) ;
#10367 =( BOUNDED_SURFACE ( )  B_SPLINE_SURFACE ( 3, 1, ( 
 ( #3439, #18694 ),
 ( #19122, #12218 ),
 ( #8191, #20983 ),
 ( #3716, #1270 ) ),
 .UNSPECIFIED., .F., .F., .F. ) 
 B_SPLINE_SURFACE_WITH_KNOTS ( ( 4, 4 ),
 ( 2, 2 ),
 ( 0.000000000000000000, 1.000000000000000000 ),
 ( 0.000000000000000000, 1.000000000000000000 ),
 .UNSPECIFIED. ) 
 GEOMETRIC_REPRESENTATION_ITEM ( )  RATIONAL_B_SPLINE_SURFACE ( (
 ( 1.000000000000000000, 1.000000000000000000),
 ( 0.9956975270656955868, 0.8568959468854907557),
 ( 0.9956975270656955868, 0.8568959468854907557),
 ( 1.000000000000000000, 1.000000000000000000) ) ) 
 REPRESENTATION_ITEM ( '' )  SURFACE ( )  );
#10368 = ORIENTED_EDGE ( 'NONE', *, *, #28417, .F. ) ;
#10369 = FACE_OUTER_BOUND ( 'NONE', #11231, .T. ) ;
#10370 = ADVANCED_FACE ( 'NONE', ( #16716 ), #21, .T. ) ;
#10371 = EDGE_CURVE ( 'NONE', #17023, #27443, #18581, .T. ) ;
#10373 = B_SPLINE_CURVE_WITH_KNOTS ( 'NONE', 3,
 ( #8271, #1771, #17035, #25832, #6390, #1638, #26101, #16907 ),
 .UNSPECIFIED., .F., .F.,
 ( 4, 2, 2, 4 ),
 ( 0.000000000000000000, 0.0002429592666046734805, 0.0004859185332093469609, 0.0009718370664186885008 ),
 .UNSPECIFIED. ) ;
#10372 = DIRECTION ( 'NONE',  ( 0.000000000000000000, 0.000000000000000000, 1.000000000000000000 ) ) ;
#10374 = B_SPLINE_CURVE_WITH_KNOTS ( 'NONE', 3,
 ( #18031, #9847, #5371, #27089, #18617, #24827, #16167, #7398, #22668, #14136 ),
 .UNSPECIFIED., .F., .F.,
 ( 4, 3, 3, 4 ),
 ( 1.962615573354718958E-17, 0.0002669560319015674304, 0.0005492286108966131560, 0.0008315040496093250568 ),
 .UNSPECIFIED. ) ;
#10375 = CARTESIAN_POINT ( 'NONE',  ( 109.1721716018069515, -0.01629455849719226371, 0.005082060336465219624 ) ) ;
#10376 = B_SPLINE_CURVE_WITH_KNOTS ( 'NONE', 3,
 ( #15541, #17990, #11105, #9088, #26776, #13246, #26629, #2600 ),
 .UNSPECIFIED., .F., .F.,
 ( 4, 2, 2, 4 ),
 ( 2.214340075454938295E-16, 0.002761568181852865067, 0.005523136363705508090, 0.01104627272741079587 ),
 .UNSPECIFIED. ) ;
#10377 =( LENGTH_UNIT ( ) NAMED_UNIT ( * ) SI_UNIT ( .MILLI., .METRE. ) );
#10378 = FACE_OUTER_BOUND ( 'NONE', #26925, .T. ) ;
#10379 = EDGE_CURVE ( 'NONE', #1405, #18334, #2948, .T. ) ;
#10380 = CARTESIAN_POINT ( 'NONE',  ( 26.11404676487259024, 12.95861723607453619, 112.4785329405482628 ) ) ;
#10381 = CARTESIAN_POINT ( 'NONE',  ( 25.64681081121879203, -75.24277141833549365, 84.18689316040023130 ) ) ;
#10382 = CARTESIAN_POINT ( 'NONE',  ( 2.263178607246690621, -57.85473702627204773, 133.3897506477020443 ) ) ;
#10383 = ORIENTED_EDGE ( 'NONE', *, *, #13874, .T. ) ;
#10384 = ORIENTED_EDGE ( 'NONE', *, *, #11863, .T. ) ;
#10385 = FACE_OUTER_BOUND ( 'NONE', #18563, .T. ) ;
#10386 = CARTESIAN_POINT ( 'NONE',  ( 30.58324630866340854, -67.85993782330834279, 100.1119227962718128 ) ) ;
#10387 = CARTESIAN_POINT ( 'NONE',  ( 25.64703792032469920, -84.00887408969001058, -75.44170528134974063 ) ) ;
#10388 = DIRECTION ( 'NONE',  ( 1.000000000000000000, -6.938893903907226837E-18, 1.734723475976806709E-18 ) ) ;
#10389 = CARTESIAN_POINT ( 'NONE',  ( -20.21097721650787449, 24.14932365326977148, 17.13687097598110398 ) ) ;
#10390 = CARTESIAN_POINT ( 'NONE',  ( 24.01988960052064215, -130.7041393974935204, 9.440825210282998370 ) ) ;
#10391 = ORIENTED_EDGE ( 'NONE', *, *, #3806, .T. ) ;
#10392 = CARTESIAN_POINT ( 'NONE',  ( 32.73300124599737160, -117.3295799645428872, -8.473903470907334423 ) ) ;
#10393 = CARTESIAN_POINT ( 'NONE',  ( -1.323830074806772616, -25.17121255494502563, -38.58891736138520656 ) ) ;
#10394 = CARTESIAN_POINT ( 'NONE',  ( 109.1586900883932856, -0.002109621908824195913, -0.006819617742892433374 ) ) ;
#10395 = EDGE_CURVE ( 'NONE', #16104, #22997, #14955, .T. ) ;
#10396 = ORIENTED_EDGE ( 'NONE', *, *, #15493, .T. ) ;
#10397 = CARTESIAN_POINT ( 'NONE',  ( 25.64681081121880624, -46.30456157731397582, 102.9795863647027119 ) ) ;
#10398 = CARTESIAN_POINT ( 'NONE',  ( 25.64703792032469920, -11.95040607427908341, -112.2770217641849371 ) ) ;
#10399 = ORIENTED_EDGE ( 'NONE', *, *, #27802, .F. ) ;
#10400 = EDGE_CURVE ( 'NONE', #24273, #23707, #27294, .T. ) ;
#10401 = ADVANCED_FACE ( 'NONE', ( #8921, #4023 ), #17258, .F. ) ;
#10402 = ORIENTED_EDGE ( 'NONE', *, *, #12451, .T. ) ;
#10403 = EDGE_LOOP ( 'NONE', ( #10197, #262, #9632, #21130 ) ) ;
#10404 =( BOUNDED_SURFACE ( )  B_SPLINE_SURFACE ( 3, 1, ( 
 ( #7188, #16673 ),
 ( #14499, #21110 ),
 ( #27307, #5879 ),
 ( #14067, #3426 ) ),
 .UNSPECIFIED., .F., .F., .F. ) 
 B_SPLINE_SURFACE_WITH_KNOTS ( ( 4, 4 ),
 ( 2, 2 ),
 ( 0.000000000000000000, 1.000000000000000000 ),
 ( 0.000000000000000000, 1.000000000000000000 ),
 .UNSPECIFIED. ) 
 GEOMETRIC_REPRESENTATION_ITEM ( )  RATIONAL_B_SPLINE_SURFACE ( (
 ( 1.000000000000000000, 1.000000000000000000),
 ( 0.9960225298536222738, 0.9999952330161893110),
 ( 0.9960225298536222738, 0.9999952330161893110),
 ( 1.000000000000000000, 1.000000000000000000) ) ) 
 REPRESENTATION_ITEM ( '' )  SURFACE ( )  );
#10405 = FACE_OUTER_BOUND ( 'NONE', #25741, .T. ) ;
#10406 = LINE ( 'NONE', #23227, #11980 ) ;
#10407 = CARTESIAN_POINT ( 'NONE',  ( 1.833838850093440165, 30.17001281793556089, -141.9387673160883026 ) ) ;
#10408 = CARTESIAN_POINT ( 'NONE',  ( 13.84597867724973064, 124.5889929031786920, 77.45414123936249950 ) ) ;
#10409 = ORIENTED_EDGE ( 'NONE', *, *, #11684, .F. ) ;
#10410 = CARTESIAN_POINT ( 'NONE',  ( 1.833838850093439943, -59.02146106674994996, -132.5643635152040929 ) ) ;
#10411 = B_SPLINE_CURVE_WITH_KNOTS ( 'NONE', 3,
 ( #19161, #8230, #12672, #23648, #16872, #8374, #1732, #27933 ),
 .UNSPECIFIED., .F., .F.,
 ( 4, 2, 2, 4 ),
 ( 3.469446951953614189E-18, 0.0002429592666046782238, 0.0004859185332093529782, 0.0009718370664186902355 ),
 .UNSPECIFIED. ) ;
#10412 = CARTESIAN_POINT ( 'NONE',  ( 10.93730112725932635, 0.000000000000000000, 0.000000000000000000 ) ) ;
#10413 = CARTESIAN_POINT ( 'NONE',  ( -1.044556982611268614, 45.76404732357880079, -1.643392503292874895 ) ) ;
#10414 = CARTESIAN_POINT ( 'NONE',  ( -12.82751273423880001, 21.21958768041857724, 44.03362901246980243 ) ) ;
#10415 = CARTESIAN_POINT ( 'NONE',  ( -23.77929240705205771, 6.464423883190382192, -35.68044874544699496 ) ) ;
#10416 = CARTESIAN_POINT ( 'NONE',  ( 6.224689322667647851, 48.18553814190031659, 139.9988794244333690 ) ) ;
#10417 = CARTESIAN_POINT ( 'NONE',  ( 109.1586900883932856, -0.002301750759599823989, 0.006757191295060836073 ) ) ;
#10418 = CARTESIAN_POINT ( 'NONE',  ( 9.884929003653626367, 42.50195158091224101, -144.4113244745767588 ) ) ;
#10419 = FACE_OUTER_BOUND ( 'NONE', #17370, .T. ) ;
#10420 = CARTESIAN_POINT ( 'NONE',  ( -7.711401346138400115, -25.75361633141456608, 45.70592430511747040 ) ) ;
#10421 = EDGE_CURVE ( 'NONE', #16227, #17233, #15599, .T. ) ;
#10422 = ORIENTED_EDGE ( 'NONE', *, *, #6928, .T. ) ;
#10423 = ADVANCED_FACE ( 'NONE', ( #8627 ), #21181, .F. ) ;
#10424 = ORIENTED_EDGE ( 'NONE', *, *, #27698, .T. ) ;
#10425 = CARTESIAN_POINT ( 'NONE',  ( 109.1586059443104944, 0.007001002073869785382, -0.001014167950289997146 ) ) ;
#10426 = CARTESIAN_POINT ( 'NONE',  ( -22.23342874802667879, -29.33662284748868387, -11.82490389046302859 ) ) ;
#10427 = VERTEX_POINT ( 'NONE', #28461 ) ;
#10428 = ORIENTED_EDGE ( 'NONE', *, *, #24664, .T. ) ;
#10429 = VERTEX_POINT ( 'NONE', #15371 ) ;
#10430 = CARTESIAN_POINT ( 'NONE',  ( 19.66333377628706458, 88.78556591841305590, 105.3186440504699561 ) ) ;
#10431 = CARTESIAN_POINT ( 'NONE',  ( -24.53237795827023859, 6.738475012720130941, -33.25734978085264260 ) ) ;
#10432 = EDGE_CURVE ( 'NONE', #24805, #19774, #6619, .T. ) ;
#10433 =( BOUNDED_SURFACE ( )  B_SPLINE_SURFACE ( 3, 1, ( 
 ( #10536, #16879 ),
 ( #7974, #14417 ),
 ( #21325, #25378 ),
 ( #21179, #14261 ) ),
 .UNSPECIFIED., .F., .F., .F. ) 
 B_SPLINE_SURFACE_WITH_KNOTS ( ( 4, 4 ),
 ( 2, 2 ),
 ( 0.000000000000000000, 1.000000000000000000 ),
 ( 0.000000000000000000, 1.000000000000000000 ),
 .UNSPECIFIED. ) 
 GEOMETRIC_REPRESENTATION_ITEM ( )  RATIONAL_B_SPLINE_SURFACE ( (
 ( 1.000000000000000000, 1.000000000000000000),
 ( 0.9960225298536222738, 0.9999952330161893110),
 ( 0.9960225298536222738, 0.9999952330161893110),
 ( 1.000000000000000000, 1.000000000000000000) ) ) 
 REPRESENTATION_ITEM ( '' )  SURFACE ( )  );
#10434 = CARTESIAN_POINT ( 'NONE',  ( 109.1592201516379674, -0.005485778713193788063, 0.005631912476305676526 ) ) ;
#10435 = CARTESIAN_POINT ( 'NONE',  ( 1.833485406944043827, -14.63699153649458040, 144.3694338680884641 ) ) ;
#10436 = CARTESIAN_POINT ( 'NONE',  ( 2.433796855181233454, -86.69855925933894980, -116.8607839509065371 ) ) ;
#10437 = CARTESIAN_POINT ( 'NONE',  ( -1.239374126674604337, 44.48112152129347407, -11.92219841463844432 ) ) ;
#10438 = CARTESIAN_POINT ( 'NONE',  ( 25.87036335909426654, -112.5399073133628463, -10.83311869338186462 ) ) ;
#10439 = ADVANCED_FACE ( 'NONE', ( #10515 ), #22100, .F. ) ;
#10440 = EDGE_LOOP ( 'NONE', ( #17727, #11211, #20460, #12474 ) ) ;
#10441 = VERTEX_POINT ( 'NONE', #1854 ) ;
#10442 = ADVANCED_FACE ( 'NONE', ( #19423 ), #22281, .F. ) ;
#10444 = CARTESIAN_POINT ( 'NONE',  ( 2.430230287190592531, -125.2872625092167596, 74.01081053031055035 ) ) ;
#10443 = DIRECTION ( 'NONE',  ( 1.000000000000000000, -6.938893903907226837E-18, 1.734723475976806709E-18 ) ) ;
#10445 = CARTESIAN_POINT ( 'NONE',  ( 5.340103579038270709, 96.93942141937453982, -111.1041836885938068 ) ) ;
#10446 = CARTESIAN_POINT ( 'NONE',  ( 1.832998868059858122, -117.0819875546689417, -85.72499093308222484 ) ) ;
#10447 = CARTESIAN_POINT ( 'NONE',  ( 25.70243777736192570, 112.4037002646849146, -11.07690056740750073 ) ) ;
#10448 = ORIENTED_EDGE ( 'NONE', *, *, #9934, .F. ) ;
#10449 = LINE ( 'NONE', #19080, #20748 ) ;
#10450 = ADVANCED_FACE ( 'NONE', ( #15645 ), #2777, .T. ) ;
#10451 = CARTESIAN_POINT ( 'NONE',  ( -1.619063947482197729, -29.22875152547781852, -35.99532424477369830 ) ) ;
#10452 = CARTESIAN_POINT ( 'NONE',  ( 2.063896406836605024, 46.16709813092805348, -137.7380992975097911 ) ) ;
#10453 = ORIENTED_EDGE ( 'NONE', *, *, #16319, .T. ) ;
#10454 = VERTEX_POINT ( 'NONE', #20553 ) ;
#10455 = ADVANCED_FACE ( 'NONE', ( #27165 ), #14375, .F. ) ;
#10456 = VERTEX_POINT ( 'NONE', #22297 ) ;
#10457 = VERTEX_POINT ( 'NONE', #15809 ) ;
#10458 = B_SPLINE_CURVE_WITH_KNOTS ( 'NONE', 3,
 ( #17544, #10808, #6485, #11219, #4315, #8777, #17401, #2006, #13092, #19993 ),
 .UNSPECIFIED., .F., .F.,
 ( 4, 2, 2, 2, 4 ),
 ( 1.301042606982605321E-18, 0.0003346267210630944101, 0.0006692534421261875192, 0.001003880163189280628, 0.001338506884252373737 ),
 .UNSPECIFIED. ) ;
#10459 = CARTESIAN_POINT ( 'NONE',  ( 6.224689322667647851, -18.02516478984043857, -146.9579047224771386 ) ) ;
#10460 = VERTEX_POINT ( 'NONE', #4729 ) ;
#10461 = CARTESIAN_POINT ( 'NONE',  ( 1.832998868059890096, 137.8420662456170191, 45.34898734666091968 ) ) ;
#10462 = CONTEXT_DEPENDENT_SHAPE_REPRESENTATION ( #2555, #20505 ) ;
#10463 = CARTESIAN_POINT ( 'NONE',  ( 26.11404676487256893, -55.62948129436175293, -98.61392875273419634 ) ) ;
#10464 = CARTESIAN_POINT ( 'NONE',  ( 109.1778270068192853, -0.003465086990435428584, 0.008646067828082875176 ) ) ;
#10465 = CARTESIAN_POINT ( 'NONE',  ( 2.263178607246682628, 138.7064943909645649, 43.59477707254079348 ) ) ;
#10466 = CARTESIAN_POINT ( 'NONE',  ( -1.049819825607589685, 13.66706894614437928, -43.71263398674757639 ) ) ;
#10467 = CARTESIAN_POINT ( 'NONE',  ( 13.84597867724978215, -10.56985607909703617, -146.3210145202069441 ) ) ;
#10468 = CARTESIAN_POINT ( 'NONE',  ( 25.87036335909428075, -103.6841944152903920, -45.07965203035023904 ) ) ;
#10470 = CARTESIAN_POINT ( 'NONE',  ( 25.81918753295377300, -10.88546493098934320, 112.5005889664128489 ) ) ;
#10469 = CARTESIAN_POINT ( 'NONE',  ( -20.20700224038492721, -28.44216453106542986, -8.199606986804219844 ) ) ;
#10471 = CARTESIAN_POINT ( 'NONE',  ( 10.93730112725971892, -10.89264110825104837, 150.7858122213660863 ) ) ;
#10472 = ORIENTED_EDGE ( 'NONE', *, *, #7006, .T. ) ;
#10473 = ORIENTED_EDGE ( 'NONE', *, *, #25597, .T. ) ;
#10474 = LINE ( 'NONE', #1124, #989 ) ;
#10475 = CARTESIAN_POINT ( 'NONE',  ( 1.832998868059858122, -85.72499093308022111, -117.0819875546704054 ) ) ;
#10476 = EDGE_CURVE ( 'NONE', #16572, #194, #5711, .T. ) ;
#10477 = CARTESIAN_POINT ( 'NONE',  ( 109.1624594426973118, 0.01591840958353239743, 0.001206615835669516733 ) ) ;
#10478 = CARTESIAN_POINT ( 'NONE',  ( 25.69398547355840634, -76.12333255527457254, -83.43419615433070646 ) ) ;
#10479 = CARTESIAN_POINT ( 'NONE',  ( 2.433796855181233454, 98.43889364293860922, 107.1581411821788947 ) ) ;
#10480 = CARTESIAN_POINT ( 'NONE',  ( -25.21435515916043713, -15.02493970636168896, -31.17620025257581062 ) ) ;
#10481 = CARTESIAN_POINT ( 'NONE',  ( -1.044557008772714068, -44.03203053429562885, 12.57891310333395118 ) ) ;
#10482 = VERTEX_POINT ( 'NONE', #11482 ) ;
#10483 = CARTESIAN_POINT ( 'NONE',  ( -20.57838717382308147, 1.611677988432778319, 29.92853265176829325 ) ) ;
#10484 = DIRECTION ( 'NONE',  ( -1.000000000000000000, -0.000000000000000000, -0.000000000000000000 ) ) ;
#10485 = EDGE_CURVE ( 'NONE', #2734, #26638, #533, .T. ) ;
#10486 = CARTESIAN_POINT ( 'NONE',  ( -4.473127245936431073, -47.80062405537792358, 12.17046501147566318 ) ) ;
#10487 = CARTESIAN_POINT ( 'NONE',  ( -15.02187109954783040, -21.95370994985601953, -40.82269973458228662 ) ) ;
#10488 =( REPRESENTATION_RELATIONSHIP ('NONE','NONE', #15430, #22271 ) REPRESENTATION_RELATIONSHIP_WITH_TRANSFORMATION ( #25721 )SHAPE_REPRESENTATION_RELATIONSHIP( ) );
#10489 = CARTESIAN_POINT ( 'NONE',  ( -55.24390624410018802, -0.009374879212966679906, -0.004572280736703028189 ) ) ;
#10490 = EDGE_LOOP ( 'NONE', ( #23190, #233, #3857, #15304 ) ) ;
#10491 = CARTESIAN_POINT ( 'NONE',  ( 16.75465622695655199, -34.09043808962508137, 138.0797984721904754 ) ) ;
#10492 = CARTESIAN_POINT ( 'NONE',  ( -1.619063947482197729, 44.80407745103800465, 11.94059994246113021 ) ) ;
#10493 = ORIENTED_EDGE ( 'NONE', *, *, #12803, .F. ) ;
#10494 = CARTESIAN_POINT ( 'NONE',  ( 1.833206310202347034, -29.44113265021029591, 142.0914673790819620 ) ) ;
#10495 = CARTESIAN_POINT ( 'NONE',  ( -1.113548883309550153, -35.91246368318222437, -28.52482525634933097 ) ) ;
#10496 = B_SPLINE_CURVE_WITH_KNOTS ( 'NONE', 3,
 ( #22689, #26968, #13452, #20501, #26688, #18052, #7275 ),
 .UNSPECIFIED., .F., .F.,
 ( 4, 3, 4 ),
 ( 0.000000000000000000, 0.02398743853561398701, 0.04000277880656223639 ),
 .UNSPECIFIED. ) ;
#10497 = CARTESIAN_POINT ( 'NONE',  ( 25.64681081121879203, 97.99105938547923245, 56.09509703373377931 ) ) ;
#10498 = CARTESIAN_POINT ( 'NONE',  ( -1.050230347699842692, 5.964912479342754695E-15, -45.79907861674080749 ) ) ;
#10499 = CARTESIAN_POINT ( 'NONE',  ( -1.045287976400351981, 36.12803364096590997, -28.14015102489844011 ) ) ;
#10500 = CARTESIAN_POINT ( 'NONE',  ( 5.340103579038080639, 128.8311297206841459, 71.72120379026067383 ) ) ;
#10501 = CARTESIAN_POINT ( 'NONE',  ( 16.05277956358202118, 67.56865019684023821, -126.3767940428294736 ) ) ;
#10502 = CARTESIAN_POINT ( 'NONE',  ( 109.1592201516379674, -0.006649399203953433417, 0.004194960840990133617 ) ) ;
#10503 = B_SPLINE_CURVE_WITH_KNOTS ( 'NONE', 3,
 ( #19106, #19234, #28148, #16667 ),
 .UNSPECIFIED., .F., .F.,
 ( 4, 4 ),
 ( 1.895855152355442610E-16, 0.001982023823822949386 ),
 .UNSPECIFIED. ) ;
#10504 = CIRCLE ( 'NONE', #371, 151.1787379149930359 ) ;
#10505 = CARTESIAN_POINT ( 'NONE',  ( 1.833838850093452821, -59.02145475724738333, 132.5643663243755839 ) ) ;
#10506 = CARTESIAN_POINT ( 'NONE',  ( 1.832998868059858122, 132.3466930259793628, 59.50898020732557114 ) ) ;
#10507 = CARTESIAN_POINT ( 'NONE',  ( 55.49584447822657296, 48.34726110740061245, -54.09506550945575754 ) ) ;
#10508 = CARTESIAN_POINT ( 'NONE',  ( -1.044556982611270612, 28.22896456560720679, 36.05793013899066324 ) ) ;
#10509 = EDGE_LOOP ( 'NONE', ( #24887, #25869, #15995, #24904 ) ) ;
#10510 = B_SPLINE_CURVE_WITH_KNOTS ( 'NONE', 3,
 ( #11988, #18302, #2931, #20908, #9413, #1197 ),
 .UNSPECIFIED., .F., .F.,
 ( 4, 2, 4 ),
 ( 4.114075111014854645E-16, 0.003576372551511222079, 0.007152745103022032161 ),
 .UNSPECIFIED. ) ;
#10511 = ORIENTED_EDGE ( 'NONE', *, *, #23726, .T. ) ;
#10512 = CARTESIAN_POINT ( 'NONE',  ( -8.786685647604896232, 52.67761315067299677, 9.545808661480061019 ) ) ;
#10513 = CARTESIAN_POINT ( 'NONE',  ( 25.64707127832796019, 1.378041109049876443E-14, 112.9112343549835487 ) ) ;
#10514 = EDGE_CURVE ( 'NONE', #19079, #16076, #7859, .T. ) ;
#10515 = FACE_OUTER_BOUND ( 'NONE', #8749, .T. ) ;
#10516 = CARTESIAN_POINT ( 'NONE',  ( 26.11404676487259024, -83.38016054979834735, 76.59696442953165274 ) ) ;
#10517 = CARTESIAN_POINT ( 'NONE',  ( 109.1586900883932856, -0.001385221016527508594, 0.007002774699553633575 ) ) ;
#10518 = ORIENTED_EDGE ( 'NONE', *, *, #13864, .F. ) ;
#10519 = CARTESIAN_POINT ( 'NONE',  ( 8.186469829614219762, 57.56191610809376868, 137.8131829164336182 ) ) ;
#10520 = CARTESIAN_POINT ( 'NONE',  ( -55.24271866751342941, 0.008433070970614256479, -0.004365563123935527895 ) ) ;
#10521 = CARTESIAN_POINT ( 'NONE',  ( 109.1624594426973118, 0.01595733256932007488, -0.0004639210235603172228 ) ) ;
#10522 = EDGE_CURVE ( 'NONE', #4222, #20894, #17349, .T. ) ;
#10523 = EDGE_CURVE ( 'NONE', #604, #24791, #21138, .T. ) ;
#10524 = B_SPLINE_CURVE_WITH_KNOTS ( 'NONE', 3,
 ( #21803, #6697, #19350, #27988, #28398, #21939, #8429 ),
 .UNSPECIFIED., .F., .F.,
 ( 4, 3, 4 ),
 ( 0.000000000000000000, 0.02398743853561394884, 0.04000277880656219476 ),
 .UNSPECIFIED. ) ;
#10525 = CARTESIAN_POINT ( 'NONE',  ( -8.786685647604890903, -23.24040270374424466, -48.22796981442760256 ) ) ;
#10526 =( BOUNDED_SURFACE ( )  B_SPLINE_SURFACE ( 3, 1, ( 
 ( #1146, #13799 ),
 ( #25333, #5608 ),
 ( #14372, #9636 ),
 ( #22757, #27028 ) ),
 .UNSPECIFIED., .F., .F., .F. ) 
 B_SPLINE_SURFACE_WITH_KNOTS ( ( 4, 4 ),
 ( 2, 2 ),
 ( 0.000000000000000000, 1.000000000000000000 ),
 ( 0.000000000000000000, 1.000000000000000000 ),
 .UNSPECIFIED. ) 
 GEOMETRIC_REPRESENTATION_ITEM ( )  RATIONAL_B_SPLINE_SURFACE ( (
 ( 1.000000000000000000, 1.000000000000000000),
 ( 0.7789835883360576307, 0.9689951854195403280),
 ( 0.7789835883360576307, 0.9689951854195403280),
 ( 1.000000000000000000, 1.000000000000000000) ) ) 
 REPRESENTATION_ITEM ( '' )  SURFACE ( )  );
#10527 = VERTEX_POINT ( 'NONE', #24754 ) ;
#10528 = CARTESIAN_POINT ( 'NONE',  ( 25.64692232868534560, -112.3263170481596660, -11.47740546588750199 ) ) ;
#10529 = CARTESIAN_POINT ( 'NONE',  ( 10.93730112725932635, 0.000000000000000000, 0.000000000000000000 ) ) ;
#10530 = ORIENTED_EDGE ( 'NONE', *, *, #10601, .T. ) ;
#10531 = AXIS2_PLACEMENT_3D ( 'NONE', #5222, #3352, #11555 ) ;
#10532 = ORIENTED_EDGE ( 'NONE', *, *, #1189, .F. ) ;
#10533 = VECTOR ( 'NONE', #12040, 1000.000000000000000 ) ;
#10534 = ORIENTED_EDGE ( 'NONE', *, *, #7071, .T. ) ;
#10535 = CARTESIAN_POINT ( 'NONE',  ( 109.1778270068192853, 0.001322180554006313971, -0.009220257877172538530 ) ) ;
#10536 = CARTESIAN_POINT ( 'NONE',  ( 109.1586900883932856, -0.001385221016527508594, 0.007002774699553633575 ) ) ;
#10537 = CARTESIAN_POINT ( 'NONE',  ( 1.833485406944071361, 29.64752363041738548, -142.0485807715643034 ) ) ;
#10538 = EDGE_CURVE ( 'NONE', #2946, #8194, #694, .T. ) ;
#10539 = CARTESIAN_POINT ( 'NONE',  ( 28.37644542392823865, 105.5967537682344926, 65.64862111872109551 ) ) ;
#10540 = ORIENTED_EDGE ( 'NONE', *, *, #4844, .F. ) ;
#10541 = CARTESIAN_POINT ( 'NONE',  ( -1.619063947482197729, 46.30105812165548684, 2.489035965910320503 ) ) ;
#10542 = DIRECTION ( 'NONE',  ( -0.7071067818211355105, 4.902845705138443504E-18, 0.7071067805519596350 ) ) ;
#10543 = CARTESIAN_POINT ( 'NONE',  ( 109.1586900883932856, -0.006960773163856042410, -0.001582822706024228452 ) ) ;
#10544 = EDGE_CURVE ( 'NONE', #6343, #5142, #22160, .T. ) ;
#10545 = CARTESIAN_POINT ( 'NONE',  ( -1.048996300304487095, 45.79145529752471333, -0.7649764263853394697 ) ) ;
#10546 = CARTESIAN_POINT ( 'NONE',  ( -8.786685647604931759, 47.14957014837394667, 25.35688121747446999 ) ) ;
#10547 = CARTESIAN_POINT ( 'NONE',  ( 25.64708228042118776, -11.84161204513335619, 112.2886173090159048 ) ) ;
#10548 = CARTESIAN_POINT ( 'NONE',  ( 10.93730112725971715, -20.69552240458431314, 149.7554878793147282 ) ) ;
#10549 = CARTESIAN_POINT ( 'NONE',  ( 94.22246935314088034, 90.00000000000005684, 12.49999999999999467 ) ) ;
#10550 = VERTEX_POINT ( 'NONE', #2411 ) ;
#10551 =( BOUNDED_SURFACE ( )  B_SPLINE_SURFACE ( 3, 1, ( 
 ( #16344, #14173 ),
 ( #14321, #20944 ),
 ( #14468, #23141 ),
 ( #1650, #1231 ) ),
 .UNSPECIFIED., .F., .F., .F. ) 
 B_SPLINE_SURFACE_WITH_KNOTS ( ( 4, 4 ),
 ( 2, 2 ),
 ( 0.000000000000000000, 1.000000000000000000 ),
 ( 0.000000000000000000, 1.000000000000000000 ),
 .UNSPECIFIED. ) 
 GEOMETRIC_REPRESENTATION_ITEM ( )  RATIONAL_B_SPLINE_SURFACE ( (
 ( 1.000000000000000000, 1.000000000000000000),
 ( 0.9593753223639863714, 0.9995975284513187731),
 ( 0.9593753223639863714, 0.9995975284513187731),
 ( 1.000000000000000000, 1.000000000000000000) ) ) 
 REPRESENTATION_ITEM ( '' )  SURFACE ( )  );
#10552 = ORIENTED_EDGE ( 'NONE', *, *, #4933, .T. ) ;
#10553 = CARTESIAN_POINT ( 'NONE',  ( 25.64681081121880624, -23.88203588908001507, -110.3564950173084185 ) ) ;
#10554 = VERTEX_POINT ( 'NONE', #20689 ) ;
#10555 = VERTEX_POINT ( 'NONE', #11922 ) ;
#10556 = ORIENTED_EDGE ( 'NONE', *, *, #21882, .F. ) ;
#10557 = VERTEX_POINT ( 'NONE', #3288 ) ;
#10558 = DIRECTION ( 'NONE',  ( -1.000000000000000000, 6.938893903907227607E-18, -1.734723475976806902E-18 ) ) ;
#10559 = CARTESIAN_POINT ( 'NONE',  ( 10.93730112725970294, 65.95960219663110990, 136.0306644680985642 ) ) ;
#10560 = CARTESIAN_POINT ( 'NONE',  ( -24.53239521893645048, 29.54733954334105661, -16.68574937150984638 ) ) ;
#10561 = CARTESIAN_POINT ( 'NONE',  ( -20.47566338032525124, 16.24827550219824701, -25.06314818626695740 ) ) ;
#10562 = B_SPLINE_CURVE_WITH_KNOTS ( 'NONE', 3,
 ( #17597, #6258, #6683, #23965, #21926, #8416, #2184, #4221, #12849, #14880, #2331, #8685, #10993 ),
 .UNSPECIFIED., .F., .F.,
 ( 4, 3, 3, 3, 4 ),
 ( 1.551583845779545699E-17, 0.0007657099931970509123, 0.001531419946797920456, 0.002296279302920149930, 0.003061450627205759834 ),
 .UNSPECIFIED. ) ;
#10563 = EDGE_CURVE ( 'NONE', #3225, #10550, #10847, .T. ) ;
#10564 = CARTESIAN_POINT ( 'NONE',  ( 180.4657679828686980, -20.00000000000000000, 3.130582043300658722E-16 ) ) ;
#10565 = EDGE_CURVE ( 'NONE', #15445, #1356, #27665, .T. ) ;
#10566 = CARTESIAN_POINT ( 'NONE',  ( 1.832998868059858122, 117.0819875546695528, 85.72499093308138640 ) ) ;
#10567 = LINE ( 'NONE', #19201, #6527 ) ;
#10568 = ADVANCED_FACE ( 'NONE', ( #14640 ), #28145, .F. ) ;
#10569 = CARTESIAN_POINT ( 'NONE',  ( -55.24340739397742794, -0.005344433640973866861, 0.008612749836242647450 ) ) ;
#10570 = CARTESIAN_POINT ( 'NONE',  ( 6.224689322667647851, -134.1951906609243110, 62.55544044765201761 ) ) ;
#10571 = CARTESIAN_POINT ( 'NONE',  ( 10.93730112725991077, -79.81734490845832397, -128.3908183996600201 ) ) ;
#10572 = ORIENTED_EDGE ( 'NONE', *, *, #7071, .F. ) ;
#10573 = VERTEX_POINT ( 'NONE', #23306 ) ;
#10575 = CARTESIAN_POINT ( 'NONE',  ( -55.24198130335446422, 0.001391250620105636670, -0.009190321388309047670 ) ) ;
#10574 = CARTESIAN_POINT ( 'NONE',  ( 2.433796855181219243, -13.76554153471791864, 144.8571464219888583 ) ) ;
#10576 = CARTESIAN_POINT ( 'NONE',  ( -55.25297051322618813, 0.01306918787467630481, -0.007247191603131783282 ) ) ;
#10577 = CARTESIAN_POINT ( 'NONE',  ( 2.108985857320914370, 96.26411661813186527, -108.8271972979190423 ) ) ;
#10578 = ORIENTED_EDGE ( 'NONE', *, *, #18889, .T. ) ;
#10579 = CARTESIAN_POINT ( 'NONE',  ( 8.186469777911039358, 148.1306754055311501, -19.05650978729052270 ) ) ;
#10580 = CARTESIAN_POINT ( 'NONE',  ( -20.21097721712959583, -17.67178718142840665, 23.76068428613700334 ) ) ;
#10581 = CARTESIAN_POINT ( 'NONE',  ( -1.239374126674604337, -28.97829083655465254, -35.79060836339803586 ) ) ;
#10582 = ORIENTED_EDGE ( 'NONE', *, *, #3353, .T. ) ;
#10583 = VERTEX_POINT ( 'NONE', #21267 ) ;
#10584 = CARTESIAN_POINT ( 'NONE',  ( -1.031422197589716205, 15.60268798220638509, -43.06660437151315080 ) ) ;
#10585 = ORIENTED_EDGE ( 'NONE', *, *, #9752, .T. ) ;
#10586 = ORIENTED_EDGE ( 'NONE', *, *, #6932, .F. ) ;
#10587 =( BOUNDED_SURFACE ( )  B_SPLINE_SURFACE ( 3, 1, ( 
 ( #8870, #12605 ),
 ( #17209, #19228 ),
 ( #13166, #12880 ),
 ( #28003, #17629 ) ),
 .UNSPECIFIED., .F., .F., .F. ) 
 B_SPLINE_SURFACE_WITH_KNOTS ( ( 4, 4 ),
 ( 2, 2 ),
 ( 0.000000000000000000, 1.000000000000000000 ),
 ( 0.000000000000000000, 1.000000000000000000 ),
 .UNSPECIFIED. ) 
 GEOMETRIC_REPRESENTATION_ITEM ( )  RATIONAL_B_SPLINE_SURFACE ( (
 ( 1.000000000000000000, 1.000000000000000000),
 ( 0.7789835883360576307, 0.9689951854195403280),
 ( 0.7789835883360576307, 0.9689951854195403280),
 ( 1.000000000000000000, 1.000000000000000000) ) ) 
 REPRESENTATION_ITEM ( '' )  SURFACE ( )  );
#10588 = CARTESIAN_POINT ( 'NONE',  ( -8.786685647604894456, 37.00619870957989832, 38.68584556812258768 ) ) ;
#10589 = EDGE_CURVE ( 'NONE', #16457, #15104, #19400, .T. ) ;
#10590 = ORIENTED_EDGE ( 'NONE', *, *, #9535, .T. ) ;
#10591 = AXIS2_PLACEMENT_3D ( 'NONE', #14782, #2228, #17223 ) ;
#10592 = B_SPLINE_CURVE_WITH_KNOTS ( 'NONE', 3,
 ( #11442, #24269, #9570, #17898 ),
 .UNSPECIFIED., .F., .F.,
 ( 4, 4 ),
 ( 3.492272924721346237E-16, 0.01077107486149825148 ),
 .UNSPECIFIED. ) ;
#10593 = VECTOR ( 'NONE', #23851, 1000.000000000000114 ) ;
#10594 = CARTESIAN_POINT ( 'NONE',  ( 5.340103556456440081, -75.71042922800619124, 126.5279493230356280 ) ) ;
#10595 = AXIS2_PLACEMENT_3D ( 'NONE', #19399, #8475, #26027 ) ;
#10596 = EDGE_CURVE ( 'NONE', #8511, #21937, #24574, .T. ) ;
#10597 = CARTESIAN_POINT ( 'NONE',  ( 13.36082413113061307, 70.90215303572124128, 135.4964217943309563 ) ) ;
#10598 = CARTESIAN_POINT ( 'NONE',  ( 28.43349137099852442, 109.5743306972603932, 58.58376153369732720 ) ) ;
#10599 = CARTESIAN_POINT ( 'NONE',  ( -1.048996300304495310, 13.42280206896976757, -43.78665266739842110 ) ) ;
#10600 = CARTESIAN_POINT ( 'NONE',  ( 28.37644542392846603, -8.957364412599346792, -124.0168596762486715 ) ) ;
#10601 = EDGE_CURVE ( 'NONE', #4557, #13961, #3957, .T. ) ;
#10602 = CARTESIAN_POINT ( 'NONE',  ( -20.20700224038492721, 10.08426345511588984, -27.82980252387822517 ) ) ;
#10604 = CARTESIAN_POINT ( 'NONE',  ( -20.20612091757426043, 24.59769958242388910, -16.46550228026404028 ) ) ;
#10603 = CARTESIAN_POINT ( 'NONE',  ( 1.831572820252009626, -144.2101521542831790, 16.14965423926163623 ) ) ;
#10605 = CARTESIAN_POINT ( 'NONE',  ( 25.70243777736188662, -102.8829101922927691, -46.60897284577268351 ) ) ;
#10606 = ORIENTED_EDGE ( 'NONE', *, *, #16250, .F. ) ;
#10607 = ORIENTED_EDGE ( 'NONE', *, *, #18518, .F. ) ;
#10608 = CARTESIAN_POINT ( 'NONE',  ( 25.64700659047695197, 56.65258046470393083, -97.67001118499042889 ) ) ;
#10609 = LINE ( 'NONE', #19377, #27734 ) ;
#10611 = CARTESIAN_POINT ( 'NONE',  ( 2.263178607246686180, 46.26071628252450552, 137.8402782326812712 ) ) ;
#10610 = DIRECTION ( 'NONE',  ( -1.000000000000000000, -0.000000000000000000, -0.000000000000000000 ) ) ;
#10612 = CARTESIAN_POINT ( 'NONE',  ( 25.81918753295379432, -76.32043280377756389, -83.36706424720522079 ) ) ;
#10613 = CARTESIAN_POINT ( 'NONE',  ( 25.64670758986457955, 97.53391148296672952, 56.88615781331523635 ) ) ;
#10614 = CARTESIAN_POINT ( 'NONE',  ( -8.786685647604890903, -23.24040270374424466, -48.22796981442760256 ) ) ;
#10615 = VERTEX_POINT ( 'NONE', #984 ) ;
#10616 = CARTESIAN_POINT ( 'NONE',  ( -1.583189561560255143, 2.490696082059864924, -46.33203782964461936 ) ) ;
#10617 = AXIS2_PLACEMENT_3D ( 'NONE', #9396, #4480, #601 ) ;
#10618 = CARTESIAN_POINT ( 'NONE',  ( -55.24271866751342941, 0.004256484107795918508, -0.008488649505343059953 ) ) ;
#10620 = VECTOR ( 'NONE', #24053, 999.9999999999997726 ) ;
#10619 = CARTESIAN_POINT ( 'NONE',  ( -22.23226125620929139, -31.55376588768476509, 2.179935373562780221 ) ) ;
#10621 = CARTESIAN_POINT ( 'NONE',  ( 26.11404676487259024, -103.8885755249566643, -45.01677474591514283 ) ) ;
#10622 = AXIS2_PLACEMENT_3D ( 'NONE', #3091, #16031, #9565 ) ;
#10623 = VERTEX_POINT ( 'NONE', #9774 ) ;
#10624 = CARTESIAN_POINT ( 'NONE',  ( -25.21435515916043357, -15.02493970636125198, 31.17620025257602379 ) ) ;
#10625 = VECTOR ( 'NONE', #26554, 1000.000000000000114 ) ;
#10626 = CARTESIAN_POINT ( 'NONE',  ( 109.1721716018069515, -0.008358834333177977277, -0.01488186354165293469 ) ) ;
#10627 = ORIENTED_EDGE ( 'NONE', *, *, #20311, .F. ) ;
#10628 = CARTESIAN_POINT ( 'NONE',  ( 28.37644542392844826, -80.14194118792646293, -95.06674036596292865 ) ) ;
#10629 =( BOUNDED_SURFACE ( )  B_SPLINE_SURFACE ( 3, 1, ( 
 ( #18355, #22714 ),
 ( #9595, #27138 ),
 ( #7164, #16207 ),
 ( #22856, #15569 ) ),
 .UNSPECIFIED., .F., .F., .F. ) 
 B_SPLINE_SURFACE_WITH_KNOTS ( ( 4, 4 ),
 ( 2, 2 ),
 ( 0.000000000000000000, 1.000000000000000000 ),
 ( 0.000000000000000000, 1.000000000000000000 ),
 .UNSPECIFIED. ) 
 GEOMETRIC_REPRESENTATION_ITEM ( )  RATIONAL_B_SPLINE_SURFACE ( (
 ( 1.000000000000000000, 1.000000000000000000),
 ( 0.7789835883360578528, 0.9689951854195403280),
 ( 0.7789835883360578528, 0.9689951854195403280),
 ( 1.000000000000000000, 1.000000000000000000) ) ) 
 REPRESENTATION_ITEM ( '' )  SURFACE ( )  );
#10630 = EDGE_CURVE ( 'NONE', #4919, #4083, #2575, .T. ) ;
#10631 = CARTESIAN_POINT ( 'NONE',  ( 32.73300124599741423, -92.86301839379967760, -72.21147546950645335 ) ) ;
#10632 = CARTESIAN_POINT ( 'NONE',  ( 2.433796855181205476, 137.9325382748285165, 46.34326152018790168 ) ) ;
#10633 = EDGE_CURVE ( 'NONE', #27511, #4864, #1410, .T. ) ;
#10634 = VERTEX_POINT ( 'NONE', #25736 ) ;
#10635 = LINE ( 'NONE', #12499, #25450 ) ;
#10636 = CARTESIAN_POINT ( 'NONE',  ( -1.045287976400362417, 37.92705037016796155, 25.66401692419947977 ) ) ;
#10637 = CARTESIAN_POINT ( 'NONE',  ( 26.04756280548352976, 55.62433096787562192, -98.56594554799059438 ) ) ;
#10638 = EDGE_CURVE ( 'NONE', #18596, #25142, #18008, .T. ) ;
#10639 = CONICAL_SURFACE ( 'NONE', #3762, 28.92774122539760384, 0.7853981625000054922 ) ;
#10640 = DIRECTION ( 'NONE',  ( -0.5914120900931443270, 0.7023121577978127528, 0.3962188444547265487 ) ) ;
#10641 = CARTESIAN_POINT ( 'NONE',  ( 1.833603222531960730, -137.8693250773474688, -45.26427810763046011 ) ) ;
#10642 = CARTESIAN_POINT ( 'NONE',  ( -22.23226125620943705, 16.78323347921918796, -26.80886670319641851 ) ) ;
#10643 = CARTESIAN_POINT ( 'NONE',  ( -1.049817751779876351, -0.5106138415323642210, 45.79652915392416190 ) ) ;
#10644 = AXIS2_PLACEMENT_3D ( 'NONE', #24320, #19840, #9055 ) ;
#10645 = CARTESIAN_POINT ( 'NONE',  ( 26.11404676487259024, -57.58742681967517285, 97.48350837663589630 ) ) ;
#10646 = ADVANCED_FACE ( 'NONE', ( #25873 ), #15332, .F. ) ;
#10647 = CARTESIAN_POINT ( 'NONE',  ( 28.43349137099851021, 86.10800331998767376, 89.57679848841816295 ) ) ;
#10648 = PLANE ( 'NONE',  #11155 ) ;
#10649 = CARTESIAN_POINT ( 'NONE',  ( -20.24419206586954090, -10.37009329716784656, -27.76448493191440292 ) ) ;
#10650 = ORIENTED_EDGE ( 'NONE', *, *, #8070, .F. ) ;
#10651 = AXIS2_PLACEMENT_3D ( 'NONE', #12113, #1172, #24793 ) ;
#10652 = EDGE_LOOP ( 'NONE', ( #10051, #16919, #9749, #14817 ) ) ;
#10653 = ORIENTED_EDGE ( 'NONE', *, *, #16479, .T. ) ;
#10654 = CARTESIAN_POINT ( 'NONE',  ( -20.20700224038492721, -23.35150625415671755, -18.19058640100215385 ) ) ;
#10655 = CARTESIAN_POINT ( 'NONE',  ( -1.539760825549689294, 16.63252404870416257, 43.19716078875421772 ) ) ;
#10656 = CARTESIAN_POINT ( 'NONE',  ( 2.430230287190581429, 16.65331920325930781, -144.5585181921884157 ) ) ;
#10657 = CARTESIAN_POINT ( 'NONE',  ( -25.21435515916043713, -34.05351380035328646, 6.169479169075816394 ) ) ;
#10658 = CARTESIAN_POINT ( 'NONE',  ( 10.93730112726006354, 149.7554878793152966, -20.69552240458195413 ) ) ;
#10659 = CARTESIAN_POINT ( 'NONE',  ( 55.79472521941426777, -68.96476385670649734, -23.17337251492834227 ) ) ;
#10660 = CARTESIAN_POINT ( 'NONE',  ( -55.25719721206881729, -0.008651607285660899843, 0.007063345920781139223 ) ) ;
#10661 = VERTEX_POINT ( 'NONE', #21830 ) ;
#10662 = CARTESIAN_POINT ( 'NONE',  ( 1.831572820252009626, 107.1759352627519206, -97.82994539998277617 ) ) ;
#10663 = CARTESIAN_POINT ( 'NONE',  ( -55.24340739397742794, 0.007744344507854989193, -0.006539691034608598359 ) ) ;
#10664 = CARTESIAN_POINT ( 'NONE',  ( 1.833691583653552115, 117.6050685739180182, -85.00512109099132374 ) ) ;
#10665 = B_SPLINE_CURVE_WITH_KNOTS ( 'NONE', 3,
 ( #14855, #25677, #8114, #1887, #8250, #10283 ),
 .UNSPECIFIED., .F., .F.,
 ( 4, 2, 4 ),
 ( 1.127570259384924611E-17, 0.0006311636237756805372, 0.001262327247551349799 ),
 .UNSPECIFIED. ) ;
#10666 = CARTESIAN_POINT ( 'NONE',  ( 30.59141879584288048, -60.43012207291027238, 99.26511058698874024 ) ) ;
#10667 = B_SPLINE_CURVE_WITH_KNOTS ( 'NONE', 3,
 ( #13609, #515, #25138, #27278, #7156, #5408, #7291 ),
 .UNSPECIFIED., .F., .F.,
 ( 4, 3, 4 ),
 ( 0.000000000000000000, 0.006568092053401818758, 0.02506242213020845946 ),
 .UNSPECIFIED. ) ;
#10668 = VERTEX_POINT ( 'NONE', #23872 ) ;
#10669 = CARTESIAN_POINT ( 'NONE',  ( -1.619063947482197729, 29.22875152547757338, -35.99532424477389725 ) ) ;
#10670 = CARTESIAN_POINT ( 'NONE',  ( 25.64708010899964208, -11.85684669924894585, -112.2870082086267587 ) ) ;
#10671 = ORIENTED_EDGE ( 'NONE', *, *, #14722, .T. ) ;
#10672 = ORIENTED_EDGE ( 'NONE', *, *, #5422, .F. ) ;
#10673 = ORIENTED_EDGE ( 'NONE', *, *, #10034, .T. ) ;
#10674 = VECTOR ( 'NONE', #1499, 1000.000000000000000 ) ;
#10675 = ADVANCED_FACE ( 'NONE', ( #19524 ), #11975, .T. ) ;
#10676 = CARTESIAN_POINT ( 'NONE',  ( -22.23226125620944771, -16.78323347921898900, 26.80886670319655707 ) ) ;
#10677 = CARTESIAN_POINT ( 'NONE',  ( -25.21435515916025594, 1.749597353048488237E-16, -4.373993382621220594E-17 ) ) ;
#10678 = EDGE_CURVE ( 'NONE', #24940, #24442, #19744, .T. ) ;
#10679 = DIRECTION ( 'NONE',  ( 0.5946245182733607137, -0.4701913299128774315, -0.6521823330503007110 ) ) ;
#10680 = EDGE_CURVE ( 'NONE', #10554, #9705, #6358, .T. ) ;
#10681 = B_SPLINE_CURVE_WITH_KNOTS ( 'NONE', 3,
 ( #23512, #3920, #1471, #27667 ),
 .UNSPECIFIED., .F., .F.,
 ( 4, 4 ),
 ( 1.097135458930219133E-17, 0.008383560773332686053 ),
 .UNSPECIFIED. ) ;
#10682 = B_SPLINE_CURVE_WITH_KNOTS ( 'NONE', 3,
 ( #19210, #1781, #14463, #3524, #8021, #23273 ),
 .UNSPECIFIED., .F., .F.,
 ( 4, 2, 4 ),
 ( 7.757919228897728493E-18, 0.0004335184443140311294, 0.0008670368886280545610 ),
 .UNSPECIFIED. ) ;
#10683 = CARTESIAN_POINT ( 'NONE',  ( 30.59138290137869731, 114.2039707400270458, 21.51300488027170843 ) ) ;
#10684 = ORIENTED_EDGE ( 'NONE', *, *, #27325, .F. ) ;
#10685 = FACE_OUTER_BOUND ( 'NONE', #24668, .T. ) ;
#10686 = CARTESIAN_POINT ( 'NONE',  ( -4.473127245936434626, -31.51789735524219438, -37.94261489385706909 ) ) ;
#10687 = CARTESIAN_POINT ( 'NONE',  ( 10.93730112725977932, -128.3908183996597074, 79.81734490845860819 ) ) ;
#10689 =( BOUNDED_SURFACE ( )  B_SPLINE_SURFACE ( 3, 1, ( 
 ( #2113, #4146 ),
 ( #22133, #10917 ),
 ( #15356, #11194 ),
 ( #6324, #24165 ) ),
 .UNSPECIFIED., .F., .F., .F. ) 
 B_SPLINE_SURFACE_WITH_KNOTS ( ( 4, 4 ),
 ( 2, 2 ),
 ( 0.000000000000000000, 1.000000000000000000 ),
 ( 0.000000000000000000, 1.000000000000000000 ),
 .UNSPECIFIED. ) 
 GEOMETRIC_REPRESENTATION_ITEM ( )  RATIONAL_B_SPLINE_SURFACE ( (
 ( 1.000000000000000000, 1.000000000000000000),
 ( 0.6386103224230316178, 0.9954351624131538845),
 ( 0.6386103224230316178, 0.9954351624131538845),
 ( 1.000000000000000000, 1.000000000000000000) ) ) 
 REPRESENTATION_ITEM ( '' )  SURFACE ( )  );
#10688 = AXIS2_PLACEMENT_3D ( 'NONE', #24446, #678, #2841 ) ;
#10690 = CARTESIAN_POINT ( 'NONE',  ( -1.050230347699842248, -0.2550051351976088121, -45.79907861674080749 ) ) ;
#10691 = CARTESIAN_POINT ( 'NONE',  ( -6.574463467970683261, 44.27173031830773908, 25.96726214983142000 ) ) ;
#10692 = CARTESIAN_POINT ( 'NONE',  ( -55.24390624410018802, -0.01027195578987734684, 0.001811362924359352471 ) ) ;
#10693 = VECTOR ( 'NONE', #27094, 1000.000000000000114 ) ;
#10694 = CARTESIAN_POINT ( 'NONE',  ( 26.11404676487257603, 107.3263591096430218, 36.06104232266487486 ) ) ;
#10695 = CARTESIAN_POINT ( 'NONE',  ( 109.1721716018069515, -0.01281875973823909734, 0.01127028715939367397 ) ) ;
#10696 = CARTESIAN_POINT ( 'NONE',  ( 1.831572820252009626, 73.40899645746004865, 125.1738732943812664 ) ) ;
#10697 = ORIENTED_EDGE ( 'NONE', *, *, #7169, .F. ) ;
#10698 = ORIENTED_EDGE ( 'NONE', *, *, #27421, .T. ) ;
#10699 = CARTESIAN_POINT ( 'NONE',  ( 109.1586059443104944, -0.001198897580739041041, 0.006971743774739755720 ) ) ;
#10700 = CARTESIAN_POINT ( 'NONE',  ( -1.050229599974477068, 45.79907399707867199, 0.2556477501661113538 ) ) ;
#10701 = ORIENTED_EDGE ( 'NONE', *, *, #24753, .T. ) ;
#10702 = VERTEX_POINT ( 'NONE', #17354 ) ;
#10703 = VERTEX_POINT ( 'NONE', #19795 ) ;
#10704 = EDGE_CURVE ( 'NONE', #17963, #25814, #1567, .T. ) ;
#10705 = VECTOR ( 'NONE', #19950, 999.9999999999998863 ) ;
#10706 = EDGE_CURVE ( 'NONE', #25074, #6918, #9520, .T. ) ;
#10707 = CARTESIAN_POINT ( 'NONE',  ( -25.21435515916043002, 30.48034229288640162, -16.39063784838753790 ) ) ;
#10708 = CARTESIAN_POINT ( 'NONE',  ( 1.833485406944043827, -73.01664920993054864, 125.4007332306543105 ) ) ;
#10709 = EDGE_CURVE ( 'NONE', #9246, #14330, #16579, .T. ) ;
#10710 = B_SPLINE_CURVE_WITH_KNOTS ( 'NONE', 3,
 ( #900, #27525, #5220, #20906 ),
 .UNSPECIFIED., .F., .F.,
 ( 4, 4 ),
 ( 1.920770561445796063E-16, 0.001982023823822942447 ),
 .UNSPECIFIED. ) ;
#10711 = LINE ( 'NONE', #23688, #22685 ) ;
#10712 = CARTESIAN_POINT ( 'NONE',  ( -20.38016308990357928, 7.753479680700950283, -28.74660391518346714 ) ) ;
#10713 = CARTESIAN_POINT ( 'NONE',  ( -8.786685647604890903, 38.68584556812300690, -37.00619870957947910 ) ) ;
#10714 = CARTESIAN_POINT ( 'NONE',  ( -4.780792508754329262, 45.80716263181262349, 18.84172549606824987 ) ) ;
#10715 = VECTOR ( 'NONE', #15134, 1000.000000000000114 ) ;
#10716 = CARTESIAN_POINT ( 'NONE',  ( 109.1721716018069657, -0.001583175916619938188, 0.01699510305644696614 ) ) ;
#10717 = CARTESIAN_POINT ( 'NONE',  ( -15.02187109954795119, 6.234056423739480657, -45.93032478317444856 ) ) ;
#10718 =( BOUNDED_SURFACE ( )  B_SPLINE_SURFACE ( 3, 1, ( 
 ( #22258, #2516 ),
 ( #15910, #9302 ),
 ( #7581, #18497 ),
 ( #18199, #26842 ) ),
 .UNSPECIFIED., .F., .F., .F. ) 
 B_SPLINE_SURFACE_WITH_KNOTS ( ( 4, 4 ),
 ( 2, 2 ),
 ( 0.000000000000000000, 1.000000000000000000 ),
 ( 0.000000000000000000, 1.000000000000000000 ),
 .UNSPECIFIED. ) 
 GEOMETRIC_REPRESENTATION_ITEM ( )  RATIONAL_B_SPLINE_SURFACE ( (
 ( 1.000000000000000000, 1.000000000000000000),
 ( 0.9934239774497837239, 0.8357310067453919133),
 ( 0.9934239774497837239, 0.8357310067453919133),
 ( 1.000000000000000000, 1.000000000000000000) ) ) 
 REPRESENTATION_ITEM ( '' )  SURFACE ( )  );
#10719 = ORIENTED_EDGE ( 'NONE', *, *, #15354, .F. ) ;
#10720 = ORIENTED_EDGE ( 'NONE', *, *, #26031, .F. ) ;
#10722 = CARTESIAN_POINT ( 'NONE',  ( 25.64670758986459376, -56.88615781331557741, 97.53391148296655899 ) ) ;
#10721 = CARTESIAN_POINT ( 'NONE',  ( 109.1592201516379674, -0.002134489919768192863, 0.007566779963325561721 ) ) ;
#10723 = FACE_OUTER_BOUND ( 'NONE', #19887, .T. ) ;
#10724 = CARTESIAN_POINT ( 'NONE',  ( 2.430230287190572103, 31.67257033707700131, -142.0258656395018591 ) ) ;
#10725 = DIRECTION ( 'NONE',  ( 5.541455922705463698E-20, -5.223019709708320524E-21, 1.000000000000000000 ) ) ;
#10726 = CARTESIAN_POINT ( 'NONE',  ( -55.25719721206881729, 0.01115102788683387629, -0.0006290797159233242576 ) ) ;
#10727 = AXIS2_PLACEMENT_3D ( 'NONE', #16041, #26415, #9013 ) ;
#10728 = ORIENTED_EDGE ( 'NONE', *, *, #21782, .T. ) ;
#10729 = CARTESIAN_POINT ( 'NONE',  ( 1.893872463202064260, 145.1467500857187929, 0.9528309182402651123 ) ) ;
#10730 = CIRCLE ( 'NONE', #19855, 151.1787379149930359 ) ;
#10731 = CARTESIAN_POINT ( 'NONE',  ( -5.986830583229486358, -33.39046620690942291, -38.20088153919488860 ) ) ;
#10732 = CARTESIAN_POINT ( 'NONE',  ( -1.048996300304505747, -37.49570739463903379, -26.29666317565288480 ) ) ;
#10733 = ORIENTED_EDGE ( 'NONE', *, *, #15184, .F. ) ;
#10734 = ORIENTED_EDGE ( 'NONE', *, *, #20336, .T. ) ;
#10735 = CARTESIAN_POINT ( 'NONE',  ( 10.93730112725990367, -133.3192575531795399, -71.28103789255078482 ) ) ;
#10736 = EDGE_CURVE ( 'NONE', #15797, #22192, #19787, .T. ) ;
#10737 = ORIENTED_EDGE ( 'NONE', *, *, #28165, .T. ) ;
#10738 = CARTESIAN_POINT ( 'NONE',  ( 109.1592201516379674, -0.002913740842108687636, -0.007302213399779916743 ) ) ;
#10739 = ORIENTED_EDGE ( 'NONE', *, *, #9594, .F. ) ;
#10740 = EDGE_CURVE ( 'NONE', #21908, #3673, #23612, .T. ) ;
#10741 = EDGE_CURVE ( 'NONE', #26085, #18255, #18882, .T. ) ;
#10742 = CARTESIAN_POINT ( 'NONE',  ( 10.93730112725995873, 4.928439153522441885, -151.0983828010091656 ) ) ;
#10743 = AXIS2_PLACEMENT_3D ( 'NONE', #3331, #18276, #16282 ) ;
#10744 = CARTESIAN_POINT ( 'NONE',  ( -55.24340739397742794, 0.009386184976285603249, -0.003826481709800144074 ) ) ;
#10745 = ORIENTED_EDGE ( 'NONE', *, *, #4039, .T. ) ;
#10746 = CARTESIAN_POINT ( 'NONE',  ( -1.019300379054419947, 42.90269154183450695, 16.06793277091947658 ) ) ;
#10747 = CARTESIAN_POINT ( 'NONE',  ( -22.23342874802668234, -11.82490389046295043, 29.33662284748872651 ) ) ;
#10748 = CARTESIAN_POINT ( 'NONE',  ( 13.36082413113061307, -135.4964217943312121, 70.90215303572075811 ) ) ;
#10749 = CARTESIAN_POINT ( 'NONE',  ( -1.031422197589716205, -25.67058493451416368, 37.93675465142500514 ) ) ;
#10750 = DIRECTION ( 'NONE',  ( -0.7071067818211357325, 4.902845705138444274E-18, 0.7071067805519594129 ) ) ;
#10751 = FACE_OUTER_BOUND ( 'NONE', #3977, .T. ) ;
#10752 = CARTESIAN_POINT ( 'NONE',  ( 55.79472521941426777, -15.83764557006318796, 71.00924468211151463 ) ) ;
#10753 = CARTESIAN_POINT ( 'NONE',  ( 25.64660436782555308, -103.3839381879728876, -45.39454672041220107 ) ) ;
#10755 = CARTESIAN_POINT ( 'NONE',  ( -1.044556982611268614, 45.76404732357880079, -1.643392503292874895 ) ) ;
#10754 = CARTESIAN_POINT ( 'NONE',  ( 1.832998868059858122, -144.2584710144581663, 15.69902610990328640 ) ) ;
#10756 = CARTESIAN_POINT ( 'NONE',  ( -25.21435515916025594, 1.749597353048488237E-16, -4.373993382621220594E-17 ) ) ;
#10757 = EDGE_LOOP ( 'NONE', ( #20893, #20719, #2345, #28130 ) ) ;
#10758 = VERTEX_POINT ( 'NONE', #26556 ) ;
#10759 = CARTESIAN_POINT ( 'NONE',  ( 10.93730112725982373, -142.1801301103788262, 51.37919228020236773 ) ) ;
#10760 = LINE ( 'NONE', #17495, #25452 ) ;
#10762 = CARTESIAN_POINT ( 'NONE',  ( -25.21435515916042647, 25.00736669481023355, -23.92354251275945742 ) ) ;
#10761 = CARTESIAN_POINT ( 'NONE',  ( -18.41936578851709783, 37.37524689996197935, -20.09935324538209045 ) ) ;
#10763 = CARTESIAN_POINT ( 'NONE',  ( -7.711401346138397450, -47.70038152767074990, 21.83927363365083707 ) ) ;
#10764 = CARTESIAN_POINT ( 'NONE',  ( -20.21097721650786738, 8.835581399095163491, -28.26295598655176633 ) ) ;
#10765 = CIRCLE ( 'NONE', #13433, 44.74884827092600403 ) ;
#10766 = ORIENTED_EDGE ( 'NONE', *, *, #5397, .F. ) ;
#10767 = CARTESIAN_POINT ( 'NONE',  ( -1.019300379054419947, -2.023851374322355845, 45.76814864815092676 ) ) ;
#10768 = EDGE_CURVE ( 'NONE', #15152, #14205, #24629, .T. ) ;
#10769 = CARTESIAN_POINT ( 'NONE',  ( 1.833485406944043827, -29.64752363041439764, -142.0485807715649003 ) ) ;
#10770 = CARTESIAN_POINT ( 'NONE',  ( 8.186469829614351212, -149.3111477833938636, -3.468244397268659629 ) ) ;
#10771 = CARTESIAN_POINT ( 'NONE',  ( 55.79472521941426777, 71.00924468211157148, 15.83764557006294993 ) ) ;
#10772 = VERTEX_POINT ( 'NONE', #15468 ) ;
#10773 =( BOUNDED_SURFACE ( )  B_SPLINE_SURFACE ( 3, 1, ( 
 ( #11025, #17487 ),
 ( #12745, #6289 ),
 ( #17071, #25862 ),
 ( #17343, #8871 ) ),
 .UNSPECIFIED., .F., .F., .F. ) 
 B_SPLINE_SURFACE_WITH_KNOTS ( ( 4, 4 ),
 ( 2, 2 ),
 ( 0.000000000000000000, 1.000000000000000000 ),
 ( 0.000000000000000000, 1.000000000000000000 ),
 .UNSPECIFIED. ) 
 GEOMETRIC_REPRESENTATION_ITEM ( )  RATIONAL_B_SPLINE_SURFACE ( (
 ( 1.000000000000000000, 1.000000000000000000),
 ( 0.9956975270656955868, 0.8568959468854907557),
 ( 0.9956975270656955868, 0.8568959468854907557),
 ( 1.000000000000000000, 1.000000000000000000) ) ) 
 REPRESENTATION_ITEM ( '' )  SURFACE ( )  );
#10774 = EDGE_CURVE ( 'NONE', #17852, #14882, #13625, .T. ) ;
#10775 = EDGE_CURVE ( 'NONE', #17914, #24750, #13891, .T. ) ;
#10776 = VERTEX_POINT ( 'NONE', #364 ) ;
#10777 = DIRECTION ( 'NONE',  ( -0.7637818620346800147, -0.6201872550346679835, -0.1788995134688763367 ) ) ;
#10778 = VERTEX_POINT ( 'NONE', #659 ) ;
#10779 = CARTESIAN_POINT ( 'NONE',  ( -1.044557008772710516, -36.05793264791363129, -28.22896138707358205 ) ) ;
#10780 = CARTESIAN_POINT ( 'NONE',  ( 32.73300124599732186, 0.000000000000000000, 0.000000000000000000 ) ) ;
#10781 = CARTESIAN_POINT ( 'NONE',  ( 2.433796855181219243, -71.49415740225165905, 126.7346379669253622 ) ) ;
#10782 = DIRECTION ( 'NONE',  ( -1.000000000000000000, -0.000000000000000000, -0.000000000000000000 ) ) ;
#10783 = FACE_OUTER_BOUND ( 'NONE', #8550, .T. ) ;
#10784 = CARTESIAN_POINT ( 'NONE',  ( 25.64681081121879203, -110.3564950173080206, -23.88203588908195130 ) ) ;
#10785 = CARTESIAN_POINT ( 'NONE',  ( 25.64708228042120197, 23.43704872438759423, 110.4520805602535916 ) ) ;
#10786 = CARTESIAN_POINT ( 'NONE',  ( 24.22246935314087324, 0.000000000000000000, 0.000000000000000000 ) ) ;
#10787 = CARTESIAN_POINT ( 'NONE',  ( -2.265401668238148591, 2.645701981445804929, -46.93990709177545995 ) ) ;
#10788 = CARTESIAN_POINT ( 'NONE',  ( 28.37603512858451538, -93.86378016273927472, -65.97809844506220145 ) ) ;
#10789 = DIRECTION ( 'NONE',  ( 0.000000000000000000, 5.223019709707975211E-21, -1.000000000000000000 ) ) ;
#10790 = CARTESIAN_POINT ( 'NONE',  ( 55.79472521941426777, -63.36760613016249977, 35.74479459808824799 ) ) ;
#10791 = CARTESIAN_POINT ( 'NONE',  ( -55.24271866751342941, 0.009369360294296127586, 0.001545935011630553526 ) ) ;
#10792 = ORIENTED_EDGE ( 'NONE', *, *, #13412, .F. ) ;
#10793 = ORIENTED_EDGE ( 'NONE', *, *, #6410, .F. ) ;
#10794 = EDGE_LOOP ( 'NONE', ( #18183, #25979, #7295, #10004 ) ) ;
#10795 = CARTESIAN_POINT ( 'NONE',  ( -1.048172774974293064, -43.23017713506512649, 15.11899685083868761 ) ) ;
#10796 = FACE_OUTER_BOUND ( 'NONE', #17937, .T. ) ;
#10797 = CARTESIAN_POINT ( 'NONE',  ( 109.1586900883932856, 0.0006456433529162480898, 0.007109207791181754860 ) ) ;
#10798 = CARTESIAN_POINT ( 'NONE',  ( 2.433796855181233454, -98.43889364293788447, -107.1581411821795626 ) ) ;
#10799 = CARTESIAN_POINT ( 'NONE',  ( -25.21435515916025594, 34.29329011225976132, 4.655591116594488099 ) ) ;
#10800 = CARTESIAN_POINT ( 'NONE',  ( 55.79472521941428198, 43.35047097963449403, 58.42842213658343553 ) ) ;
#10801 = LINE ( 'NONE', #19152, #19380 ) ;
#10802 = ORIENTED_EDGE ( 'NONE', *, *, #8880, .F. ) ;
#10803 = CARTESIAN_POINT ( 'NONE',  ( 26.11404676487257603, -65.63269960453305885, 92.25884714080386573 ) ) ;
#10804 = CARTESIAN_POINT ( 'NONE',  ( 109.1589550718175161, -0.003284595046935084688, -0.006826119083824118937 ) ) ;
#10805 = EDGE_CURVE ( 'NONE', #8222, #10266, #12910, .T. ) ;
#10806 = EDGE_CURVE ( 'NONE', #21774, #11861, #21182, .T. ) ;
#10807 = B_SPLINE_CURVE_WITH_KNOTS ( 'NONE', 3,
 ( #5577, #14344, #18963, #23162, #7904, #27742, #25594 ),
 .UNSPECIFIED., .F., .F.,
 ( 4, 3, 4 ),
 ( 5.204170427930421283E-18, 0.02816610861753244405, 0.04000277880656212537 ),
 .UNSPECIFIED. ) ;
#10808 = CARTESIAN_POINT ( 'NONE',  ( -1.539760825549689516, -43.19716078875427456, 16.63252404870400269 ) ) ;
#10809 =( BOUNDED_SURFACE ( )  B_SPLINE_SURFACE ( 3, 1, ( 
 ( #10692, #28226 ),
 ( #8528, #17290 ),
 ( #6365, #15117 ),
 ( #13116, #8804 ) ),
 .UNSPECIFIED., .F., .F., .F. ) 
 B_SPLINE_SURFACE_WITH_KNOTS ( ( 4, 4 ),
 ( 2, 2 ),
 ( 0.000000000000000000, 1.000000000000000000 ),
 ( 0.000000000000000000, 1.000000000000000000 ),
 .UNSPECIFIED. ) 
 GEOMETRIC_REPRESENTATION_ITEM ( )  RATIONAL_B_SPLINE_SURFACE ( (
 ( 1.000000000000000000, 1.000000000000000000),
 ( 0.9934239774497837239, 0.8357310067453919133),
 ( 0.9934239774497837239, 0.8357310067453919133),
 ( 1.000000000000000000, 1.000000000000000000) ) ) 
 REPRESENTATION_ITEM ( '' )  SURFACE ( )  );
#10810 = ORIENTED_EDGE ( 'NONE', *, *, #7834, .F. ) ;
#10812 = ADVANCED_FACE ( 'NONE', ( #2371 ), #18221, .F. ) ;
#10811 = CARTESIAN_POINT ( 'NONE',  ( 99.22246935314079508, -90.00000000000005684, -40.00000000000002842 ) ) ;
#10813 = CARTESIAN_POINT ( 'NONE',  ( 25.64681081121879203, -11.38886654529598275, -112.3352186517031726 ) ) ;
#10814 = ORIENTED_EDGE ( 'NONE', *, *, #21290, .T. ) ;
#10815 = B_SPLINE_CURVE_WITH_KNOTS ( 'NONE', 3,
 ( #20883, #5332, #13966, #12108, #5480, #22921, #16127, #9961 ),
 .UNSPECIFIED., .F., .F.,
 ( 4, 2, 2, 4 ),
 ( 0.000000000000000000, 0.002761524886576651946, 0.005523049773153303893, 0.01104609954630660952 ),
 .UNSPECIFIED. ) ;
#10816 = EDGE_CURVE ( 'NONE', #26927, #12310, #18426, .T. ) ;
#10817 = VERTEX_POINT ( 'NONE', #9580 ) ;
#10818 = ORIENTED_EDGE ( 'NONE', *, *, #6948, .F. ) ;
#10819 = CARTESIAN_POINT ( 'NONE',  ( -20.57838717382308147, -10.78122205917020437, -27.96569011373082603 ) ) ;
#10820 = FACE_OUTER_BOUND ( 'NONE', #4431, .T. ) ;
#10821 = CARTESIAN_POINT ( 'NONE',  ( -55.24271866751342941, 0.009388511352198142604, 0.001425019990782173561 ) ) ;
#10822 = FACE_OUTER_BOUND ( 'NONE', #27118, .T. ) ;
#10823 = EDGE_CURVE ( 'NONE', #4924, #27145, #17045, .T. ) ;
#10824 = CARTESIAN_POINT ( 'NONE',  ( -8.786685647604890903, 37.00619870957935120, -38.68584556812312059 ) ) ;
#10825 = EDGE_LOOP ( 'NONE', ( #11183, #21888, #8670, #6409 ) ) ;
#10826 = CARTESIAN_POINT ( 'NONE',  ( -1.046936909428682450, -43.93225665392624535, -12.93351869073256388 ) ) ;
#10827 = CARTESIAN_POINT ( 'NONE',  ( -25.21435515916043357, 6.169479169075458458, -34.05351380035335751 ) ) ;
#10828 = LINE ( 'NONE', #15256, #27137 ) ;
#10829 = CARTESIAN_POINT ( 'NONE',  ( 6.224689322667630975, 2.565137105445823185, -148.0369967195762513 ) ) ;
#10830 = CARTESIAN_POINT ( 'NONE',  ( -12.82751273423881599, 8.715310691360238948, -48.09651489336683738 ) ) ;
#10831 = CARTESIAN_POINT ( 'NONE',  ( -1.583189561560253589, 2.490696082060518624, 46.33203782964458384 ) ) ;
#10832 = CARTESIAN_POINT ( 'NONE',  ( 1.893872463202077805, -29.24569695044139905, -142.1730500379301532 ) ) ;
#10833 = EDGE_CURVE ( 'NONE', #27728, #25430, #22206, .T. ) ;
#10834 = CARTESIAN_POINT ( 'NONE',  ( -20.20700224038492010, -10.08426345511570332, 27.82980252387829623 ) ) ;
#10835 = B_SPLINE_CURVE_WITH_KNOTS ( 'NONE', 3,
 ( #17571, #6660, #17849, #15406, #26493, #24358, #11526, #11110, #17992, #18554 ),
 .UNSPECIFIED., .F., .F.,
 ( 4, 3, 3, 4 ),
 ( 3.642919299551294898E-17, 0.0002669559177086183342, 0.0005339118354150966701, 0.001067817517169159913 ),
 .UNSPECIFIED. ) ;
#10836 = CARTESIAN_POINT ( 'NONE',  ( -23.79223135445719706, -16.82181692922836547, -28.60983116549958538 ) ) ;
#10837 = ORIENTED_EDGE ( 'NONE', *, *, #24362, .F. ) ;
#10838 = VERTEX_POINT ( 'NONE', #4836 ) ;
#10839 = EDGE_CURVE ( 'NONE', #1176, #21489, #24978, .T. ) ;
#10840 = CARTESIAN_POINT ( 'NONE',  ( 13.84597867724977505, -40.76072889493656248, -140.9259526407712713 ) ) ;
#10841 = ORIENTED_EDGE ( 'NONE', *, *, #21886, .F. ) ;
#10842 = VERTEX_POINT ( 'NONE', #3390 ) ;
#10843 = ORIENTED_EDGE ( 'NONE', *, *, #26899, .F. ) ;
#10844 = CARTESIAN_POINT ( 'NONE',  ( 1.831572820252009626, 86.09108691067770280, 116.8148281295972168 ) ) ;
#10845 = PRODUCT_DEFINITION_SHAPE ( 'NONE', 'NONE',  #25506 ) ;
#10846 = LINE ( 'NONE', #8676, #2787 ) ;
#10847 = B_SPLINE_CURVE_WITH_KNOTS ( 'NONE', 3,
 ( #3559, #5744, #23174, #16377, #10213, #18973 ),
 .UNSPECIFIED., .F., .F.,
 ( 4, 2, 4 ),
 ( 4.679414566804424472E-16, 0.003576372551511269784, 0.007152745103022071192 ),
 .UNSPECIFIED. ) ;
#10848 = CARTESIAN_POINT ( 'NONE',  ( 1.832998868059890096, 45.34898734666227682, -137.8420662456165644 ) ) ;
#10849 =( BOUNDED_SURFACE ( )  B_SPLINE_SURFACE ( 3, 1, ( 
 ( #15053, #15119 ),
 ( #4342, #2304 ),
 ( #21617, #28231 ),
 ( #11252, #2458 ) ),
 .UNSPECIFIED., .F., .F., .F. ) 
 B_SPLINE_SURFACE_WITH_KNOTS ( ( 4, 4 ),
 ( 2, 2 ),
 ( 0.000000000000000000, 1.000000000000000000 ),
 ( 0.000000000000000000, 1.000000000000000000 ),
 .UNSPECIFIED. ) 
 GEOMETRIC_REPRESENTATION_ITEM ( )  RATIONAL_B_SPLINE_SURFACE ( (
 ( 1.000000000000000000, 1.000000000000000000),
 ( 0.6386103224230302855, 0.9954351624131538845),
 ( 0.6386103224230302855, 0.9954351624131538845),
 ( 1.000000000000000000, 1.000000000000000000) ) ) 
 REPRESENTATION_ITEM ( '' )  SURFACE ( )  );
#10850 = CARTESIAN_POINT ( 'NONE',  ( 109.1778270068192853, -0.005967275455169835166, -0.007152128381194115120 ) ) ;
#10851 = CARTESIAN_POINT ( 'NONE',  ( -8.786685647604890903, -23.24040270374424466, -48.22796981442760256 ) ) ;
#10852 = DIRECTION ( 'NONE',  ( -0.5946245182733607137, -0.5401723099040838250, -0.5955128528260831278 ) ) ;
#10853 = CARTESIAN_POINT ( 'NONE',  ( 55.79472521941426777, -66.16469064668278577, -30.25520714117973142 ) ) ;
#10854 = CARTESIAN_POINT ( 'NONE',  ( -25.21435515916043357, 31.17620025257608418, 15.02493970636113474 ) ) ;
#10855 = CARTESIAN_POINT ( 'NONE',  ( -10.86508079875801691, 6.877801422380844798, -50.67624451685624365 ) ) ;
#10856 = VERTEX_POINT ( 'NONE', #22845 ) ;
#10857 = ORIENTED_EDGE ( 'NONE', *, *, #22833, .T. ) ;
#10858 = CARTESIAN_POINT ( 'NONE',  ( -28.13707043255157103, -0.7675454997508607269, -22.88591869784690402 ) ) ;
#10859 = EDGE_CURVE ( 'NONE', #2880, #20917, #4352, .T. ) ;
#10860 = CARTESIAN_POINT ( 'NONE',  ( -55.24198130335446422, -0.008252882783649790471, 0.004276389980776089048 ) ) ;
#10861 = CARTESIAN_POINT ( 'NONE',  ( -6.588769196390771299, 11.07780292579764847, 50.13301368233286581 ) ) ;
#10862 = CARTESIAN_POINT ( 'NONE',  ( -1.113548883309555482, -42.96943836789115778, -16.03115934825511957 ) ) ;
#10863 = CARTESIAN_POINT ( 'NONE',  ( -23.79223135445719350, -28.60983116549952143, 16.82181692922848626 ) ) ;
#10864 = VERTEX_POINT ( 'NONE', #23271 ) ;
#10865 = CARTESIAN_POINT ( 'NONE',  ( -7.078251931573400491, 34.59014398252916322, -38.93060825814240644 ) ) ;
#10867 = EDGE_CURVE ( 'NONE', #28052, #13932, #14658, .T. ) ;
#10866 = LINE ( 'NONE', #28260, #18439 ) ;
#10868 = LINE ( 'NONE', #26253, #6139 ) ;
#10869 = VERTEX_POINT ( 'NONE', #5404 ) ;
#10870 = ORIENTED_EDGE ( 'NONE', *, *, #10775, .F. ) ;
#10871 = EDGE_CURVE ( 'NONE', #26876, #7314, #18789, .T. ) ;
#10872 = CARTESIAN_POINT ( 'NONE',  ( -8.786685647604890903, -9.545808661480982948, -52.67761315067281913 ) ) ;
#10873 = ORIENTED_EDGE ( 'NONE', *, *, #10706, .F. ) ;
#10874 = CARTESIAN_POINT ( 'NONE',  ( -23.77929240705206837, -32.66578242509734054, 15.74261278740706338 ) ) ;
#10875 = ORIENTED_EDGE ( 'NONE', *, *, #10064, .F. ) ;
#10876 = CARTESIAN_POINT ( 'NONE',  ( 109.1587776205901861, 0.005880209827414124152, -0.004375189885423126993 ) ) ;
#10877 = FACE_OUTER_BOUND ( 'NONE', #17645, .T. ) ;
#10878 = EDGE_CURVE ( 'NONE', #1317, #8855, #15660, .T. ) ;
#10879 = CARTESIAN_POINT ( 'NONE',  ( 9.884929003653608603, -19.90991253123348059, 149.2134106160915508 ) ) ;
#10880 = CARTESIAN_POINT ( 'NONE',  ( 2.430230287190572103, -46.34481016236920681, 137.9371479820460991 ) ) ;
#10881 =( BOUNDED_SURFACE ( )  B_SPLINE_SURFACE ( 3, 1, ( 
 ( #27346, #13671 ),
 ( #20878, #25069 ),
 ( #7802, #16122 ),
 ( #18135, #20585 ) ),
 .UNSPECIFIED., .F., .F., .F. ) 
 B_SPLINE_SURFACE_WITH_KNOTS ( ( 4, 4 ),
 ( 2, 2 ),
 ( 0.000000000000000000, 1.000000000000000000 ),
 ( 0.000000000000000000, 1.000000000000000000 ),
 .UNSPECIFIED. ) 
 GEOMETRIC_REPRESENTATION_ITEM ( )  RATIONAL_B_SPLINE_SURFACE ( (
 ( 1.000000000000000000, 1.000000000000000000),
 ( 0.6386103224230302855, 0.9954351624131538845),
 ( 0.6386103224230302855, 0.9954351624131538845),
 ( 1.000000000000000000, 1.000000000000000000) ) ) 
 REPRESENTATION_ITEM ( '' )  SURFACE ( )  );
#10882 = CARTESIAN_POINT ( 'NONE',  ( -4.473127245936434626, -41.70021447285072469, -26.34600523034523434 ) ) ;
#10883 = CARTESIAN_POINT ( 'NONE',  ( 1.833485406944043827, -97.49333871408619245, -107.4794113447419477 ) ) ;
#10884 = CARTESIAN_POINT ( 'NONE',  ( 25.73574536432414206, -112.2643803187784641, -12.61003673872005137 ) ) ;
#10885 = B_SPLINE_CURVE_WITH_KNOTS ( 'NONE', 3,
 ( #26815, #8986, #4657, #13424, #22224, #7549, #25539, #7989, #5512, #18904 ),
 .UNSPECIFIED., .F., .F.,
 ( 4, 2, 2, 2, 4 ),
 ( 2.976713740813343128E-16, 0.0003346187017559132675, 0.0006692374035115289214, 0.001003856105267144630, 0.001338474807022760121 ),
 .UNSPECIFIED. ) ;
#10886 = CARTESIAN_POINT ( 'NONE',  ( 25.87036335909426299, 103.6841944152907047, 45.07965203034955692 ) ) ;
#10888 = FACE_OUTER_BOUND ( 'NONE', #23462, .T. ) ;
#10887 = CARTESIAN_POINT ( 'NONE',  ( 2.430230287190581429, -13.76600171652546045, -144.8619874886008176 ) ) ;
#10889 = ORIENTED_EDGE ( 'NONE', *, *, #2500, .T. ) ;
#10890 = VERTEX_POINT ( 'NONE', #14314 ) ;
#10891 = CARTESIAN_POINT ( 'NONE',  ( 32.73300124599732186, 0.000000000000000000, 0.000000000000000000 ) ) ;
#10892 = FACE_OUTER_BOUND ( 'NONE', #10186, .T. ) ;
#10893 = CARTESIAN_POINT ( 'NONE',  ( -1.031422197589716205, 45.78027046666444733, -1.530725436377611715 ) ) ;
#10894 = EDGE_CURVE ( 'NONE', #26453, #9221, #14291, .T. ) ;
#10895 = CARTESIAN_POINT ( 'NONE',  ( -4.178947244162633190, -45.38689110596704523, 18.28784278438497068 ) ) ;
#10896 = CARTESIAN_POINT ( 'NONE',  ( 32.73300124599741423, 115.8010721414085822, -20.69176323058512423 ) ) ;
#10897 = CARTESIAN_POINT ( 'NONE',  ( -4.780792508754318604, 18.84172549606871883, -45.80716263181242454 ) ) ;
#10898 = EDGE_LOOP ( 'NONE', ( #8564, #22879, #15128, #7997 ) ) ;
#10899 = CARTESIAN_POINT ( 'NONE',  ( 1.833721034905632541, -44.50273803002032480, 138.1171912769429468 ) ) ;
#10900 = DIRECTION ( 'NONE',  ( 1.000000000000000000, -0.000000000000000000, -0.000000000000000000 ) ) ;
#10901 = B_SPLINE_CURVE_WITH_KNOTS ( 'NONE', 3,
 ( #25023, #22862, #11328, #3122 ),
 .UNSPECIFIED., .F., .F.,
 ( 4, 4 ),
 ( 0.000000000000000000, 0.008383560773332727686 ),
 .UNSPECIFIED. ) ;
#10902 = CARTESIAN_POINT ( 'NONE',  ( 25.64699802086725811, 112.3172869996024730, 11.56593161917351864 ) ) ;
#10903 = CARTESIAN_POINT ( 'NONE',  ( -55.25297051322618813, -0.01354497706059463319, 0.006313402748432140991 ) ) ;
#10904 = ORIENTED_EDGE ( 'NONE', *, *, #20434, .T. ) ;
#10905 = VERTEX_POINT ( 'NONE', #3106 ) ;
#10906 = FACE_OUTER_BOUND ( 'NONE', #22104, .T. ) ;
#10907 = CARTESIAN_POINT ( 'NONE',  ( 1.833603222531972055, 15.61050054119223063, -144.2675221341992540 ) ) ;
#10908 = CARTESIAN_POINT ( 'NONE',  ( 32.73300124599739291, 89.94078864464164269, -75.82012867748392182 ) ) ;
#10909 = ORIENTED_EDGE ( 'NONE', *, *, #13971, .T. ) ;
#10910 = CARTESIAN_POINT ( 'NONE',  ( 28.37603512858454380, 93.86378016273968683, 65.97809844506153354 ) ) ;
#10911 = CARTESIAN_POINT ( 'NONE',  ( 1.833485406944057594, 108.1939177044926055, 96.69979900902202985 ) ) ;
#10912 = ORIENTED_EDGE ( 'NONE', *, *, #8409, .T. ) ;
#10913 = CARTESIAN_POINT ( 'NONE',  ( -1.045287976400362417, -12.68782741917263657, 44.00138577190661948 ) ) ;
#10914 = LINE ( 'NONE', #1983, #17957 ) ;
#10915 = DIRECTION ( 'NONE',  ( -1.000000000000000000, 6.938893903907226837E-18, -1.734723475976806709E-18 ) ) ;
#10916 = CARTESIAN_POINT ( 'NONE',  ( 25.86096068574581253, 46.89265070732260199, -102.8701285401536865 ) ) ;
#10917 = CARTESIAN_POINT ( 'NONE',  ( 9.884929003653626367, 139.1775604444703731, 57.36421526887207989 ) ) ;
#10918 = CARTESIAN_POINT ( 'NONE',  ( 19.66333377628716050, -99.30798531455278066, -95.46107873288976009 ) ) ;
#10919 = CARTESIAN_POINT ( 'NONE',  ( -2.904412668506655582, 2.864640348250632851, -47.56768199507435213 ) ) ;
#10920 = CARTESIAN_POINT ( 'NONE',  ( 26.11404676487257603, 110.9778746459746941, 22.43340081644806006 ) ) ;
#10921 = EDGE_CURVE ( 'NONE', #8760, #11237, #25568, .T. ) ;
#10922 = CARTESIAN_POINT ( 'NONE',  ( 2.430230287190572103, 96.28466919684099423, 109.1043569252017562 ) ) ;
#10923 = CARTESIAN_POINT ( 'NONE',  ( 1.832998868059890096, -117.0819875546689701, -85.72499093308219642 ) ) ;
#10924 = CARTESIAN_POINT ( 'NONE',  ( 26.11404676487257603, 112.7148551500680469, 10.71016160607605627 ) ) ;
#10925 = EDGE_LOOP ( 'NONE', ( #2469, #23969, #23358, #1488 ) ) ;
#10926 = EDGE_CURVE ( 'NONE', #8537, #21319, #2616, .T. ) ;
#10927 = VERTEX_POINT ( 'NONE', #14462 ) ;
#10928 = CARTESIAN_POINT ( 'NONE',  ( -1.050230346682675231, -43.55772679531839486, 14.15203301556477378 ) ) ;
#10929 = CARTESIAN_POINT ( 'NONE',  ( -8.786685647604896232, 9.545808661481343549, 52.67761315067276229 ) ) ;
#10930 = CARTESIAN_POINT ( 'NONE',  ( 2.263178607246667973, -98.32595927618783094, -107.1074316126228183 ) ) ;
#10931 = CARTESIAN_POINT ( 'NONE',  ( -1.463510566862832984, 43.13857742234528558, 16.57250862017374970 ) ) ;
#10932 =( BOUNDED_SURFACE ( )  B_SPLINE_SURFACE ( 3, 1, ( 
 ( #2252, #28451 ),
 ( #8755, #17523 ),
 ( #19824, #6605 ),
 ( #4148, #15358 ) ),
 .UNSPECIFIED., .F., .F., .F. ) 
 B_SPLINE_SURFACE_WITH_KNOTS ( ( 4, 4 ),
 ( 2, 2 ),
 ( 0.000000000000000000, 1.000000000000000000 ),
 ( 0.000000000000000000, 1.000000000000000000 ),
 .UNSPECIFIED. ) 
 GEOMETRIC_REPRESENTATION_ITEM ( )  RATIONAL_B_SPLINE_SURFACE ( (
 ( 1.000000000000000000, 1.000000000000000000),
 ( 0.6386103224230316178, 0.9954351624131538845),
 ( 0.6386103224230316178, 0.9954351624131538845),
 ( 1.000000000000000000, 1.000000000000000000) ) ) 
 REPRESENTATION_ITEM ( '' )  SURFACE ( )  );
#10933 = CARTESIAN_POINT ( 'NONE',  ( 28.37644542392854063, -102.9230687709012244, 69.76573497039046856 ) ) ;
#10934 = CARTESIAN_POINT ( 'NONE',  ( -1.045287976400362417, 25.66401692419989899, -37.92705037016767733 ) ) ;
#10935 = ORIENTED_EDGE ( 'NONE', *, *, #8343, .F. ) ;
#10936 = CARTESIAN_POINT ( 'NONE',  ( 1.833485406944057594, 30.69200235378934849, 141.8265699653868523 ) ) ;
#10937 = CARTESIAN_POINT ( 'NONE',  ( -20.57838717382308147, 25.16001208503129760, 16.28767523336092893 ) ) ;
#10938 = CARTESIAN_POINT ( 'NONE',  ( 109.1778270068192853, 0.005186985107090136965, -0.007736698406808922672 ) ) ;
#10939 = FACE_OUTER_BOUND ( 'NONE', #1070, .T. ) ;
#10940 = CARTESIAN_POINT ( 'NONE',  ( 109.1721716018069515, 0.005466227998627255259, -0.01616973485710007305 ) ) ;
#10941 = ORIENTED_EDGE ( 'NONE', *, *, #25483, .T. ) ;
#10942 = CARTESIAN_POINT ( 'NONE',  ( -25.21435515916025594, 34.29329011225976132, 4.655591116594488099 ) ) ;
#10943 = CARTESIAN_POINT ( 'NONE',  ( 109.1592201516379674, -0.006044422199822568030, 0.005027640251767196387 ) ) ;
#10944 = ORIENTED_EDGE ( 'NONE', *, *, #6909, .T. ) ;
#10945 = VERTEX_POINT ( 'NONE', #942 ) ;
#10946 = ORIENTED_EDGE ( 'NONE', *, *, #1932, .T. ) ;
#10947 = CARTESIAN_POINT ( 'NONE',  ( -21.41427618760458884, 11.22988868156184772, -28.68857606049970244 ) ) ;
#10948 = CARTESIAN_POINT ( 'NONE',  ( -1.583189561560252701, -2.490696082059551397, 46.33203782964464068 ) ) ;
#10949 = CARTESIAN_POINT ( 'NONE',  ( -55.24390624410018802, -0.004896917417127438256, -0.009209468562451287102 ) ) ;
#10950 = AXIS2_PLACEMENT_3D ( 'NONE', #7959, #28062, #21163 ) ;
#10951 = EDGE_CURVE ( 'NONE', #10065, #23186, #25806, .T. ) ;
#10952 = ORIENTED_EDGE ( 'NONE', *, *, #18728, .T. ) ;
#10953 = EDGE_CURVE ( 'NONE', #335, #20657, #24886, .T. ) ;
#10954 = CARTESIAN_POINT ( 'NONE',  ( -20.57838717382308147, -7.715628353033886278, -28.96176188950215646 ) ) ;
#10955 = CARTESIAN_POINT ( 'NONE',  ( 10.93730112725977932, -115.5857507957709913, 97.44200844886238144 ) ) ;
#10956 = ORIENTED_EDGE ( 'NONE', *, *, #5392, .T. ) ;
#10957 = EDGE_CURVE ( 'NONE', #4229, #7217, #23952, .T. ) ;
#10958 = CARTESIAN_POINT ( 'NONE',  ( 1.833603222531960952, 85.65285110156294479, -117.1340888386541224 ) ) ;
#10959 = CARTESIAN_POINT ( 'NONE',  ( 1.833485406944043827, 142.0485807715649571, -29.64752363041402816 ) ) ;
#10960 = DIRECTION ( 'NONE',  ( -1.000000000000000000, -0.000000000000000000, -0.000000000000000000 ) ) ;
#10961 = CARTESIAN_POINT ( 'NONE',  ( -8.786685647604885574, 6.096987947571466530E-17, -1.524246986892866633E-17 ) ) ;
#10962 = CARTESIAN_POINT ( 'NONE',  ( -5.986830583229481029, 26.01297580803325360, -43.56094206392965873 ) ) ;
#10963 = EDGE_CURVE ( 'NONE', #28334, #26729, #21848, .T. ) ;
#10964 = FACE_OUTER_BOUND ( 'NONE', #23567, .T. ) ;
#10965 = CARTESIAN_POINT ( 'NONE',  ( 8.186469829614372529, -57.56191610809284498, -137.8131829164341582 ) ) ;
#10966 = CARTESIAN_POINT ( 'NONE',  ( 32.73300124599732186, 0.000000000000000000, 0.000000000000000000 ) ) ;
#10967 = B_SPLINE_CURVE_WITH_KNOTS ( 'NONE', 3,
 ( #27472, #20425, #10076, #25185, #5310, #18398, #707, #20566, #7784, #16538 ),
 .UNSPECIFIED., .F., .F.,
 ( 4, 3, 3, 4 ),
 ( 3.816391647148975608E-17, 0.0002669559177086078174, 0.0005339118354150857197, 0.001067817517169160780 ),
 .UNSPECIFIED. ) ;
#10968 = CARTESIAN_POINT ( 'NONE',  ( 5.340103556456443634, -2.303180381359250628, 147.4316330165019622 ) ) ;
#10969 = DIRECTION ( 'NONE',  ( 0.000000000000000000, -1.000000000000000000, 0.000000000000000000 ) ) ;
#10970 = CARTESIAN_POINT ( 'NONE',  ( -1.056502255334264895, -27.33667001641194361, -36.75727364034722200 ) ) ;
#10971 = CIRCLE ( 'NONE', #28406, 20.00000000000000000 ) ;
#10972 = CARTESIAN_POINT ( 'NONE',  ( 9.884929003653608603, 124.2095058357589039, -85.04731144912386753 ) ) ;
#10973 = ORIENTED_EDGE ( 'NONE', *, *, #28160, .F. ) ;
#10974 = VECTOR ( 'NONE', #7804, 1000.000000000000000 ) ;
#10975 = ORIENTED_EDGE ( 'NONE', *, *, #8707, .F. ) ;
#10976 = CARTESIAN_POINT ( 'NONE',  ( -8.786685647604892679, -53.04920435127177569, 7.199674155859498548 ) ) ;
#10977 = CARTESIAN_POINT ( 'NONE',  ( 25.69398547355838858, 35.60637981494853221, 107.1830796521255422 ) ) ;
#10978 = ORIENTED_EDGE ( 'NONE', *, *, #27825, .F. ) ;
#10979 = EDGE_LOOP ( 'NONE', ( #23553, #13398, #6553, #18440 ) ) ;
#10980 = ORIENTED_EDGE ( 'NONE', *, *, #2905, .T. ) ;
#10981 = CARTESIAN_POINT ( 'NONE',  ( 109.1586900883932856, 0.002995460350188396646, 0.006479576224398257700 ) ) ;
#10982 = CARTESIAN_POINT ( 'NONE',  ( 1.833750490713684345, 137.9248034078897547, 45.09517546033693947 ) ) ;
#10983 = ADVANCED_FACE ( 'NONE', ( #4225 ), #2598, .F. ) ;
#10984 = EDGE_CURVE ( 'NONE', #26085, #13800, #13264, .T. ) ;
#10985 = FACE_OUTER_BOUND ( 'NONE', #16488, .T. ) ;
#10986 = CARTESIAN_POINT ( 'NONE',  ( -1.463510566862831208, -46.14841196428341874, -2.430838777910016901 ) ) ;
#10987 = CARTESIAN_POINT ( 'NONE',  ( -1.583189561560256253, 38.94740041318330981, 25.21827308671188916 ) ) ;
#10988 = EDGE_CURVE ( 'NONE', #27119, #3338, #495, .T. ) ;
#10989 = CARTESIAN_POINT ( 'NONE',  ( -4.473127245936431073, 3.196405119333807221, -49.22197550883368677 ) ) ;
#10990 = CARTESIAN_POINT ( 'NONE',  ( -1.463510566862832984, 43.13857742234528558, 16.57250862017374970 ) ) ;
#10991 = CARTESIAN_POINT ( 'NONE',  ( -16.86833981943425442, 20.94590537750608661, -38.94907963570727816 ) ) ;
#10992 = CARTESIAN_POINT ( 'NONE',  ( 32.73300124599740002, 110.6325518752278896, -39.98094346392192477 ) ) ;
#10993 = CARTESIAN_POINT ( 'NONE',  ( -1.045287976400362417, 25.66401692420069125, 37.92705037016716574 ) ) ;
#10994 = CARTESIAN_POINT ( 'NONE',  ( -1.619063947482197729, -2.489035965909835557, 46.30105812165550816 ) ) ;
#10995 = VERTEX_POINT ( 'NONE', #8278 ) ;
#10996 = ORIENTED_EDGE ( 'NONE', *, *, #21504, .T. ) ;
#10998 = CARTESIAN_POINT ( 'NONE',  ( -55.25297051322618813, 0.01019003092403517226, 0.01093108995494820879 ) ) ;
#10997 = CARTESIAN_POINT ( 'NONE',  ( 32.73300124599732186, 0.000000000000000000, 0.000000000000000000 ) ) ;
#10999 = CARTESIAN_POINT ( 'NONE',  ( 1.833485406944043827, 15.69895494453577101, -144.2578170162061326 ) ) ;
#11000 = CARTESIAN_POINT ( 'NONE',  ( 32.73300124599735028, 8.473903470906103408, 117.3295799645430151 ) ) ;
#11001 = CARTESIAN_POINT ( 'NONE',  ( 8.186469829614225091, -19.05650981809914057, 148.1306754360700211 ) ) ;
#11002 = CARTESIAN_POINT ( 'NONE',  ( 1.831572820252009626, -71.69925593429898925, 126.1609924456727754 ) ) ;
#11003 = VERTEX_POINT ( 'NONE', #14744 ) ;
#11004 = CARTESIAN_POINT ( 'NONE',  ( 25.64700659047697684, 97.89757946487087281, -56.25842064175987645 ) ) ;
#11005 = ORIENTED_EDGE ( 'NONE', *, *, #19908, .F. ) ;
#11006 = CARTESIAN_POINT ( 'NONE',  ( -20.21097721650786738, -17.13687097598118925, 24.14932365326971464 ) ) ;
#11007 = CARTESIAN_POINT ( 'NONE',  ( -1.050229599974477734, -26.71319688967661676, -37.20249516760164710 ) ) ;
#11008 = ORIENTED_EDGE ( 'NONE', *, *, #5063, .F. ) ;
#11009 = ORIENTED_EDGE ( 'NONE', *, *, #11022, .T. ) ;
#11010 = CARTESIAN_POINT ( 'NONE',  ( 60.46576798286869803, -4.195655488513964285E-16, 1.048913872128491071E-16 ) ) ;
#11011 = EDGE_LOOP ( 'NONE', ( #13497, #14290, #8532, #21778 ) ) ;
#11012 = CARTESIAN_POINT ( 'NONE',  ( 2.430230287190592531, -43.58368230469486804, 138.8342928068218498 ) ) ;
#11013 = B_SPLINE_CURVE_WITH_KNOTS ( 'NONE', 3,
 ( #16761, #14231, #2887, #26762, #7077, #27040, #24645, #26908 ),
 .UNSPECIFIED., .F., .F.,
 ( 4, 2, 2, 4 ),
 ( 1.962615573354718958E-17, 0.0002429592666046852441, 0.0004859185332093508640, 0.0009718370664186700694 ),
 .UNSPECIFIED. ) ;
#11014 = VERTEX_POINT ( 'NONE', #15148 ) ;
#11015 = CARTESIAN_POINT ( 'NONE',  ( 1.833206308920042105, -125.2945011813201006, -73.19872517709852389 ) ) ;
#11016 = CARTESIAN_POINT ( 'NONE',  ( -55.24390624410018802, 0.009209468562451588944, -0.004896917417127890151 ) ) ;
#11017 = VERTEX_POINT ( 'NONE', #21369 ) ;
#11018 = CARTESIAN_POINT ( 'NONE',  ( -55.24390624410018802, 0.004896917417131886954, -0.009209468562452662738 ) ) ;
#11019 = EDGE_CURVE ( 'NONE', #8336, #7588, #11543, .T. ) ;
#11020 = CARTESIAN_POINT ( 'NONE',  ( -25.21435515916025594, 1.749597353048488237E-16, -4.373993382621220594E-17 ) ) ;
#11021 = CARTESIAN_POINT ( 'NONE',  ( 9.884929003653608603, -132.4189379373575548, 71.59798461011283166 ) ) ;
#11022 = EDGE_CURVE ( 'NONE', #17054, #26729, #8422, .T. ) ;
#11023 = FACE_OUTER_BOUND ( 'NONE', #2405, .T. ) ;
#11024 = CARTESIAN_POINT ( 'NONE',  ( -1.048172774974287291, 13.17853518375297739, -43.86067135048624266 ) ) ;
#11025 = CARTESIAN_POINT ( 'NONE',  ( 109.1586900883932856, 0.006960773163856030267, 0.001582822706024277024 ) ) ;
#11026 = EDGE_CURVE ( 'NONE', #5021, #7441, #28352, .T. ) ;
#11027 = B_SPLINE_CURVE_WITH_KNOTS ( 'NONE', 3,
 ( #294, #2595, #13821, #24926, #24497, #13381, #18137, #3043 ),
 .UNSPECIFIED., .F., .F.,
 ( 4, 2, 2, 4 ),
 ( 0.000000000000000000, 0.002761524886576660186, 0.005523049773153320373, 0.01104609954630662340 ),
 .UNSPECIFIED. ) ;
#11028 = CARTESIAN_POINT ( 'NONE',  ( 1.833838850093453043, 125.6687428896159417, 72.55487854850731821 ) ) ;
#11029 = CARTESIAN_POINT ( 'NONE',  ( 109.1592201516379674, -0.002720803050370518023, -0.007376275279032888654 ) ) ;
#11030 = CARTESIAN_POINT ( 'NONE',  ( 25.64700659047696263, -56.65258046470324871, 97.67001118499082679 ) ) ;
#11031 = ORIENTED_EDGE ( 'NONE', *, *, #22681, .F. ) ;
#11032 = CARTESIAN_POINT ( 'NONE',  ( -1.046935749539997573, -27.93995161054667875, 36.28605774377793125 ) ) ;
#11033 = CARTESIAN_POINT ( 'NONE',  ( -12.94347594948485103, 23.08810053288751263, 42.93165645342833869 ) ) ;
#11034 = CARTESIAN_POINT ( 'NONE',  ( 10.93730112726006354, 148.8212007290666747, -26.59437931460595905 ) ) ;
#11035 = CARTESIAN_POINT ( 'NONE',  ( -1.539763995773685723, 11.93465967526358185, 44.72359274866469292 ) ) ;
#11036 = CARTESIAN_POINT ( 'NONE',  ( 25.64681081121879203, -35.28660243342475411, -107.2555980796244910 ) ) ;
#11037 = CARTESIAN_POINT ( 'NONE',  ( 1.832998868059858122, -59.50898020732601879, 132.3466930259791923 ) ) ;
#11038 = LINE ( 'NONE', #26152, #594 ) ;
#11039 = CARTESIAN_POINT ( 'NONE',  ( 16.05277956358201408, 80.40847413522703846, -118.6216415718953527 ) ) ;
#11040 = ORIENTED_EDGE ( 'NONE', *, *, #18793, .F. ) ;
#11041 = CARTESIAN_POINT ( 'NONE',  ( -4.473127245936431073, 26.34600523034598396, 41.70021447285024863 ) ) ;
#11042 = CIRCLE ( 'NONE', #6085, 117.6351876552689504 ) ;
#11043 = CARTESIAN_POINT ( 'NONE',  ( -1.259920593601974392, 45.95412615877143026, 2.243284667987943681 ) ) ;
#11044 = AXIS2_PLACEMENT_3D ( 'NONE', #6097, #8243, #27944 ) ;
#11045 = ORIENTED_EDGE ( 'NONE', *, *, #22391, .T. ) ;
#11046 = CARTESIAN_POINT ( 'NONE',  ( 109.1624594426973118, -0.01503296564241274336, 0.005372302061316216668 ) ) ;
#11047 = CARTESIAN_POINT ( 'NONE',  ( -90.83090735639699176, 4.592425496802575156E-15, 37.50000000000001421 ) ) ;
#11048 = CARTESIAN_POINT ( 'NONE',  ( 26.11404676487257603, 57.58742681967585497, -97.48350837663548418 ) ) ;
#11049 = ADVANCED_FACE ( 'NONE', ( #10723 ), #24133, .F. ) ;
#11050 = ORIENTED_EDGE ( 'NONE', *, *, #26238, .T. ) ;
#11051 = DIRECTION ( 'NONE',  ( 1.000000000000000000, 0.000000000000000000, 0.000000000000000000 ) ) ;
#11052 = CYLINDRICAL_SURFACE ( 'NONE', #5566, 37.50000000000001421 ) ;
#11053 = CARTESIAN_POINT ( 'NONE',  ( 32.73300124599740002, -8.473903470905288060, -117.3295799645430151 ) ) ;
#11054 = CARTESIAN_POINT ( 'NONE',  ( 55.79472521941426777, -71.00924468211145779, -15.83764557006343487 ) ) ;
#11055 = DIRECTION ( 'NONE',  ( -0.000000000000000000, 0.000000000000000000, 1.000000000000000000 ) ) ;
#11056 = CARTESIAN_POINT ( 'NONE',  ( 1.833838850093452599, -132.5643635152038655, 59.02146106675034787 ) ) ;
#11057 = ORIENTED_EDGE ( 'NONE', *, *, #7388, .F. ) ;
#11058 = CARTESIAN_POINT ( 'NONE',  ( -55.24198130335446422, 0.009190321388310579431, -0.001391250620101621869 ) ) ;
#11059 = ORIENTED_EDGE ( 'NONE', *, *, #27157, .F. ) ;
#11061 = ORIENTED_EDGE ( 'NONE', *, *, #4002, .T. ) ;
#11060 = AXIS2_PLACEMENT_3D ( 'NONE', #212, #22525, #489 ) ;
#11062 = ORIENTED_EDGE ( 'NONE', *, *, #375, .T. ) ;
#11063 = CONICAL_SURFACE ( 'NONE', #1849, 117.6351876552689504, 0.9945805576725580410 ) ;
#11064 = CARTESIAN_POINT ( 'NONE',  ( -1.046936909428679341, -27.93981068760648157, -36.28616897897442328 ) ) ;
#11065 = CARTESIAN_POINT ( 'NONE',  ( -20.37983603106074071, 28.74620395171562492, -7.753708011498657626 ) ) ;
#11066 = CARTESIAN_POINT ( 'NONE',  ( -20.57838717382308147, -7.715628353033886278, -28.96176188950215646 ) ) ;
#11067 = AXIS2_PLACEMENT_3D ( 'NONE', #8905, #12921, #2251 ) ;
#11068 = CARTESIAN_POINT ( 'NONE',  ( 2.108985857320933466, -98.16869034643225689, -107.1123114102938274 ) ) ;
#11069 = CARTESIAN_POINT ( 'NONE',  ( 1.833838850093452821, 72.55487854850862561, -125.6687428896151886 ) ) ;
#11070 = CARTESIAN_POINT ( 'NONE',  ( -20.90916690077962770, 27.35210456531415346, 28.59207721780114753 ) ) ;
#11071 = ORIENTED_EDGE ( 'NONE', *, *, #19329, .F. ) ;
#11072 = CARTESIAN_POINT ( 'NONE',  ( -55.24198130335446422, 0.009190321388309335635, 0.001391250620105184774 ) ) ;
#11073 = CARTESIAN_POINT ( 'NONE',  ( -21.41430102051751305, 25.94791611261640085, 16.60879216503605704 ) ) ;
#11074=STYLED_ITEM('',(#28528),#17192);
#11075 = CARTESIAN_POINT ( 'NONE',  ( 25.64708228042123395, 23.51409906510363612, -110.4357030047554531 ) ) ;
#11076 = FACE_OUTER_BOUND ( 'NONE', #11253, .T. ) ;
#11077 = DIRECTION ( 'NONE',  ( 1.000000000000000000, -6.938893903907226837E-18, 1.734723475976806709E-18 ) ) ;
#11078 = LINE ( 'NONE', #8635, #12125 ) ;
#11079 = PRODUCT_DEFINITION_SHAPE ( 'NONE', 'NONE',  #28485 ) ;
#11080 = CARTESIAN_POINT ( 'NONE',  ( 1.833809397773861649, -107.9565774559017797, 96.96506043213419446 ) ) ;
#11081 = CARTESIAN_POINT ( 'NONE',  ( -55.25719721206881729, -0.004044147484877910065, -0.01041086141212526316 ) ) ;
#11082 = VERTEX_POINT ( 'NONE', #13146 ) ;
#11083 = ORIENTED_EDGE ( 'NONE', *, *, #21712, .T. ) ;
#11084 = ADVANCED_FACE ( 'NONE', ( #10319 ), #6486, .F. ) ;
#11085 = ORIENTED_EDGE ( 'NONE', *, *, #11835, .T. ) ;
#11086 = EDGE_CURVE ( 'NONE', #10842, #20262, #26970, .T. ) ;
#11087 = VECTOR ( 'NONE', #22955, 1000.000000000000114 ) ;
#11088 = AXIS2_PLACEMENT_3D ( 'NONE', #4536, #19649, #4116 ) ;
#11089 = EDGE_CURVE ( 'NONE', #15583, #3658, #16015, .T. ) ;
#11090 = CARTESIAN_POINT ( 'NONE',  ( -1.056502255334265339, 45.80535052436398047, 0.5104472526221617290 ) ) ;
#11091 = CARTESIAN_POINT ( 'NONE',  ( 6.224689322667647851, 126.9212313063855362, -76.23997225729135607 ) ) ;
#11092 = CARTESIAN_POINT ( 'NONE',  ( 10.93730112725932635, 0.000000000000000000, 0.000000000000000000 ) ) ;
#11093 = ORIENTED_EDGE ( 'NONE', *, *, #13841, .F. ) ;
#11094 = DIRECTION ( 'NONE',  ( 0.7563875759206388771, 0.2351350468682867345, -0.6104009704506935252 ) ) ;
#11095 =( BOUNDED_SURFACE ( )  B_SPLINE_SURFACE ( 3, 1, ( 
 ( #20004, #1879 ),
 ( #19448, #28216 ),
 ( #8518, #12958 ),
 ( #21753, #15836 ) ),
 .UNSPECIFIED., .F., .F., .F. ) 
 B_SPLINE_SURFACE_WITH_KNOTS ( ( 4, 4 ),
 ( 2, 2 ),
 ( 0.000000000000000000, 1.000000000000000000 ),
 ( 0.000000000000000000, 1.000000000000000000 ),
 .UNSPECIFIED. ) 
 GEOMETRIC_REPRESENTATION_ITEM ( )  RATIONAL_B_SPLINE_SURFACE ( (
 ( 1.000000000000000000, 1.000000000000000000),
 ( 0.9593753223639863714, 0.9995975284513187731),
 ( 0.9593753223639863714, 0.9995975284513187731),
 ( 1.000000000000000000, 1.000000000000000000) ) ) 
 REPRESENTATION_ITEM ( '' )  SURFACE ( )  );
#11096 = CARTESIAN_POINT ( 'NONE',  ( -1.113548883309547044, -12.28732181966548609, -44.18588492042589166 ) ) ;
#11097 = ORIENTED_EDGE ( 'NONE', *, *, #16965, .T. ) ;
#11098 = VERTEX_POINT ( 'NONE', #10999 ) ;
#11099 = CARTESIAN_POINT ( 'NONE',  ( 2.108393763691202683, 31.45977531353488033, -141.8460676169241026 ) ) ;
#11100 = CARTESIAN_POINT ( 'NONE',  ( 1.833485406944057594, -45.34878176254139248, -137.8414413349090637 ) ) ;
#11101 = CARTESIAN_POINT ( 'NONE',  ( -1.056502255334265339, -43.72121397317214786, 13.66916755949895546 ) ) ;
#11102 = CARTESIAN_POINT ( 'NONE',  ( -1.619063947482197729, -2.489035965910479486, -46.30105812165547974 ) ) ;
#11103 = CARTESIAN_POINT ( 'NONE',  ( 55.79472521941428198, -71.31192372336666097, -14.41365263906626915 ) ) ;
#11104 = CARTESIAN_POINT ( 'NONE',  ( -20.38016308990358638, 18.69911008768368532, 23.16952666206563549 ) ) ;
#11105 = CARTESIAN_POINT ( 'NONE',  ( -2.904412668506659578, -25.64203923793602868, -40.16685646686200073 ) ) ;
#11106 = AXIS2_PLACEMENT_3D ( 'NONE', #7064, #15662, #4883 ) ;
#11107 = B_SPLINE_CURVE_WITH_KNOTS ( 'NONE', 3,
 ( #12222, #1417, #23606, #7930, #5606, #3995, #3574 ),
 .UNSPECIFIED., .F., .F.,
 ( 4, 3, 4 ),
 ( 0.000000000000000000, 0.02398743853561344230, 0.04000277880656222251 ),
 .UNSPECIFIED. ) ;
#11108 = VECTOR ( 'NONE', #4127, 1000.000000000000114 ) ;
#11109 = CARTESIAN_POINT ( 'NONE',  ( 109.1586900883932856, -0.006130969560687385411, 0.003656351050331833278 ) ) ;
#11110 = CARTESIAN_POINT ( 'NONE',  ( 1.833838848569424806, 15.34509722932533649, 144.2962335061012027 ) ) ;
#11111 = CARTESIAN_POINT ( 'NONE',  ( 109.1586059443104944, -0.004378796245590049069, -0.005555961672773755862 ) ) ;
#11112 = DIRECTION ( 'NONE',  ( -0.5914120900931443270, -0.2567974902965039496, -0.7643865440136131673 ) ) ;
#11113 = ORIENTED_EDGE ( 'NONE', *, *, #13247, .T. ) ;
#11114 = VECTOR ( 'NONE', #7776, 1000.000000000000114 ) ;
#11115 = ADVANCED_FACE ( 'NONE', ( #24824 ), #26894, .F. ) ;
#11116 = ORIENTED_EDGE ( 'NONE', *, *, #8521, .T. ) ;
#11117 = CARTESIAN_POINT ( 'NONE',  ( 1.833485406944043827, -96.69979900902094982, -108.1939177044935860 ) ) ;
#11118 = EDGE_LOOP ( 'NONE', ( #28249, #12181, #5851, #21308 ) ) ;
#11119 = ORIENTED_EDGE ( 'NONE', *, *, #17059, .T. ) ;
#11120 = EDGE_CURVE ( 'NONE', #2861, #24693, #3643, .T. ) ;
#11121 = ORIENTED_EDGE ( 'NONE', *, *, #15719, .T. ) ;
#11122 = EDGE_CURVE ( 'NONE', #24160, #11589, #14325, .T. ) ;
#11123 = CARTESIAN_POINT ( 'NONE',  ( 1.833691583653523249, 137.8971124741068195, 45.17974255430862485 ) ) ;
#11124 = CARTESIAN_POINT ( 'NONE',  ( 26.11404676487259024, 10.71016160607567080, 112.7148551500680753 ) ) ;
#11125 = B_SPLINE_CURVE_WITH_KNOTS ( 'NONE', 3,
 ( #18268, #7224, #13672, #22478, #24925, #13820, #5038 ),
 .UNSPECIFIED., .F., .F.,
 ( 4, 3, 4 ),
 ( 6.534015072584227389E-16, 0.02816610861753247874, 0.04000277880656289559 ),
 .UNSPECIFIED. ) ;
#11126 = CARTESIAN_POINT ( 'NONE',  ( -1.113548883309553927, -45.82026503946952545, -1.968251867498708174 ) ) ;
#11127 = AXIS2_PLACEMENT_3D ( 'NONE', #9877, #7582, #25131 ) ;
#11128 = CARTESIAN_POINT ( 'NONE',  ( 2.263178607246687069, 43.59477707254215062, -138.7064943909641102 ) ) ;
#11129 = CARTESIAN_POINT ( 'NONE',  ( -23.77929240705206482, 31.93650644494365309, 17.17389748746929001 ) ) ;
#11130 = CARTESIAN_POINT ( 'NONE',  ( 19.66333377628691181, -46.81583828063168085, 129.5498775999586485 ) ) ;
#11131 = CARTESIAN_POINT ( 'NONE',  ( 9.884929003653626367, -149.2134106160917497, 19.90991253123197779 ) ) ;
#11132 = CARTESIAN_POINT ( 'NONE',  ( 21.16825799904896144, 127.3716170292830725, -46.02882515936357066 ) ) ;
#11133 = CARTESIAN_POINT ( 'NONE',  ( -18.41936578851717599, 5.707900577128148356, -42.05131332928112187 ) ) ;
#11134 = CARTESIAN_POINT ( 'NONE',  ( 1.833485406944043827, -117.7091014914955309, 84.86072343962528919 ) ) ;
#11135 = ORIENTED_EDGE ( 'NONE', *, *, #14150, .F. ) ;
#11136 = EDGE_LOOP ( 'NONE', ( #25562, #2467, #9496, #18122 ) ) ;
#11138 = FACE_OUTER_BOUND ( 'NONE', #17601, .T. ) ;
#11137 = CARTESIAN_POINT ( 'NONE',  ( -55.24340739397742794, 0.006539691034608862037, 0.007744344507854531226 ) ) ;
#11139 = CARTESIAN_POINT ( 'NONE',  ( 5.340103556456273104, 139.5040934094290606, 47.74933482044414745 ) ) ;
#11140 = CARTESIAN_POINT ( 'NONE',  ( -20.20898968516257810, -0.6607166829021660082, -29.59696826051172280 ) ) ;
#11141 = CARTESIAN_POINT ( 'NONE',  ( -8.786685647604887350, 53.04920435127183254, 7.199674155859139724 ) ) ;
#11142 = VERTEX_POINT ( 'NONE', #15434 ) ;
#11143 = CARTESIAN_POINT ( 'NONE',  ( -55.24271866751342941, -0.001545935011630304593, 0.009369360294295640129 ) ) ;
#11144 = EDGE_CURVE ( 'NONE', #14537, #18454, #25337, .T. ) ;
#11145 = ORIENTED_EDGE ( 'NONE', *, *, #15351, .T. ) ;
#11146 = CARTESIAN_POINT ( 'NONE',  ( 25.70243777736190438, 103.4793210720854262, -45.26941207740190976 ) ) ;
#11147 = CARTESIAN_POINT ( 'NONE',  ( -1.045287976400362417, -28.14015102489855735, -36.12803364096578207 ) ) ;
#11148 = VERTEX_POINT ( 'NONE', #9268 ) ;
#11149 = B_SPLINE_CURVE_WITH_KNOTS ( 'NONE', 3,
 ( #25230, #27222, #1190, #22798, #753, #22942, #7248, #3481 ),
 .UNSPECIFIED., .F., .F.,
 ( 4, 2, 2, 4 ),
 ( 2.211348276820754320E-16, 0.002761568181852866368, 0.005523136363705511559, 0.01104627272741080107 ),
 .UNSPECIFIED. ) ;
#11150 = EDGE_LOOP ( 'NONE', ( #18374, #27990, #8841, #12009 ) ) ;
#11151 = ADVANCED_FACE ( 'NONE', ( #18028 ), #12455, .T. ) ;
#11152 = CARTESIAN_POINT ( 'NONE',  ( 1.832998868059890096, -0.5339089137757804249, 145.1092030902949830 ) ) ;
#11153 = CONICAL_SURFACE ( 'NONE', #7489, 34.60786435723138510, 0.8559913436420825139 ) ;
#11154 = CARTESIAN_POINT ( 'NONE',  ( 1.832998868059890096, 117.7096351258387870, 84.86110816369641441 ) ) ;
#11155 = AXIS2_PLACEMENT_3D ( 'NONE', #23766, #8620, #4570 ) ;
#11156 = ORIENTED_EDGE ( 'NONE', *, *, #27504, .T. ) ;
#11157 = EDGE_CURVE ( 'NONE', #14392, #9282, #17402, .T. ) ;
#11158 = FACE_OUTER_BOUND ( 'NONE', #16800, .T. ) ;
#11159 = EDGE_CURVE ( 'NONE', #565, #19578, #10885, .T. ) ;
#11160 = EDGE_LOOP ( 'NONE', ( #23035, #13810, #21084, #5575 ) ) ;
#11161 = CARTESIAN_POINT ( 'NONE',  ( 109.1778270068192853, -0.008960903982060999459, 0.002542344697958557470 ) ) ;
#11162 = CARTESIAN_POINT ( 'NONE',  ( -20.20700224038492721, -27.82980252387826781, -10.08426345511578504 ) ) ;
#11164 = AXIS2_PLACEMENT_3D ( 'NONE', #20567, #20989, #24908 ) ;
#11163 = CARTESIAN_POINT ( 'NONE',  ( 1.834118845439484335, -97.22976650547497002, 107.7186227765451321 ) ) ;
#11165 = CARTESIAN_POINT ( 'NONE',  ( 8.186469829614047455, 84.95702201190542269, 122.8338389144547307 ) ) ;
#11166 = CIRCLE ( 'NONE', #27247, 34.60786435723138510 ) ;
#11167 = CARTESIAN_POINT ( 'NONE',  ( -20.20700224038492721, -16.58740185276692358, 24.51628800869065827 ) ) ;
#11169 = CARTESIAN_POINT ( 'NONE',  ( 109.1624594426973260, 0.01591840958352308891, -0.001206615835671232158 ) ) ;
#11168 = CARTESIAN_POINT ( 'NONE',  ( 2.063896406836609909, -144.3268707900448646, 16.52087515463731648 ) ) ;
#11170 = CARTESIAN_POINT ( 'NONE',  ( 26.11404676487259024, -112.4785329405482912, 12.95861723607416671 ) ) ;
#11171 = VECTOR ( 'NONE', #18508, 1000.000000000000000 ) ;
#11172 = ORIENTED_EDGE ( 'NONE', *, *, #13583, .F. ) ;
#11173 = CARTESIAN_POINT ( 'NONE',  ( 5.340103579038173010, 17.70136536264663008, 146.3832392131351980 ) ) ;
#11174 = CARTESIAN_POINT ( 'NONE',  ( -1.046936909428682005, -25.87632113675133283, 37.78538189376536849 ) ) ;
#11175 = CARTESIAN_POINT ( 'NONE',  ( -25.21435515916043713, 4.655591116594827383, 34.29329011225949841 ) ) ;
#11176 = CARTESIAN_POINT ( 'NONE',  ( -20.20700224038492721, -28.44216453106531617, 8.199606986804630182 ) ) ;
#11177 = VERTEX_POINT ( 'NONE', #14276 ) ;
#11178 = CARTESIAN_POINT ( 'NONE',  ( -16.86833981943427929, 5.948101187262172296, 43.82216161736197790 ) ) ;
#11179 = CARTESIAN_POINT ( 'NONE',  ( -1.463510566862831430, 46.14841196428341163, 2.430838777910348192 ) ) ;
#11180 = LINE ( 'NONE', #94, #3371 ) ;
#11181 = LINE ( 'NONE', #19957, #8665 ) ;
#11182 = EDGE_CURVE ( 'NONE', #27431, #9334, #14436, .T. ) ;
#11183 = ORIENTED_EDGE ( 'NONE', *, *, #3090, .T. ) ;
#11184 = EDGE_CURVE ( 'NONE', #4432, #5699, #3493, .T. ) ;
#11185 = CARTESIAN_POINT ( 'NONE',  ( 1.833603222531958288, -97.42748212378351980, 107.5392551439151276 ) ) ;
#11186 = ORIENTED_EDGE ( 'NONE', *, *, #18952, .F. ) ;
#11187 = CARTESIAN_POINT ( 'NONE',  ( 28.37603512858451182, 33.74339723237929434, -109.6581134439363723 ) ) ;
#11188 = VECTOR ( 'NONE', #2182, 1000.000000000000114 ) ;
#11189 = LINE ( 'NONE', #9033, #22136 ) ;
#11190 = ORIENTED_EDGE ( 'NONE', *, *, #2594, .F. ) ;
#11191 = CARTESIAN_POINT ( 'NONE',  ( -55.25297051322618813, 0.001818774723749745246, 0.01483298743814625079 ) ) ;
#11192 = CARTESIAN_POINT ( 'NONE',  ( -9.156249394959706578, 9.022661520478530761, 53.74753343182691623 ) ) ;
#11193 = CARTESIAN_POINT ( 'NONE',  ( 25.70243777736189728, 46.60897284577303878, -102.8829101922925986 ) ) ;
#11194 = CARTESIAN_POINT ( 'NONE',  ( 6.224689322667647851, 136.2818611715190400, 57.86870174583473414 ) ) ;
#11195 = CARTESIAN_POINT ( 'NONE',  ( -25.21435515916025594, 1.749597353048488237E-16, -4.373993382621220594E-17 ) ) ;
#11196 = CARTESIAN_POINT ( 'NONE',  ( -1.050229599974474404, -0.2556477501656316820, 45.79907399707867199 ) ) ;
#11197 = ORIENTED_EDGE ( 'NONE', *, *, #15354, .T. ) ;
#11198 = DIRECTION ( 'NONE',  ( 0.000000000000000000, 5.223019709708233256E-21, -1.000000000000000000 ) ) ;
#11199 = CARTESIAN_POINT ( 'NONE',  ( 2.430230287190592531, 144.8619874886006471, 13.76600171652691706 ) ) ;
#11200 = CARTESIAN_POINT ( 'NONE',  ( -1.046936909428695328, 43.14407378092994350, -15.35929614323679893 ) ) ;
#11201 = CARTESIAN_POINT ( 'NONE',  ( -2.911734481061403645, 17.36785190846042681, 44.38410240830284437 ) ) ;
#11202 = ORIENTED_EDGE ( 'NONE', *, *, #14433, .T. ) ;
#11203 = ORIENTED_EDGE ( 'NONE', *, *, #10064, .T. ) ;
#11204 = ORIENTED_EDGE ( 'NONE', *, *, #11233, .T. ) ;
#11205 = CARTESIAN_POINT ( 'NONE',  ( -1.050229599974477734, -26.71319688967661676, -37.20249516760164710 ) ) ;
#11206 = CARTESIAN_POINT ( 'NONE',  ( -55.24390624410018802, 0.001451500391953283731, -0.01032895241566680888 ) ) ;
#11207 = CARTESIAN_POINT ( 'NONE',  ( -1.045287976400379737, -37.92705037016725100, 25.66401692420055269 ) ) ;
#11208 = CARTESIAN_POINT ( 'NONE',  ( -55.24271866751342941, -0.004256484107795216812, 0.008488649505342837909 ) ) ;
#11209 = DIRECTION ( 'NONE',  ( 0.000000000000000000, 0.000000000000000000, 1.000000000000000000 ) ) ;
#11210 = CARTESIAN_POINT ( 'NONE',  ( 25.64700659047695908, -91.21315746821477433, -66.55152787776225409 ) ) ;
#11211 = ORIENTED_EDGE ( 'NONE', *, *, #3353, .F. ) ;
#11212 = CARTESIAN_POINT ( 'NONE',  ( 30.59141879584272061, 115.2623358717303006, 14.83090566979459979 ) ) ;
#11213 = CARTESIAN_POINT ( 'NONE',  ( 30.59141879584274193, 92.40465812955542901, 70.47510900703801440 ) ) ;
#11214 = FACE_BOUND ( 'NONE', #20491, .T. ) ;
#11215 = CARTESIAN_POINT ( 'NONE',  ( -21.81686047589425215, 16.72402253294313823, -34.70276904128894557 ) ) ;
#11216 = CARTESIAN_POINT ( 'NONE',  ( 2.430230287190572103, 86.70145658344814876, -116.8646894862403514 ) ) ;
#11217 = ADVANCED_FACE ( 'NONE', ( #765 ), #9250, .F. ) ;
#11218 = ORIENTED_EDGE ( 'NONE', *, *, #20872, .T. ) ;
#11219 = CARTESIAN_POINT ( 'NONE',  ( -1.323439229708139431, -43.04565903621273293, 16.42345129173381935 ) ) ;
#11220 = CARTESIAN_POINT ( 'NONE',  ( -15.02187109954785171, 45.93032478317463330, 6.234056423739666286 ) ) ;
#11221 = EDGE_CURVE ( 'NONE', #23477, #12482, #1282, .T. ) ;
#11222 = CARTESIAN_POINT ( 'NONE',  ( -9.156249394959713683, 25.18996226954615736, -48.32878616081018208 ) ) ;
#11223 = ORIENTED_EDGE ( 'NONE', *, *, #25339, .T. ) ;
#11224 = EDGE_CURVE ( 'NONE', #17719, #6423, #2972, .T. ) ;
#11225 = B_SPLINE_CURVE_WITH_KNOTS ( 'NONE', 3,
 ( #11453, #13898, #368, #517, #9153, #26982, #18070, #6865 ),
 .UNSPECIFIED., .F., .F.,
 ( 4, 2, 2, 4 ),
 ( 3.469446951953614189E-18, 0.0002429588503611264990, 0.0004859177007222495286, 0.0009718354014444822520 ),
 .UNSPECIFIED. ) ;
#11226 = EDGE_LOOP ( 'NONE', ( #11116, #13184, #8641, #5801 ) ) ;
#11227 = EDGE_LOOP ( 'NONE', ( #12596, #9576, #10792, #19534 ) ) ;
#11228 = DIRECTION ( 'NONE',  ( -0.7637818620346800147, 0.6201872550346668733, 0.1788995134688804445 ) ) ;
#11229 = CARTESIAN_POINT ( 'NONE',  ( 10.93730112725990367, -145.2260730187398678, -42.00474393596407197 ) ) ;
#11230 = CARTESIAN_POINT ( 'NONE',  ( -4.780792508754318604, 18.84172549606871883, -45.80716263181242454 ) ) ;
#11231 = EDGE_LOOP ( 'NONE', ( #19471, #18186, #919, #7902 ) ) ;
#11232 = B_SPLINE_CURVE_WITH_KNOTS ( 'NONE', 3,
 ( #18814, #27877, #14059, #14345 ),
 .UNSPECIFIED., .F., .F.,
 ( 4, 4 ),
 ( 3.283912181224055105E-16, 0.01077107486149822199 ),
 .UNSPECIFIED. ) ;
#11233 = EDGE_CURVE ( 'NONE', #5939, #10890, #3676, .T. ) ;
#11234 = CARTESIAN_POINT ( 'NONE',  ( -1.463510566862832762, -11.94877850058534285, -44.64091840826485935 ) ) ;
#11235 = ORIENTED_EDGE ( 'NONE', *, *, #25756, .T. ) ;
#11236 = CARTESIAN_POINT ( 'NONE',  ( 32.73300124599738581, 108.9684813982494092, -44.31599526637845798 ) ) ;
#11237 = VERTEX_POINT ( 'NONE', #5669 ) ;
#11238 = DIRECTION ( 'NONE',  ( -6.938893903907226837E-18, -1.000000000000000000, 0.000000000000000000 ) ) ;
#11239 = CARTESIAN_POINT ( 'NONE',  ( 25.64703792032469920, -46.06101937225536602, -103.0889146124069953 ) ) ;
#11240 = CARTESIAN_POINT ( 'NONE',  ( 1.893872463202051826, -145.1467500857188213, -0.9528309182412637579 ) ) ;
#11241 = DIRECTION ( 'NONE',  ( -0.5946245182733607137, 0.4045541647807432417, 0.6948076064830672749 ) ) ;
#11242 = CARTESIAN_POINT ( 'NONE',  ( -1.323439229708126774, -12.01475235539415642, 44.47813215539056131 ) ) ;
#11243 = CARTESIAN_POINT ( 'NONE',  ( 25.64681081121879203, 66.70335573067988832, -91.10197563707880875 ) ) ;
#11244 = EDGE_CURVE ( 'NONE', #18571, #13110, #8828, .T. ) ;
#11245 = CARTESIAN_POINT ( 'NONE',  ( 109.1721716018069657, 0.01254847260354827708, -0.01157047143379286505 ) ) ;
#11246 = CARTESIAN_POINT ( 'NONE',  ( -4.473127245936434626, -45.82513704981530367, 18.25038884639918280 ) ) ;
#11247 = EDGE_CURVE ( 'NONE', #15244, #8760, #4693, .T. ) ;
#11248 = CARTESIAN_POINT ( 'NONE',  ( -20.21097721650787093, -8.835581399094968091, 28.26295598655181607 ) ) ;
#11249 = CARTESIAN_POINT ( 'NONE',  ( 25.65782528836480481, -65.90345832277411375, -91.69136324939171345 ) ) ;
#11250 = DIRECTION ( 'NONE',  ( 1.000000000000000000, -6.938893903907226837E-18, 1.734723475976806709E-18 ) ) ;
#11251 = ADVANCED_FACE ( 'NONE', ( #22811 ), #27050, .F. ) ;
#11252 = CARTESIAN_POINT ( 'NONE',  ( 109.1778270068192853, -0.004106684808170070998, -0.008360410075196058124 ) ) ;
#11253 = EDGE_LOOP ( 'NONE', ( #27997, #10363, #12319, #8538 ) ) ;
#11254 = ORIENTED_EDGE ( 'NONE', *, *, #4618, .T. ) ;
#11255 = DIRECTION ( 'NONE',  ( -0.7563875759206389882, 0.03500244528123006016, 0.6531865459554675457 ) ) ;
#11256 = CARTESIAN_POINT ( 'NONE',  ( -55.24390624410018802, 0.01032895241567037548, -0.001451500391950801341 ) ) ;
#11257 = B_SPLINE_CURVE_WITH_KNOTS ( 'NONE', 3,
 ( #4052, #25804, #6507, #24079 ),
 .UNSPECIFIED., .F., .F.,
 ( 4, 4 ),
 ( 0.000000000000000000, 0.01077107196513816915 ),
 .UNSPECIFIED. ) ;
#11258 = EDGE_LOOP ( 'NONE', ( #19293, #7159, #22934, #1440 ) ) ;
#11259 = B_SPLINE_CURVE_WITH_KNOTS ( 'NONE', 3,
 ( #16128, #18583, #22922, #25359, #1446, #24929, #11958, #18271, #23064, #5632 ),
 .UNSPECIFIED., .F., .F.,
 ( 4, 3, 3, 4 ),
 ( 2.775557561562891351E-17, 0.0002669559177086170331, 0.0005339118354151071869, 0.001067817517169159479 ),
 .UNSPECIFIED. ) ;
#11260 = B_SPLINE_CURVE_WITH_KNOTS ( 'NONE', 3,
 ( #24638, #15829, #22020, #8643, #17414, #26199, #15670 ),
 .UNSPECIFIED., .F., .F.,
 ( 4, 3, 4 ),
 ( 4.109830475680215708E-16, 0.02816610861753246833, 0.04000277880656254170 ),
 .UNSPECIFIED. ) ;
#11261 = ORIENTED_EDGE ( 'NONE', *, *, #6532, .F. ) ;
#11262 = ORIENTED_EDGE ( 'NONE', *, *, #15143, .F. ) ;
#11263 = CARTESIAN_POINT ( 'NONE',  ( 1.832998868059858122, 85.72499093308101692, 117.0819875546698512 ) ) ;
#11264 = CARTESIAN_POINT ( 'NONE',  ( -25.21435515916043713, 16.39063784838786475, 30.48034229288620622 ) ) ;
#11265 =( BOUNDED_SURFACE ( )  B_SPLINE_SURFACE ( 3, 1, ( 
 ( #8548, #15287 ),
 ( #23694, #3945 ),
 ( #12713, #10570 ),
 ( #19337, #28113 ) ),
 .UNSPECIFIED., .F., .F., .F. ) 
 B_SPLINE_SURFACE_WITH_KNOTS ( ( 4, 4 ),
 ( 2, 2 ),
 ( 0.000000000000000000, 1.000000000000000000 ),
 ( 0.000000000000000000, 1.000000000000000000 ),
 .UNSPECIFIED. ) 
 GEOMETRIC_REPRESENTATION_ITEM ( )  RATIONAL_B_SPLINE_SURFACE ( (
 ( 1.000000000000000000, 1.000000000000000000),
 ( 0.6386103224230316178, 0.9954351624131538845),
 ( 0.6386103224230316178, 0.9954351624131538845),
 ( 1.000000000000000000, 1.000000000000000000) ) ) 
 REPRESENTATION_ITEM ( '' )  SURFACE ( )  );
#11266 = CARTESIAN_POINT ( 'NONE',  ( 1.832998868059858122, -138.1720401012263721, -44.33343224355373735 ) ) ;
#11267 = CARTESIAN_POINT ( 'NONE',  ( 109.1592201516379674, -0.002913740842108687636, -0.007302213399779916743 ) ) ;
#11268 = CARTESIAN_POINT ( 'NONE',  ( 109.1586900883932856, 0.007002774699553638779, 0.001385221016527484091 ) ) ;
#11269 = CARTESIAN_POINT ( 'NONE',  ( -1.050229599974464634, 43.47850826583074735, 14.39582765040416668 ) ) ;
#11270 = DIRECTION ( 'NONE',  ( 0.000000000000000000, 5.223019709707975211E-21, -1.000000000000000000 ) ) ;
#11271 = CARTESIAN_POINT ( 'NONE',  ( 16.75465622695658041, 4.637075857203486251, -142.1502242093125403 ) ) ;
#11272 = CARTESIAN_POINT ( 'NONE',  ( 109.1721716018069515, -0.0002019688922686823762, 0.01706748904931388797 ) ) ;
#11273 = EDGE_CURVE ( 'NONE', #17203, #3442, #920, .T. ) ;
#11274 = CARTESIAN_POINT ( 'NONE',  ( -1.155031165708890306, 12.20332162035463419, -44.25214473648917135 ) ) ;
#11275 = DIRECTION ( 'NONE',  ( -1.000000000000000000, 0.000000000000000000, 0.000000000000000000 ) ) ;
#11276 = ADVANCED_FACE ( 'NONE', ( #12554 ), #17302, .F. ) ;
#11277 = ORIENTED_EDGE ( 'NONE', *, *, #12967, .F. ) ;
#11279 = CARTESIAN_POINT ( 'NONE',  ( -6.574463467970653952, -50.12924290857544918, -11.01561683920031776 ) ) ;
#11278 = CARTESIAN_POINT ( 'NONE',  ( 26.11404676487257603, 112.7148551500681890, -10.71016160607451262 ) ) ;
#11280 = CARTESIAN_POINT ( 'NONE',  ( 25.70243777736188662, -22.76560620136980617, -110.6300896395619162 ) ) ;
#11281 = CARTESIAN_POINT ( 'NONE',  ( 24.01988960052065281, 80.44223964539966687, -103.4492499592074779 ) ) ;
#11282 = CARTESIAN_POINT ( 'NONE',  ( 9.884929003653608603, 35.39789245780532667, -146.3148513795963481 ) ) ;
#11283 = CARTESIAN_POINT ( 'NONE',  ( -8.786685647604890903, -37.00619870957961410, -38.68584556812286479 ) ) ;
#11284 = ORIENTED_EDGE ( 'NONE', *, *, #21718, .T. ) ;
#11285 = CARTESIAN_POINT ( 'NONE',  ( 1.833603222531956289, -14.72553080638897249, -144.3605362014089906 ) ) ;
#11286 = ORIENTED_EDGE ( 'NONE', *, *, #14854, .T. ) ;
#11287 = CARTESIAN_POINT ( 'NONE',  ( 1.894214914920948845, -84.54370816135659084, 117.9869255019029879 ) ) ;
#11288 = CARTESIAN_POINT ( 'NONE',  ( 1.833206308920066530, 0.7447049373431984254, -145.1075835660718099 ) ) ;
#11289 = VERTEX_POINT ( 'NONE', #10548 ) ;
#11290 = EDGE_LOOP ( 'NONE', ( #23789, #8491, #21055, #18175 ) ) ;
#11291 = CARTESIAN_POINT ( 'NONE',  ( -25.21435515916043713, -31.17620025257598471, -15.02493970636134613 ) ) ;
#11292 = EDGE_LOOP ( 'NONE', ( #7907, #14739, #5520, #14556 ) ) ;
#11293 = FACE_OUTER_BOUND ( 'NONE', #16738, .T. ) ;
#11294 = ORIENTED_EDGE ( 'NONE', *, *, #1361, .F. ) ;
#11295 = EDGE_CURVE ( 'NONE', #18231, #6949, #18093, .T. ) ;
#11296 =( BOUNDED_SURFACE ( )  B_SPLINE_SURFACE ( 3, 1, ( 
 ( #1384, #8040 ),
 ( #23428, #7751 ),
 ( #25453, #20674 ),
 ( #6011, #3413 ) ),
 .UNSPECIFIED., .F., .F., .F. ) 
 B_SPLINE_SURFACE_WITH_KNOTS ( ( 4, 4 ),
 ( 2, 2 ),
 ( 0.000000000000000000, 1.000000000000000000 ),
 ( 0.000000000000000000, 1.000000000000000000 ),
 .UNSPECIFIED. ) 
 GEOMETRIC_REPRESENTATION_ITEM ( )  RATIONAL_B_SPLINE_SURFACE ( (
 ( 1.000000000000000000, 1.000000000000000000),
 ( 0.6386103224230302855, 0.9954351624131538845),
 ( 0.6386103224230302855, 0.9954351624131538845),
 ( 1.000000000000000000, 1.000000000000000000) ) ) 
 REPRESENTATION_ITEM ( '' )  SURFACE ( )  );
#11297 = CARTESIAN_POINT ( 'NONE',  ( -1.048994561756802169, 36.59609844253166244, 27.53485040342854262 ) ) ;
#11298 = CARTESIAN_POINT ( 'NONE',  ( -28.13707043255157103, 14.07296284901359051, 18.06394523322437706 ) ) ;
#11299 = CARTESIAN_POINT ( 'NONE',  ( 1.833485406944057594, 30.69200235378934849, 141.8265699653868523 ) ) ;
#11300 = EDGE_CURVE ( 'NONE', #10427, #9946, #14990, .T. ) ;
#11301 = CARTESIAN_POINT ( 'NONE',  ( 1.833838850093465922, -72.55488452980776515, -125.6687394363104886 ) ) ;
#11302 = EDGE_CURVE ( 'NONE', #9049, #8004, #16140, .T. ) ;
#11303 = B_SPLINE_CURVE_WITH_KNOTS ( 'NONE', 3,
 ( #9377, #13813, #3171, #5182, #15973, #11949, #5471, #22621, #7655, #862 ),
 .UNSPECIFIED., .F., .F.,
 ( 4, 3, 3, 4 ),
 ( 6.938893903907228378E-18, 0.0002669560319015572389, 0.0005492286108966272506, 0.0008315040496093409946 ),
 .UNSPECIFIED. ) ;
#11304 = CARTESIAN_POINT ( 'NONE',  ( 9.884929003653608603, -144.4113244745774693, 42.50195158090983938 ) ) ;
#11305 = DIRECTION ( 'NONE',  ( -1.000000000000000000, -0.000000000000000000, -0.000000000000000000 ) ) ;
#11306 = ADVANCED_FACE ( 'NONE', ( #12828 ), #9427, .F. ) ;
#11307 = VERTEX_POINT ( 'NONE', #5955 ) ;
#11308 = CARTESIAN_POINT ( 'NONE',  ( 1.834118845439484335, -145.1099497418795750, 0.1779704863065216525 ) ) ;
#11309 = CARTESIAN_POINT ( 'NONE',  ( 28.37603512858450117, -33.74339723237861932, 109.6581134439366281 ) ) ;
#11310 = CARTESIAN_POINT ( 'NONE',  ( 2.108985857320909929, -31.46042399111138010, -141.8463279126004295 ) ) ;
#11311 = CARTESIAN_POINT ( 'NONE',  ( -25.21435515916043713, -23.92354251275954979, -25.00736669481013053 ) ) ;
#11312 = CARTESIAN_POINT ( 'NONE',  ( 2.433796855181233454, -125.2830755159759519, 74.00833731765517598 ) ) ;
#11313 = EDGE_CURVE ( 'NONE', #238, #5932, #19135, .T. ) ;
#11314 = CARTESIAN_POINT ( 'NONE',  ( 109.1592201516379674, -0.006536841731962029015, -0.004368284148525239038 ) ) ;
#11315 = CARTESIAN_POINT ( 'NONE',  ( -8.786685647604890903, -53.04920435127188938, -7.199674155858766689 ) ) ;
#11316 = CARTESIAN_POINT ( 'NONE',  ( 10.93730112725977932, -108.9902118373748863, 104.7670965581006755 ) ) ;
#11317 = B_SPLINE_CURVE_WITH_KNOTS ( 'NONE', 3,
 ( #17165, #2168, #5962, #12562, #19189, #8258, #17017, #25815, #3929, #25955 ),
 .UNSPECIFIED., .F., .F.,
 ( 4, 2, 2, 2, 4 ),
 ( 8.299636676276019848E-18, 0.0003346267210630991806, 0.0006692534421261901213, 0.001003880163189280845, 0.001338506884252371786 ),
 .UNSPECIFIED. ) ;
#11318 = CARTESIAN_POINT ( 'NONE',  ( 1.832998868059858122, -117.7096351258393270, 84.86110816369566123 ) ) ;
#11319 = ORIENTED_EDGE ( 'NONE', *, *, #11684, .T. ) ;
#11320 = CARTESIAN_POINT ( 'NONE',  ( -1.019300379054419947, -12.21833869579496579, -44.15350047934394695 ) ) ;
#11321 = CARTESIAN_POINT ( 'NONE',  ( -20.47566338032515887, -28.85746366088576664, -7.708089572830313152 ) ) ;
#11322 = CARTESIAN_POINT ( 'NONE',  ( 1.833206310202323719, -59.70089235435347064, -132.2594754479310950 ) ) ;
#11323 = B_SPLINE_CURVE_WITH_KNOTS ( 'NONE', 3,
 ( #1673, #10207, #3700, #16672 ),
 .UNSPECIFIED., .F., .F.,
 ( 4, 4 ),
 ( 3.798054144356080256E-16, 0.01077107486149828271 ),
 .UNSPECIFIED. ) ;
#11324 = ORIENTED_EDGE ( 'NONE', *, *, #21129, .F. ) ;
#11325 = CARTESIAN_POINT ( 'NONE',  ( 2.430230287190572103, 84.35270093935255886, 118.5711603495684443 ) ) ;
#11326 = VERTEX_POINT ( 'NONE', #1751 ) ;
#11327 = LINE ( 'NONE', #7411, #27610 ) ;
#11328 = CARTESIAN_POINT ( 'NONE',  ( 30.59141879584313628, 2.701465575441479139, -116.1811685142591557 ) ) ;
#11329 = EDGE_LOOP ( 'NONE', ( #20919, #15028, #25000, #19712 ) ) ;
#11330 = CARTESIAN_POINT ( 'NONE',  ( -20.20612092514785019, -10.22177639105880864, -27.77903665678161360 ) ) ;
#11331 = DIRECTION ( 'NONE',  ( -0.7563875759206389882, -0.3556158456312901173, 0.5490129373055266937 ) ) ;
#11332 = CARTESIAN_POINT ( 'NONE',  ( -1.019300379054419947, -42.90269154183439326, -16.06793277091975369 ) ) ;
#11333 = CARTESIAN_POINT ( 'NONE',  ( -1.045287976400365970, 15.59869763335068171, -43.05558670614252037 ) ) ;
#11334 = CARTESIAN_POINT ( 'NONE',  ( 25.98552792386799126, -113.1317367103340388, 1.078856412010440247 ) ) ;
#11335 = EDGE_CURVE ( 'NONE', #6178, #213, #28037, .T. ) ;
#11336 = ORIENTED_EDGE ( 'NONE', *, *, #15225, .T. ) ;
#11337 = CARTESIAN_POINT ( 'NONE',  ( 25.64692232868534560, 0.3267662677151492723, 112.9106972861223426 ) ) ;
#11338 = CARTESIAN_POINT ( 'NONE',  ( -55.24340739397742794, 0.005344433640974572026, -0.008612749836242874699 ) ) ;
#11339 = CARTESIAN_POINT ( 'NONE',  ( -28.41354790283022069, 5.969609727608339966, 22.41474081377994310 ) ) ;
#11340 = VERTEX_POINT ( 'NONE', #1891 ) ;
#11341 = EDGE_CURVE ( 'NONE', #27159, #9343, #20134, .T. ) ;
#11342 = ORIENTED_EDGE ( 'NONE', *, *, #13844, .T. ) ;
#11343 = ORIENTED_EDGE ( 'NONE', *, *, #1046, .F. ) ;
#11344 = CARTESIAN_POINT ( 'NONE',  ( -1.048996300304501972, -43.31387123529967909, 14.87787369922214076 ) ) ;
#11345 = CARTESIAN_POINT ( 'NONE',  ( -55.24340739397742794, -0.007744344507854267548, 0.006539691034608354631 ) ) ;
#11346 = CARTESIAN_POINT ( 'NONE',  ( 25.64708010899964918, 75.59303792846624503, 83.87281825978644179 ) ) ;
#11347 = CARTESIAN_POINT ( 'NONE',  ( -55.24198130335446422, -0.006527480770975599769, 0.006617369590168732142 ) ) ;
#11348 = DIRECTION ( 'NONE',  ( 0.000000000000000000, 0.000000000000000000, -1.000000000000000000 ) ) ;
#11349 = LINE ( 'NONE', #26320, #5589 ) ;
#11350 = CARTESIAN_POINT ( 'NONE',  ( -20.37983603106073716, 1.508851015062576462, -29.73529213200292176 ) ) ;
#11351 = ORIENTED_EDGE ( 'NONE', *, *, #18310, .F. ) ;
#11352 = CARTESIAN_POINT ( 'NONE',  ( 25.70243777736187951, -34.20488708978023595, -107.6443926015133457 ) ) ;
#11353 = CARTESIAN_POINT ( 'NONE',  ( -55.24390624410018802, 0.004572280736703349113, -0.009374879212967143077 ) ) ;
#11354 = CARTESIAN_POINT ( 'NONE',  ( 25.64708010899965629, 11.85684669924970969, 112.2870082086266876 ) ) ;
#11355 = CARTESIAN_POINT ( 'NONE',  ( 25.64670758986456889, -75.18147256661998767, -84.24158725144702942 ) ) ;
#11356 = ORIENTED_EDGE ( 'NONE', *, *, #14655, .T. ) ;
#11357 = CARTESIAN_POINT ( 'NONE',  ( -8.786685647604894456, 7.199674155859698388, 53.04920435127174017 ) ) ;
#11358 = CARTESIAN_POINT ( 'NONE',  ( 1.834118845439484335, 44.67218053242396536, 138.0627591860431380 ) ) ;
#11359 = CARTESIAN_POINT ( 'NONE',  ( 1.833206310202330602, -142.0914673790818483, -29.44113265021077197 ) ) ;
#11360 = ORIENTED_EDGE ( 'NONE', *, *, #7896, .F. ) ;
#11361 = B_SPLINE_CURVE_WITH_KNOTS ( 'NONE', 3,
 ( #21202, #1482, #10292, #2421, #703, #4878, #20129, #15657 ),
 .UNSPECIFIED., .F., .F.,
 ( 4, 2, 2, 4 ),
 ( 6.938893903907228378E-18, 0.0002429588503611281253, 0.0004859177007222493117, 0.0009718354014444792162 ),
 .UNSPECIFIED. ) ;
#11362 = ORIENTED_EDGE ( 'NONE', *, *, #24563, .F. ) ;
#11363 = B_SPLINE_CURVE_WITH_KNOTS ( 'NONE', 3,
 ( #14361, #1818, #5889, #14646, #16952, #3988, #23448, #25880, #14924, #6179 ),
 .UNSPECIFIED., .F., .F.,
 ( 4, 3, 3, 4 ),
 ( 1.040834085586084257E-17, 0.0002669560319015712793, 0.0005492286108966347316, 0.0008315040496093422957 ),
 .UNSPECIFIED. ) ;
#11364 = VERTEX_POINT ( 'NONE', #28228 ) ;
#11365 = CARTESIAN_POINT ( 'NONE',  ( 55.79472521941428198, 53.57698701322279788, -49.22042574086372468 ) ) ;
#11366 = CARTESIAN_POINT ( 'NONE',  ( -4.473127245936434626, -31.51789735524219438, -37.94261489385706909 ) ) ;
#11367 = CARTESIAN_POINT ( 'NONE',  ( -20.57838717382308147, 16.28767523336121315, -25.16001208503110931 ) ) ;
#11368 = VERTEX_POINT ( 'NONE', #5014 ) ;
#11369 = CARTESIAN_POINT ( 'NONE',  ( 25.86096068574578766, 67.25583614083966211, -90.87263912324351622 ) ) ;
#11370 = EDGE_CURVE ( 'NONE', #17492, #22027, #3261, .T. ) ;
#11371 = DIRECTION ( 'NONE',  ( -0.5914120900931443270, -0.4804373588864723210, -0.6476200150380233556 ) ) ;
#11372 = VERTEX_POINT ( 'NONE', #22751 ) ;
#11373 = CARTESIAN_POINT ( 'NONE',  ( -20.57838717382308147, 10.78122205917000365, -27.96569011373090063 ) ) ;
#11374 = EDGE_CURVE ( 'NONE', #21438, #378, #13937, .T. ) ;
#11375 = ORIENTED_EDGE ( 'NONE', *, *, #12823, .T. ) ;
#11376 = LINE ( 'NONE', #22179, #1035 ) ;
#11377 = CARTESIAN_POINT ( 'NONE',  ( 2.108393763691207123, 13.91282116576980421, 144.6252321290181442 ) ) ;
#11378 = CARTESIAN_POINT ( 'NONE',  ( 2.430230287190589422, -142.0258656395023991, 31.67257033707456770 ) ) ;
#11379 = EDGE_CURVE ( 'NONE', #1317, #26336, #18246, .T. ) ;
#11380 = CARTESIAN_POINT ( 'NONE',  ( 10.93730112725971360, 26.59437931460756488, 148.8212007290661916 ) ) ;
#11381 = B_SPLINE_CURVE_WITH_KNOTS ( 'NONE', 3,
 ( #6099, #10281, #23089, #3775, #10127, #9987, #12686, #19038 ),
 .UNSPECIFIED., .F., .F.,
 ( 4, 2, 2, 4 ),
 ( 0.000000000000000000, 0.002761524886576651946, 0.005523049773153303893, 0.01104609954630660952 ),
 .UNSPECIFIED. ) ;
#11382 = CARTESIAN_POINT ( 'NONE',  ( 2.433796855181205476, 86.69855925934130880, -116.8607839509047892 ) ) ;
#11383 = CARTESIAN_POINT ( 'NONE',  ( -55.25297051322618813, 0.01483298743815085648, 0.001818774723749092123 ) ) ;
#11384 = CARTESIAN_POINT ( 'NONE',  ( -20.38016308990357217, -7.753479680700753107, 28.74660391518353109 ) ) ;
#11385 = CARTESIAN_POINT ( 'NONE',  ( 25.64681081121879203, -66.03065707438999254, 91.59071981940550700 ) ) ;
#11386 = CARTESIAN_POINT ( 'NONE',  ( -55.24390624410018802, -0.004896917417127438256, -0.009209468562451287102 ) ) ;
#11387 = CARTESIAN_POINT ( 'NONE',  ( -55.24271866751342941, 0.001425019990779444407, 0.009388511352200054269 ) ) ;
#11388 = ORIENTED_EDGE ( 'NONE', *, *, #5697, .F. ) ;
#11389 = ORIENTED_EDGE ( 'NONE', *, *, #12539, .T. ) ;
#11390 = CARTESIAN_POINT ( 'NONE',  ( 25.81918753295378721, 24.41190151229255534, 110.3582118788977766 ) ) ;
#11391 = CARTESIAN_POINT ( 'NONE',  ( 109.1586059443104944, 0.005438258427231131183, 0.004524147648825582735 ) ) ;
#11392 = B_SPLINE_CURVE_WITH_KNOTS ( 'NONE', 3,
 ( #16932, #3541, #27293, #14053, #21249, #19097, #25295, #14185, #23287, #14481 ),
 .UNSPECIFIED., .F., .F.,
 ( 4, 2, 2, 2, 4 ),
 ( 7.961322465290408245E-18, 0.0003346267210630986927, 0.0006692534421261893624, 0.001003880163189280195, 0.001338506884252370919 ),
 .UNSPECIFIED. ) ;
#11393 = ORIENTED_EDGE ( 'NONE', *, *, #8471, .F. ) ;
#11394 = ORIENTED_EDGE ( 'NONE', *, *, #15584, .F. ) ;
#11395 = ORIENTED_EDGE ( 'NONE', *, *, #26036, .F. ) ;
#11396 = CARTESIAN_POINT ( 'NONE',  ( 26.11404676487257603, 83.38016054979783576, 76.59696442953219275 ) ) ;
#11397 = CARTESIAN_POINT ( 'NONE',  ( 25.64681081121879203, -110.5293738517610080, 23.06870491922286348 ) ) ;
#11398 = B_SPLINE_CURVE_WITH_KNOTS ( 'NONE', 3,
 ( #3031, #9645, #9949, #20578, #18711, #27187, #7502, #1157 ),
 .UNSPECIFIED., .F., .F.,
 ( 4, 2, 2, 4 ),
 ( 2.299172327962918193E-16, 0.002761568181852868970, 0.005523136363705508090, 0.01104627272741078720 ),
 .UNSPECIFIED. ) ;
#11399 = CARTESIAN_POINT ( 'NONE',  ( -55.24340739397742084, 0.01010924026184365637, 0.0007387096945736542795 ) ) ;
#11400 = EDGE_CURVE ( 'NONE', #19738, #24861, #16365, .T. ) ;
#11401 = CARTESIAN_POINT ( 'NONE',  ( -1.019300379054419725, 2.023851374323315078, 45.76814864815086992 ) ) ;
#11402 = EDGE_CURVE ( 'NONE', #8934, #13041, #5094, .T. ) ;
#11403 = DIRECTION ( 'NONE',  ( 0.7637818620346800147, -0.6451161201712182214, -0.02150485345384170119 ) ) ;
#11404 = CARTESIAN_POINT ( 'NONE',  ( -1.050230346682668126, 43.55729751025884156, 14.15335421912537583 ) ) ;
#11405 = DIRECTION ( 'NONE',  ( 0.000000000000000000, 0.000000000000000000, 1.000000000000000000 ) ) ;
#11406 = CARTESIAN_POINT ( 'NONE',  ( -1.259920593601965066, 43.01175804832032412, 16.33409644610508238 ) ) ;
#11407 = CARTESIAN_POINT ( 'NONE',  ( 1.833206310202334821, -132.8652722326994535, -58.34025049825082476 ) ) ;
#11408 = CARTESIAN_POINT ( 'NONE',  ( 1.832998868059858122, -117.7096351258382043, -84.86110816369723864 ) ) ;
#11409 = VECTOR ( 'NONE', #22122, 1000.000000000000000 ) ;
#11410 = CARTESIAN_POINT ( 'NONE',  ( 28.43349137099831836, 116.8557575815934655, -42.22940898499091844 ) ) ;
#11411 = CARTESIAN_POINT ( 'NONE',  ( -4.473127245936434626, -3.196405119334147837, -49.22197550883366546 ) ) ;
#11412 = CLOSED_SHELL ( 'NONE', ( #18988, #4481, #4909, #9196, #2652, #27083, #25487, #8066, #17953, #17198, #17275, #23689, #27729, #12067, #9591, #19062, #18859, #10450, #10370, #7670, #18160, #24519, #16206, #18188, #13240, #7595, #27199, #24444, #26818, #17475, #17991, #20549, #26673, #1970, #380, #9863, #2969, #10983, #1750, #9814, #25632, #14070, #10455, #19655, #4821, #23045, #17000, #21549, #64, #880, #19747, #14747, #4545, #658, #25886, #19303, #23205, #5831, #27220, #4215, #7564, #9404, #4823, #14977, #15102, #13904, #4117, #8261, #22647, #18017, #16997, #3584, #2066, #912, #8820, #6314, #17096, #3160, #11805, #4170, #20902, #23332, #8877, #11468, #16792, #21605, #15542, #7240, #21670, #25227, #11639, #24322, #1938, #2527, #21353, #13980, #17707, #6414, #20926, #14366, #12116, #23716, #1694, #11306, #16211, #19393, #16780, #8974, #17462, #14974, #20759, #16652, #19260, #4254, #11049, #6613, #13337, #23003, #5791, #20830, #2833, #17549, #9101, #22870, #26372, #19946, #17205, #5217, #15452, #5530, #25054, #2227 ) ) ;
#11413 = CARTESIAN_POINT ( 'NONE',  ( 1.833809397773815686, -117.5007887865414489, 85.14934054436442068 ) ) ;
#11414 = ORIENTED_EDGE ( 'NONE', *, *, #7633, .F. ) ;
#11415 =( BOUNDED_SURFACE ( )  B_SPLINE_SURFACE ( 3, 1, ( 
 ( #17452, #24107 ),
 ( #11137, #17874 ),
 ( #4370, #13143 ),
 ( #26658, #6976 ) ),
 .UNSPECIFIED., .F., .F., .F. ) 
 B_SPLINE_SURFACE_WITH_KNOTS ( ( 4, 4 ),
 ( 2, 2 ),
 ( 0.000000000000000000, 1.000000000000000000 ),
 ( 0.000000000000000000, 1.000000000000000000 ),
 .UNSPECIFIED. ) 
 GEOMETRIC_REPRESENTATION_ITEM ( )  RATIONAL_B_SPLINE_SURFACE ( (
 ( 1.000000000000000000, 1.000000000000000000),
 ( 0.9934239774497837239, 0.8357310067453919133),
 ( 0.9934239774497837239, 0.8357310067453919133),
 ( 1.000000000000000000, 1.000000000000000000) ) ) 
 REPRESENTATION_ITEM ( '' )  SURFACE ( )  );
#11416 = LINE ( 'NONE', #4938, #18846 ) ;
#11417 = CARTESIAN_POINT ( 'NONE',  ( 8.186469777910582835, 113.2805152945354195, 97.33125097303739892 ) ) ;
#11418 = CARTESIAN_POINT ( 'NONE',  ( 25.64700659047694842, 45.71714758798376010, 103.2418925369174758 ) ) ;
#11419 = CARTESIAN_POINT ( 'NONE',  ( 26.11404676487257603, 98.61392875273440950, -55.62948129436141897 ) ) ;
#11420 = FACE_OUTER_BOUND ( 'NONE', #9279, .T. ) ;
#11421 = DIRECTION ( 'NONE',  ( 0.5914120900931444380, -0.6045864222316781333, 0.5335794202785162366 ) ) ;
#11422 = VERTEX_POINT ( 'NONE', #20420 ) ;
#11423 = CARTESIAN_POINT ( 'NONE',  ( 10.93730112725971360, 36.23586118136525158, 146.7718404940643211 ) ) ;
#11424 = ORIENTED_EDGE ( 'NONE', *, *, #3394, .F. ) ;
#11425 = CARTESIAN_POINT ( 'NONE',  ( 25.98107933586711482, 103.7920584735901599, -45.01656174308481440 ) ) ;
#11426 = CARTESIAN_POINT ( 'NONE',  ( 25.69398547355842766, 12.54367966928045064, 112.2438548322122926 ) ) ;
#11427 = ORIENTED_EDGE ( 'NONE', *, *, #14912, .F. ) ;
#11428 = LINE ( 'NONE', #9131, #19477 ) ;
#11429 =( BOUNDED_SURFACE ( )  B_SPLINE_SURFACE ( 3, 1, ( 
 ( #26634, #6945 ),
 ( #15694, #14109 ),
 ( #25080, #18433 ),
 ( #3185, #22928 ) ),
 .UNSPECIFIED., .F., .F., .F. ) 
 B_SPLINE_SURFACE_WITH_KNOTS ( ( 4, 4 ),
 ( 2, 2 ),
 ( 0.000000000000000000, 1.000000000000000000 ),
 ( 0.000000000000000000, 1.000000000000000000 ),
 .UNSPECIFIED. ) 
 GEOMETRIC_REPRESENTATION_ITEM ( )  RATIONAL_B_SPLINE_SURFACE ( (
 ( 1.000000000000000000, 1.000000000000000000),
 ( 0.9593753223639863714, 0.9995975284513187731),
 ( 0.9593753223639863714, 0.9995975284513187731),
 ( 1.000000000000000000, 1.000000000000000000) ) ) 
 REPRESENTATION_ITEM ( '' )  SURFACE ( )  );
#11430 = ORIENTED_EDGE ( 'NONE', *, *, #20632, .F. ) ;
#11431 = CARTESIAN_POINT ( 'NONE',  ( 26.11404676487257603, -97.48350837663569735, -57.58742681967552102 ) ) ;
#11432 = ORIENTED_EDGE ( 'NONE', *, *, #25822, .F. ) ;
#11433 = VECTOR ( 'NONE', #4194, 999.9999999999998863 ) ;
#11434 = CARTESIAN_POINT ( 'NONE',  ( 5.340103579038268933, 13.12023871299920330, -146.8647350263016733 ) ) ;
#11435 = EDGE_CURVE ( 'NONE', #7273, #21979, #27692, .T. ) ;
#11436 = ADVANCED_FACE ( 'NONE', ( #4340 ), #12359, .F. ) ;
#11437 = CARTESIAN_POINT ( 'NONE',  ( 109.1586900883932856, -0.002810909342002450555, 0.006561743627145253353 ) ) ;
#11438 = EDGE_CURVE ( 'NONE', #17576, #11749, #7334, .T. ) ;
#11439 = CARTESIAN_POINT ( 'NONE',  ( -1.050229599974470185, -13.90955673306158147, -43.63650726458059381 ) ) ;
#11440 = LINE ( 'NONE', #11728, #10154 ) ;
#11441 = CARTESIAN_POINT ( 'NONE',  ( 109.1586900883932856, 0.003656351050324883108, -0.006130969560693678121 ) ) ;
#11442 = CARTESIAN_POINT ( 'NONE',  ( 2.433796855181233454, -98.43889364293788447, -107.1581411821795626 ) ) ;
#11443 = FACE_OUTER_BOUND ( 'NONE', #7876, .T. ) ;
#11444 = CARTESIAN_POINT ( 'NONE',  ( 25.87036335909427009, -33.99475147239086681, 107.8283083010002912 ) ) ;
#11445 = ORIENTED_EDGE ( 'NONE', *, *, #23419, .F. ) ;
#11446 = LINE ( 'NONE', #18336, #75 ) ;
#11447 = CARTESIAN_POINT ( 'NONE',  ( -1.050231094221210526, -26.71409683968590798, 37.20185272688488709 ) ) ;
#11448 = B_SPLINE_CURVE_WITH_KNOTS ( 'NONE', 3,
 ( #23028, #3712, #3149, #18551, #25613, #16684, #11929, #7480 ),
 .UNSPECIFIED., .F., .F.,
 ( 4, 2, 2, 4 ),
 ( 0.000000000000000000, 0.0002429588503611160636, 0.0004859177007222321271, 0.0009718354014444642542 ),
 .UNSPECIFIED. ) ;
#11449 = CARTESIAN_POINT ( 'NONE',  ( 26.28373643307402219, -122.5382646256987158, -35.44121223574987312 ) ) ;
#11450 = EDGE_CURVE ( 'NONE', #12565, #2306, #15334, .T. ) ;
#11451 = CARTESIAN_POINT ( 'NONE',  ( -7.711401346138374358, 47.70038152767087780, -21.83927363365046048 ) ) ;
#11452 = CARTESIAN_POINT ( 'NONE',  ( 10.93730112725994097, -51.37919228020192008, -142.1801301103790536 ) ) ;
#11453 = CARTESIAN_POINT ( 'NONE',  ( 25.64681081121879203, 110.5293738517611501, -23.06870491922213873 ) ) ;
#11454 = CARTESIAN_POINT ( 'NONE',  ( 28.43349137099851021, 76.27296957774109387, 98.08682467580786124 ) ) ;
#11455 = ORIENTED_EDGE ( 'NONE', *, *, #20041, .T. ) ;
#11456 = CARTESIAN_POINT ( 'NONE',  ( 32.73300124599732186, 0.000000000000000000, 0.000000000000000000 ) ) ;
#11457 = ORIENTED_EDGE ( 'NONE', *, *, #22501, .F. ) ;
#11458 = CARTESIAN_POINT ( 'NONE',  ( 28.43349137099828638, -123.0821667346708068, 17.01091693849698672 ) ) ;
#11459 =( BOUNDED_SURFACE ( )  B_SPLINE_SURFACE ( 3, 1, ( 
 ( #7474, #23175 ),
 ( #8055, #25737 ),
 ( #23307, #16525 ),
 ( #12618, #27311 ) ),
 .UNSPECIFIED., .F., .F., .F. ) 
 B_SPLINE_SURFACE_WITH_KNOTS ( ( 4, 4 ),
 ( 2, 2 ),
 ( 0.000000000000000000, 1.000000000000000000 ),
 ( 0.000000000000000000, 1.000000000000000000 ),
 .UNSPECIFIED. ) 
 GEOMETRIC_REPRESENTATION_ITEM ( )  RATIONAL_B_SPLINE_SURFACE ( (
 ( 1.000000000000000000, 1.000000000000000000),
 ( 0.9956975270656954757, 0.8568959468854893125),
 ( 0.9956975270656954757, 0.8568959468854893125),
 ( 1.000000000000000000, 1.000000000000000000) ) ) 
 REPRESENTATION_ITEM ( '' )  SURFACE ( )  );
#11460 = EDGE_CURVE ( 'NONE', #28478, #16899, #11931, .T. ) ;
#11461 = CARTESIAN_POINT ( 'NONE',  ( 1.833691583653564328, -97.36155720551542458, 107.5990239011822922 ) ) ;
#11462 = ORIENTED_EDGE ( 'NONE', *, *, #14371, .T. ) ;
#11463 = CARTESIAN_POINT ( 'NONE',  ( 25.64708010899966339, -112.9112661935489683, 0.05470523945829951218 ) ) ;
#11464 = ADVANCED_FACE ( 'NONE', ( #6513 ), #15274, .F. ) ;
#11465 = ORIENTED_EDGE ( 'NONE', *, *, #6145, .T. ) ;
#11466 = CARTESIAN_POINT ( 'NONE',  ( 9.884929003653608603, -119.2676479132367433, -91.84919534722065748 ) ) ;
#11467 = ORIENTED_EDGE ( 'NONE', *, *, #20635, .T. ) ;
#11468 = ADVANCED_FACE ( 'NONE', ( #6659 ), #1513, .F. ) ;
#11469 = CARTESIAN_POINT ( 'NONE',  ( 28.37644542392837010, -109.6517504963493650, 58.62516076110009777 ) ) ;
#11470 = CARTESIAN_POINT ( 'NONE',  ( 25.64681081121879203, 107.2555980796245905, -35.28660243342437752 ) ) ;
#11471 = CARTESIAN_POINT ( 'NONE',  ( 32.73300124599738581, -115.8010721414081985, -20.69176323058746902 ) ) ;
#11472 = CARTESIAN_POINT ( 'NONE',  ( 26.04756280548353686, -113.1727782765313890, 1.110889087302109113 ) ) ;
#11473 = ORIENTED_EDGE ( 'NONE', *, *, #26871, .F. ) ;
#11474 = CARTESIAN_POINT ( 'NONE',  ( 10.93730112725932635, 0.000000000000000000, 0.000000000000000000 ) ) ;
#11475 = CARTESIAN_POINT ( 'NONE',  ( 2.433796855181233454, -96.28145139437756939, 109.1007109081222666 ) ) ;
#11476 = CARTESIAN_POINT ( 'NONE',  ( -24.53239521893645048, 29.54733954334105661, -16.68574937150984638 ) ) ;
#11477 = ORIENTED_EDGE ( 'NONE', *, *, #13997, .F. ) ;
#11478 = ORIENTED_EDGE ( 'NONE', *, *, #24590, .T. ) ;
#11479 = DIRECTION ( 'NONE',  ( 0.5914120900931444380, 0.008020494143001851220, -0.8063295922669342364 ) ) ;
#11480 = CARTESIAN_POINT ( 'NONE',  ( -20.47566262905010248, -10.72601569609877536, 27.87687924095557435 ) ) ;
#11481 = CARTESIAN_POINT ( 'NONE',  ( 25.64700659047696973, 75.38309044531882819, 84.06149911284467180 ) ) ;
#11482 = CARTESIAN_POINT ( 'NONE',  ( 2.433796855181205476, -96.28145139437610567, -109.1007109081235882 ) ) ;
#11483 = CARTESIAN_POINT ( 'NONE',  ( -7.733045908741323693, -52.15131830128827062, -5.980865481987962085 ) ) ;
#11484 = LINE ( 'NONE', #15949, #9832 ) ;
#11485 = VERTEX_POINT ( 'NONE', #16835 ) ;
#11486 = CARTESIAN_POINT ( 'NONE',  ( 109.1592201516379674, -0.007780772729118872952, -0.001127733110579658832 ) ) ;
#11487 = CARTESIAN_POINT ( 'NONE',  ( 2.430230287190581429, 43.58368230469393723, 138.8342928068221624 ) ) ;
#11488 = CARTESIAN_POINT ( 'NONE',  ( 2.108393763691185807, -57.92353377304199569, -133.2474712570800364 ) ) ;
#11489 = CARTESIAN_POINT ( 'NONE',  ( -24.53237795827032031, 14.09663893005633284, 30.86653739599985968 ) ) ;
#11490 = LINE ( 'NONE', #4588, #20164 ) ;
#11491 = AXIS2_PLACEMENT_3D ( 'NONE', #5059, #11696, #3198 ) ;
#11492 = ORIENTED_EDGE ( 'NONE', *, *, #26407, .F. ) ;
#11493 = CARTESIAN_POINT ( 'NONE',  ( 9.884929003653626367, -35.39789245780224292, -146.3148513795970587 ) ) ;
#11494 = EDGE_CURVE ( 'NONE', #6343, #17039, #16596, .T. ) ;
#11495 = VERTEX_POINT ( 'NONE', #5602 ) ;
#11496 = CARTESIAN_POINT ( 'NONE',  ( -20.57838717382308147, 29.92853265176831812, -1.611677988432464126 ) ) ;
#11497 = CARTESIAN_POINT ( 'NONE',  ( 1.833485406944043827, 144.2578170162062747, 15.69895494453433393 ) ) ;
#11498 = ORIENTED_EDGE ( 'NONE', *, *, #6111, .T. ) ;
#11499 = EDGE_CURVE ( 'NONE', #13959, #27119, #17734, .T. ) ;
#11500 = B_SPLINE_CURVE_WITH_KNOTS ( 'NONE', 3,
 ( #8300, #17628, #17069, #6157, #15036, #26412, #25994, #12603 ),
 .UNSPECIFIED., .F., .F.,
 ( 4, 2, 2, 4 ),
 ( 3.469446951953614189E-18, 0.0002429592666046667042, 0.0004859185332093299389, 0.0009718370664186788514 ),
 .UNSPECIFIED. ) ;
#11501 = ORIENTED_EDGE ( 'NONE', *, *, #26774, .T. ) ;
#11502 = ORIENTED_EDGE ( 'NONE', *, *, #1689, .T. ) ;
#11503 = EDGE_CURVE ( 'NONE', #20579, #3264, #8134, .T. ) ;
#11504 =( BOUNDED_SURFACE ( )  B_SPLINE_SURFACE ( 3, 1, ( 
 ( #18805, #12322 ),
 ( #1383, #10192 ),
 ( #18953, #27733 ),
 ( #25583, #8038 ) ),
 .UNSPECIFIED., .F., .F., .F. ) 
 B_SPLINE_SURFACE_WITH_KNOTS ( ( 4, 4 ),
 ( 2, 2 ),
 ( 0.000000000000000000, 1.000000000000000000 ),
 ( 0.000000000000000000, 1.000000000000000000 ),
 .UNSPECIFIED. ) 
 GEOMETRIC_REPRESENTATION_ITEM ( )  RATIONAL_B_SPLINE_SURFACE ( (
 ( 1.000000000000000000, 1.000000000000000000),
 ( 0.7789835883360576307, 0.9689951854195403280),
 ( 0.7789835883360576307, 0.9689951854195403280),
 ( 1.000000000000000000, 1.000000000000000000) ) ) 
 REPRESENTATION_ITEM ( '' )  SURFACE ( )  );
#11505 = DIRECTION ( 'NONE',  ( 0.7637818620346801257, -0.5092696688508668856, -0.3965875333584823470 ) ) ;
#11506 = ADVANCED_FACE ( 'NONE', ( #12491 ), #15108, .F. ) ;
#11507 = CARTESIAN_POINT ( 'NONE',  ( 119.2224693531408803, 90.00000000000005684, 19.99999999999997513 ) ) ;
#11508 = AXIS2_PLACEMENT_3D ( 'NONE', #21540, #12617, #3852 ) ;
#11509 = B_SPLINE_CURVE_WITH_KNOTS ( 'NONE', 3,
 ( #20558, #23026, #13787, #5445, #26887, #9488, #18242 ),
 .UNSPECIFIED., .F., .F.,
 ( 4, 3, 4 ),
 ( 0.000000000000000000, 0.02398743853561337985, 0.04000277880656215312 ),
 .UNSPECIFIED. ) ;
#11510 = CARTESIAN_POINT ( 'NONE',  ( 10.93730112725932635, 0.000000000000000000, 0.000000000000000000 ) ) ;
#11511 = CARTESIAN_POINT ( 'NONE',  ( -20.20612091757420359, 23.26073043121660433, 18.30568244821352408 ) ) ;
#11512 = ORIENTED_EDGE ( 'NONE', *, *, #15184, .T. ) ;
#11513 = CARTESIAN_POINT ( 'NONE',  ( 25.73574536432412074, 67.05280231777622646, -90.91878692681962093 ) ) ;
#11514 = CONICAL_SURFACE ( 'NONE', #3263, 34.60786435723138510, 0.8559913436420825139 ) ;
#11515 = CARTESIAN_POINT ( 'NONE',  ( -55.24390624410018802, -0.009209468562450790971, 0.004896917417127758312 ) ) ;
#11516 = CARTESIAN_POINT ( 'NONE',  ( 2.433796855181205476, -142.6247129145649808, 28.83182736670489987 ) ) ;
#11517 = ORIENTED_EDGE ( 'NONE', *, *, #11866, .F. ) ;
#11518 = CIRCLE ( 'NONE', #10595, 34.60786435723138510 ) ;
#11519 = ORIENTED_EDGE ( 'NONE', *, *, #6490, .T. ) ;
#11520 = CARTESIAN_POINT ( 'NONE',  ( -1.583189561560252701, -16.68617981233673220, 43.29471907393757846 ) ) ;
#11521 = CARTESIAN_POINT ( 'NONE',  ( 1.893872463202068923, 14.22435552398011005, 144.4512189534318054 ) ) ;
#11522 = CARTESIAN_POINT ( 'NONE',  ( -15.02187109954782507, 41.75590530176335591, 20.12219089991046772 ) ) ;
#11523 = CARTESIAN_POINT ( 'NONE',  ( 109.1592201516379674, -0.007051465909551689858, -0.003476928926125464302 ) ) ;
#11524 = CARTESIAN_POINT ( 'NONE',  ( 26.28373643307409679, -67.34887744616709426, -108.3320567927997047 ) ) ;
#11525 = CARTESIAN_POINT ( 'NONE',  ( -2.904412668506658246, -40.16685646686189415, 25.64203923793618145 ) ) ;
#11526 = CARTESIAN_POINT ( 'NONE',  ( 1.833838850093451933, 15.16810397409781253, 144.3148362521193064 ) ) ;
#11527 = FACE_OUTER_BOUND ( 'NONE', #11227, .T. ) ;
#11528 = CARTESIAN_POINT ( 'NONE',  ( 109.1778270068192853, -0.0006237116683805482738, -0.009293669915253103403 ) ) ;
#11529 = ORIENTED_EDGE ( 'NONE', *, *, #8098, .F. ) ;
#11530 = CARTESIAN_POINT ( 'NONE',  ( -20.20700224038492010, -8.199606986804138131, 28.44216453106544762 ) ) ;
#11531 = CONICAL_SURFACE ( 'NONE', #17943, 34.60786435723138510, 0.8559913436420825139 ) ;
#11532 = CARTESIAN_POINT ( 'NONE',  ( 109.1586900883932856, 0.006479576224403787998, 0.002995460350180830216 ) ) ;
#11533 = ORIENTED_EDGE ( 'NONE', *, *, #18488, .F. ) ;
#11534 = ADVANCED_FACE ( 'NONE', ( #9929 ), #10367, .F. ) ;
#11535 = AXIS2_PLACEMENT_3D ( 'NONE', #28008, #14911, #21105 ) ;
#11536 = VERTEX_POINT ( 'NONE', #10360 ) ;
#11537 = ORIENTED_EDGE ( 'NONE', *, *, #5500, .T. ) ;
#11538 = VECTOR ( 'NONE', #10750, 1000.000000000000114 ) ;
#11539 = DIRECTION ( 'NONE',  ( 1.000000000000000000, -6.938893903907226837E-18, 1.734723475976806709E-18 ) ) ;
#11540 = CARTESIAN_POINT ( 'NONE',  ( -1.539763995773681060, -2.469814354917172494, 46.22267697748607418 ) ) ;
#11541 = EDGE_CURVE ( 'NONE', #26952, #15878, #21277, .T. ) ;
#11542 = FACE_OUTER_BOUND ( 'NONE', #15451, .T. ) ;
#11543 = B_SPLINE_CURVE_WITH_KNOTS ( 'NONE', 3,
 ( #6541, #10445, #23700, #3951 ),
 .UNSPECIFIED., .F., .F.,
 ( 4, 4 ),
 ( 3.419165934695819025E-16, 0.01077107486149840761 ),
 .UNSPECIFIED. ) ;
#11544 = CARTESIAN_POINT ( 'NONE',  ( -9.156249394959713683, -48.78605533024723684, 24.29252099376542517 ) ) ;
#11545 =( BOUNDED_SURFACE ( )  B_SPLINE_SURFACE ( 3, 1, ( 
 ( #27316, #2713 ),
 ( #16093, #7629 ),
 ( #16383, #9191 ),
 ( #11486, #2862 ) ),
 .UNSPECIFIED., .F., .F., .F. ) 
 B_SPLINE_SURFACE_WITH_KNOTS ( ( 4, 4 ),
 ( 2, 2 ),
 ( 0.000000000000000000, 1.000000000000000000 ),
 ( 0.000000000000000000, 1.000000000000000000 ),
 .UNSPECIFIED. ) 
 GEOMETRIC_REPRESENTATION_ITEM ( )  RATIONAL_B_SPLINE_SURFACE ( (
 ( 1.000000000000000000, 1.000000000000000000),
 ( 0.6386103224230316178, 0.9954351624131538845),
 ( 0.6386103224230316178, 0.9954351624131538845),
 ( 1.000000000000000000, 1.000000000000000000) ) ) 
 REPRESENTATION_ITEM ( '' )  SURFACE ( )  );
#11546 = CARTESIAN_POINT ( 'NONE',  ( -25.21435515916043713, -31.17620025257576799, 15.02493970636179377 ) ) ;
#11547 = DIRECTION ( 'NONE',  ( 0.000000000000000000, 0.000000000000000000, 1.000000000000000000 ) ) ;
#11548 = CARTESIAN_POINT ( 'NONE',  ( -8.786685647604896232, 52.67761315067299677, 9.545808661480061019 ) ) ;
#11549 = CARTESIAN_POINT ( 'NONE',  ( -1.583189561560252701, 2.490696082059875138, -46.33203782964461936 ) ) ;
#11550 = AXIS2_PLACEMENT_3D ( 'NONE', #12086, #11653, #1144 ) ;
#11551 = CARTESIAN_POINT ( 'NONE',  ( 16.75465622695641343, -48.33695624543422298, 133.7599617830026943 ) ) ;
#11552 = AXIS2_PLACEMENT_3D ( 'NONE', #8748, #17515, #15350 ) ;
#11553 = CARTESIAN_POINT ( 'NONE',  ( -7.711401346138397450, -47.70038152767074990, 21.83927363365083707 ) ) ;
#11554 = FACE_OUTER_BOUND ( 'NONE', #5583, .T. ) ;
#11555 = DIRECTION ( 'NONE',  ( 0.000000000000000000, 5.223019709708233256E-21, -1.000000000000000000 ) ) ;
#11556 = CONICAL_SURFACE ( 'NONE', #7923, 34.60786435723138510, 0.8559913436420825139 ) ;
#11557 = ORIENTED_EDGE ( 'NONE', *, *, #555, .T. ) ;
#11559 = DIRECTION ( 'NONE',  ( -0.7563875759206387661, -0.5078650950445656731, 0.4122509917856767570 ) ) ;
#11558 = CARTESIAN_POINT ( 'NONE',  ( -55.24390624410018802, -0.004572280736701530256, -0.009374879212970928244 ) ) ;
#11560 = CARTESIAN_POINT ( 'NONE',  ( -1.056502255334265339, 0.5104472526220019679, -45.80535052436397336 ) ) ;
#11561 = LINE ( 'NONE', #26950, #25923 ) ;
#11562 = CARTESIAN_POINT ( 'NONE',  ( 30.59141879584279167, 66.10404588653790370, 95.58042137919471770 ) ) ;
#11563 = CARTESIAN_POINT ( 'NONE',  ( -1.113427685306992876, 16.03057832159213092, 42.96952363574816758 ) ) ;
#11564 = ORIENTED_EDGE ( 'NONE', *, *, #27027, .F. ) ;
#11565 = CARTESIAN_POINT ( 'NONE',  ( 13.36082413113063083, 152.7944199136427414, -6.345145185218573403 ) ) ;
#11566 = ORIENTED_EDGE ( 'NONE', *, *, #20372, .T. ) ;
#11567 = CARTESIAN_POINT ( 'NONE',  ( -20.20612092514784308, -29.57813644637189299, 1.137292630518367265 ) ) ;
#11568 = CARTESIAN_POINT ( 'NONE',  ( 26.04756280548354397, 12.93458011762476012, 112.4366864265127930 ) ) ;
#11569 = ORIENTED_EDGE ( 'NONE', *, *, #3997, .T. ) ;
#11570 = EDGE_CURVE ( 'NONE', #14056, #19926, #13605, .T. ) ;
#11571 = CARTESIAN_POINT ( 'NONE',  ( -25.21435515916043713, -4.655591116594118617, 34.29329011225960500 ) ) ;
#11572 = ORIENTED_EDGE ( 'NONE', *, *, #13183, .F. ) ;
#11573 = CARTESIAN_POINT ( 'NONE',  ( -16.86833981943421890, -43.51541671545732015, -7.884812276281936150 ) ) ;
#11574 = EDGE_CURVE ( 'NONE', #24022, #15878, #5048, .T. ) ;
#11575 = ADVANCED_FACE ( 'NONE', ( #13051 ), #19169, .F. ) ;
#11576 = ORIENTED_EDGE ( 'NONE', *, *, #7985, .F. ) ;
#11577 = FACE_OUTER_BOUND ( 'NONE', #22910, .T. ) ;
#11578 = VECTOR ( 'NONE', #19682, 1000.000000000000114 ) ;
#11579 = DIRECTION ( 'NONE',  ( -1.000000000000000000, -0.000000000000000000, -0.000000000000000000 ) ) ;
#11580 = EDGE_CURVE ( 'NONE', #20671, #11368, #22927, .T. ) ;
#11581 = DIRECTION ( 'NONE',  ( 0.000000000000000000, 0.000000000000000000, 1.000000000000000000 ) ) ;
#11582 =( BOUNDED_SURFACE ( )  B_SPLINE_SURFACE ( 3, 1, ( 
 ( #13780, #20971 ),
 ( #16375, #16522 ),
 ( #16232, #25169 ),
 ( #20842, #20687 ) ),
 .UNSPECIFIED., .F., .F., .F. ) 
 B_SPLINE_SURFACE_WITH_KNOTS ( ( 4, 4 ),
 ( 2, 2 ),
 ( 0.000000000000000000, 1.000000000000000000 ),
 ( 0.000000000000000000, 1.000000000000000000 ),
 .UNSPECIFIED. ) 
 GEOMETRIC_REPRESENTATION_ITEM ( )  RATIONAL_B_SPLINE_SURFACE ( (
 ( 1.000000000000000000, 1.000000000000000000),
 ( 0.6386103224230316178, 0.9954351624131538845),
 ( 0.6386103224230316178, 0.9954351624131538845),
 ( 1.000000000000000000, 1.000000000000000000) ) ) 
 REPRESENTATION_ITEM ( '' )  SURFACE ( )  );
#11583 = CARTESIAN_POINT ( 'NONE',  ( 1.832998868059890096, -96.70023740551195601, 108.1944082009154187 ) ) ;
#11584 = CARTESIAN_POINT ( 'NONE',  ( -1.583189561560255143, -25.21827308671260326, -38.94740041318284796 ) ) ;
#11585 = B_SPLINE_CURVE_WITH_KNOTS ( 'NONE', 3,
 ( #10144, #6112, #19318, #19467, #28236, #10977, #15411, #26220 ),
 .UNSPECIFIED., .F., .F.,
 ( 4, 2, 2, 4 ),
 ( 9.813077866773594792E-18, 0.0002429592666046790912, 0.0004859185332093483704, 0.0009718370664186869829 ),
 .UNSPECIFIED. ) ;
#11586 = CARTESIAN_POINT ( 'NONE',  ( -20.57838717382308147, -16.28767523336102130, 25.16001208503123365 ) ) ;
#11587 = CARTESIAN_POINT ( 'NONE',  ( -1.049819825607587465, 26.50610175068268859, -37.34982882986852815 ) ) ;
#11588 = CARTESIAN_POINT ( 'NONE',  ( 10.93730112725977932, -104.7670965581018123, 108.9902118373738062 ) ) ;
#11589 = VERTEX_POINT ( 'NONE', #19531 ) ;
#11590 = CARTESIAN_POINT ( 'NONE',  ( 109.1586059443104944, 0.007058870754606109445, -0.0004635842312890220179 ) ) ;
#11592 = CARTESIAN_POINT ( 'NONE',  ( 25.73574536432417759, 45.21157800100309032, 103.5288236655397185 ) ) ;
#11591 = CARTESIAN_POINT ( 'NONE',  ( -25.21435515916042647, 15.02493970636146692, -31.17620025257592786 ) ) ;
#11593 = CARTESIAN_POINT ( 'NONE',  ( 25.98107933586712903, -84.80123094405263373, 74.88680433646213430 ) ) ;
#11594 = CARTESIAN_POINT ( 'NONE',  ( 1.833206310202332379, 85.89457578512813996, 116.9567751109822069 ) ) ;
#11595 = ORIENTED_EDGE ( 'NONE', *, *, #11499, .T. ) ;
#11597 =( BOUNDED_SURFACE ( )  B_SPLINE_SURFACE ( 3, 1, ( 
 ( #2005, #15234 ),
 ( #10521, #21876 ),
 ( #15377, #22008 ),
 ( #10938, #16989 ) ),
 .UNSPECIFIED., .F., .F., .F. ) 
 B_SPLINE_SURFACE_WITH_KNOTS ( ( 4, 4 ),
 ( 2, 2 ),
 ( 0.000000000000000000, 1.000000000000000000 ),
 ( 0.000000000000000000, 1.000000000000000000 ),
 .UNSPECIFIED. ) 
 GEOMETRIC_REPRESENTATION_ITEM ( )  RATIONAL_B_SPLINE_SURFACE ( (
 ( 1.000000000000000000, 1.000000000000000000),
 ( 0.6386103224230302855, 0.9954351624131538845),
 ( 0.6386103224230302855, 0.9954351624131538845),
 ( 1.000000000000000000, 1.000000000000000000) ) ) 
 REPRESENTATION_ITEM ( '' )  SURFACE ( )  );
#11596 = CIRCLE ( 'NONE', #26301, 117.6351876552689504 ) ;
#11598 = ADVANCED_FACE ( 'NONE', ( #1964 ), #19388, .T. ) ;
#11599 = VERTEX_POINT ( 'NONE', #25883 ) ;
#11600 = CARTESIAN_POINT ( 'NONE',  ( 1.831572820252008738, 126.1609924456739975, -71.69925593429677235 ) ) ;
#11601 = VECTOR ( 'NONE', #26084, 999.9999999999998863 ) ;
#11602 = CARTESIAN_POINT ( 'NONE',  ( 16.75465622695654133, -53.58152542127593421, -131.7467602971414919 ) ) ;
#11603 = CARTESIAN_POINT ( 'NONE',  ( -55.24390624410018802, -0.009209468562450790971, 0.004896917417127758312 ) ) ;
#11604 = ORIENTED_EDGE ( 'NONE', *, *, #13757, .T. ) ;
#11605 = CARTESIAN_POINT ( 'NONE',  ( 10.93730112726003156, 84.82621002473607064, -125.1380233598471960 ) ) ;
#11607 = VERTEX_POINT ( 'NONE', #6180 ) ;
#11606 = ADVANCED_FACE ( 'NONE', ( #26151 ), #12900, .T. ) ;
#11608 = CARTESIAN_POINT ( 'NONE',  ( -1.045287976400365970, 1.530335034934747318, 45.76855895860941814 ) ) ;
#11609 = B_SPLINE_CURVE_WITH_KNOTS ( 'NONE', 3,
 ( #13085, #10252, #19014, #22151, #2266, #20122, #22300, #11210, #4438, #26738 ),
 .UNSPECIFIED., .F., .F.,
 ( 4, 3, 3, 4 ),
 ( 1.387778780781445676E-17, 0.0002669560319015615215, 0.0005492286108966200949, 0.0008315040496093287431 ),
 .UNSPECIFIED. ) ;
#11610 = B_SPLINE_CURVE_WITH_KNOTS ( 'NONE', 3,
 ( #21276, #18835, #20982, #14511 ),
 .UNSPECIFIED., .F., .F.,
 ( 4, 4 ),
 ( 3.314527865495573890E-16, 0.01077107486149804158 ),
 .UNSPECIFIED. ) ;
#11611 = EDGE_LOOP ( 'NONE', ( #24083, #25854, #7222, #16353 ) ) ;
#11612 = CARTESIAN_POINT ( 'NONE',  ( -20.47566262905009538, -27.87687924095555658, -10.72601569609885708 ) ) ;
#11613 = ORIENTED_EDGE ( 'NONE', *, *, #4787, .F. ) ;
#11614 = VECTOR ( 'NONE', #23645, 999.9999999999998863 ) ;
#11615 = CARTESIAN_POINT ( 'NONE',  ( 1.832998868059890096, 138.1720401012266848, 44.33343224355281365 ) ) ;
#11616 = ORIENTED_EDGE ( 'NONE', *, *, #21968, .F. ) ;
#11617 = SHAPE_REPRESENTATION_RELATIONSHIP ( 'NONE' , 'NONE' ,  #22271, #2743 ) ;
#11618 = VECTOR ( 'NONE', #23737, 1000.000000000000227 ) ;
#11619 = CARTESIAN_POINT ( 'NONE',  ( -20.20700224038492721, 0.9908225410478516126, -29.58392382092673145 ) ) ;
#11620 = VECTOR ( 'NONE', #23344, 1000.000000000000114 ) ;
#11621 = CARTESIAN_POINT ( 'NONE',  ( 26.11404676487259024, 108.0249973236467582, 33.91085499298413453 ) ) ;
#11622 = CARTESIAN_POINT ( 'NONE',  ( 1.833838850855463498, -125.7132320915354029, 72.47782099564605574 ) ) ;
#11623 = ORIENTED_EDGE ( 'NONE', *, *, #24948, .T. ) ;
#11624 = CARTESIAN_POINT ( 'NONE',  ( 109.1624594426973118, 0.01318243916934995832, 0.009004164758064592267 ) ) ;
#11625 = CARTESIAN_POINT ( 'NONE',  ( 25.81918753295378011, 34.03777907512061773, -107.7789657594971402 ) ) ;
#11626 = CARTESIAN_POINT ( 'NONE',  ( 10.93730112725990011, -128.3908183996585990, -79.81734490846054086 ) ) ;
#11627 = VERTEX_POINT ( 'NONE', #28433 ) ;
#11628 = EDGE_CURVE ( 'NONE', #17548, #9151, #25675, .T. ) ;
#11629 = ORIENTED_EDGE ( 'NONE', *, *, #12768, .T. ) ;
#11630 = VERTEX_POINT ( 'NONE', #10769 ) ;
#11631 = CARTESIAN_POINT ( 'NONE',  ( -16.86833981943424376, -19.19877306373879122, -39.83928801320582380 ) ) ;
#11632 = CARTESIAN_POINT ( 'NONE',  ( 55.79472521941426777, -59.28412330436329825, 42.17269936297619637 ) ) ;
#11634 = CARTESIAN_POINT ( 'NONE',  ( -9.156249394959713683, -24.29252099376526530, -48.78605533024730789 ) ) ;
#11633 = CARTESIAN_POINT ( 'NONE',  ( -20.57838717382308147, -18.89542499756482741, 23.26537097894125594 ) ) ;
#11635 = CARTESIAN_POINT ( 'NONE',  ( -55.24198130335446422, -0.008310594958152726572, 0.004163123460802491127 ) ) ;
#11636 = VECTOR ( 'NONE', #1495, 1000.000000000000000 ) ;
#11637 = CARTESIAN_POINT ( 'NONE',  ( 25.64681081121879203, -84.18689316040098447, 75.24277141833462679 ) ) ;
#11638 = CARTESIAN_POINT ( 'NONE',  ( -4.162674018437145129, -47.46216648493545875, 11.82104147411610207 ) ) ;
#11639 = ADVANCED_FACE ( 'NONE', ( #24284 ), #27658, .F. ) ;
#11640 = VERTEX_POINT ( 'NONE', #15339 ) ;
#11641 = DIRECTION ( 'NONE',  ( 1.000000000000000000, -6.938893903907226837E-18, 1.734723475976806709E-18 ) ) ;
#11642 = CARTESIAN_POINT ( 'NONE',  ( -1.539760825549692402, -16.63252404870386059, -43.19716078875433851 ) ) ;
#11643 =( BOUNDED_SURFACE ( )  B_SPLINE_SURFACE ( 3, 1, ( 
 ( #18413, #27191 ),
 ( #22769, #20439 ),
 ( #9512, #15837 ),
 ( #16116, #4898 ) ),
 .UNSPECIFIED., .F., .F., .F. ) 
 B_SPLINE_SURFACE_WITH_KNOTS ( ( 4, 4 ),
 ( 2, 2 ),
 ( 0.000000000000000000, 1.000000000000000000 ),
 ( 0.000000000000000000, 1.000000000000000000 ),
 .UNSPECIFIED. ) 
 GEOMETRIC_REPRESENTATION_ITEM ( )  RATIONAL_B_SPLINE_SURFACE ( (
 ( 1.000000000000000000, 1.000000000000000000),
 ( 0.9956975270656954757, 0.8568959468854893125),
 ( 0.9956975270656954757, 0.8568959468854893125),
 ( 1.000000000000000000, 1.000000000000000000) ) ) 
 REPRESENTATION_ITEM ( '' )  SURFACE ( )  );
#11644 = LINE ( 'NONE', #20417, #4181 ) ;
#11645 = ADVANCED_FACE ( 'NONE', ( #19254 ), #8165, .F. ) ;
#11646 = CARTESIAN_POINT ( 'NONE',  ( 109.1586900883932856, 0.004701023939945712764, -0.005371970278528660422 ) ) ;
#11647 = CARTESIAN_POINT ( 'NONE',  ( 1.833485406944057594, 142.0485807715645876, 29.64752363041592531 ) ) ;
#11648 = ORIENTED_EDGE ( 'NONE', *, *, #23883, .F. ) ;
#11649 = CARTESIAN_POINT ( 'NONE',  ( 2.063896406836609909, -137.7380992975105301, 46.16709813092576553 ) ) ;
#11650 = VECTOR ( 'NONE', #6320, 999.9999999999998863 ) ;
#11651 = VECTOR ( 'NONE', #10100, 1000.000000000000000 ) ;
#11652 = ORIENTED_EDGE ( 'NONE', *, *, #9631, .T. ) ;
#11653 = DIRECTION ( 'NONE',  ( 1.000000000000000000, -0.000000000000000000, -0.000000000000000000 ) ) ;
#11654 = CARTESIAN_POINT ( 'NONE',  ( 109.1592201516379674, 0.006536841731953405704, -0.004368284148529032879 ) ) ;
#11655 = ORIENTED_EDGE ( 'NONE', *, *, #6235, .T. ) ;
#11656 = B_SPLINE_CURVE_WITH_KNOTS ( 'NONE', 3,
 ( #18894, #19037, #21036, #8522, #21332, #21472 ),
 .UNSPECIFIED., .F., .F.,
 ( 4, 2, 4 ),
 ( 1.110764993427085326E-17, 0.0006311636237756819466, 0.001262327247551352834 ),
 .UNSPECIFIED. ) ;
#11657 = VERTEX_POINT ( 'NONE', #93 ) ;
#11658 = VERTEX_POINT ( 'NONE', #12901 ) ;
#11659 = CARTESIAN_POINT ( 'NONE',  ( 109.1592201516379674, -0.007748443302134891582, -0.001331853079201365982 ) ) ;
#11660 = CARTESIAN_POINT ( 'NONE',  ( -20.20612092514784308, 16.46550332780526915, -24.59769888281538996 ) ) ;
#11661 = CARTESIAN_POINT ( 'NONE',  ( 109.1586900883932856, 0.004277182003227222341, 0.005715190711481739176 ) ) ;
#11662 = CARTESIAN_POINT ( 'NONE',  ( 16.75465622695645962, 19.47041796022427462, -140.8868039942615553 ) ) ;
#11663 = CARTESIAN_POINT ( 'NONE',  ( -20.20612091757425333, -24.59769958242376120, 16.46550228026422502 ) ) ;
#11664 = CARTESIAN_POINT ( 'NONE',  ( 25.64692872815577473, -103.2799065540887256, 45.63107645358293496 ) ) ;
#11665 = AXIS2_PLACEMENT_3D ( 'NONE', #1111, #1243, #22722 ) ;
#11666 = LINE ( 'NONE', #863, #26947 ) ;
#11667 = ORIENTED_EDGE ( 'NONE', *, *, #22307, .T. ) ;
#11668 = ADVANCED_FACE ( 'NONE', ( #8467 ), #5031, .F. ) ;
#11669 = ORIENTED_EDGE ( 'NONE', *, *, #13326, .F. ) ;
#11670 = CARTESIAN_POINT ( 'NONE',  ( -55.24728320129491266, 0.01137345571547128398, 0.009072670231978179414 ) ) ;
#11671 = EDGE_CURVE ( 'NONE', #2917, #12674, #11225, .T. ) ;
#11672 = CARTESIAN_POINT ( 'NONE',  ( 25.64699802086724389, -46.14225289916239348, -103.0525896353906319 ) ) ;
#11673 = CARTESIAN_POINT ( 'NONE',  ( 109.1586059443104944, 0.007068659269322301146, 0.0002768082440195569175 ) ) ;
#11674 = CARTESIAN_POINT ( 'NONE',  ( 2.430230287190592531, 144.5585181921888420, -16.65331920325590787 ) ) ;
#11675 = DIRECTION ( 'NONE',  ( 0.7563875759206389882, -0.03500244528122105347, 0.6531865459554679898 ) ) ;
#11676 = B_SPLINE_CURVE_WITH_KNOTS ( 'NONE', 3,
 ( #8849, #17610, #6695, #10729, #4508, #13287 ),
 .UNSPECIFIED., .F., .F.,
 ( 4, 2, 4 ),
 ( 9.263427422397553349E-18, 0.0006311636237756821635, 0.001262327247551355220 ),
 .UNSPECIFIED. ) ;
#11677 = ORIENTED_EDGE ( 'NONE', *, *, #4093, .T. ) ;
#11678 = CARTESIAN_POINT ( 'NONE',  ( -1.259920593601978833, 44.39818421957814820, -12.06711544331578168 ) ) ;
#11679 = CARTESIAN_POINT ( 'NONE',  ( -1.049819078601898825, -0.5100232645223283789, -45.79653735114490587 ) ) ;
#11680 = EDGE_CURVE ( 'NONE', #7646, #10229, #13973, .T. ) ;
#11681 = CARTESIAN_POINT ( 'NONE',  ( -1.619063947482197729, -35.99532424477401094, -29.22875152547743838 ) ) ;
#11682 = CARTESIAN_POINT ( 'NONE',  ( 6.224689322667630975, 146.9579047224769397, 18.02516478984192716 ) ) ;
#11683 = CARTESIAN_POINT ( 'NONE',  ( -25.21435515916025594, 1.749597353048488237E-16, -4.373993382621220594E-17 ) ) ;
#11684 = EDGE_CURVE ( 'NONE', #16498, #12003, #23931, .T. ) ;
#11685 = ORIENTED_EDGE ( 'NONE', *, *, #3257, .F. ) ;
#11686 = ORIENTED_EDGE ( 'NONE', *, *, #492, .T. ) ;
#11687 = FACE_OUTER_BOUND ( 'NONE', #18910, .T. ) ;
#11688 = ORIENTED_EDGE ( 'NONE', *, *, #11460, .T. ) ;
#11689 = B_SPLINE_CURVE_WITH_KNOTS ( 'NONE', 3,
 ( #6110, #12833, #4345, #8535, #1757, #17433, #14714, #10553 ),
 .UNSPECIFIED., .F., .F.,
 ( 4, 2, 2, 4 ),
 ( 1.250926888277100303E-17, 0.0002429592666046839430, 0.0004859185332093553635, 0.0009718370664186946808 ),
 .UNSPECIFIED. ) ;
#11690 =( BOUNDED_SURFACE ( )  B_SPLINE_SURFACE ( 3, 1, ( 
 ( #3619, #27937 ),
 ( #12395, #27371 ),
 ( #25664, #14696 ),
 ( #16440, #25223 ) ),
 .UNSPECIFIED., .F., .F., .F. ) 
 B_SPLINE_SURFACE_WITH_KNOTS ( ( 4, 4 ),
 ( 2, 2 ),
 ( 0.000000000000000000, 1.000000000000000000 ),
 ( 0.000000000000000000, 1.000000000000000000 ),
 .UNSPECIFIED. ) 
 GEOMETRIC_REPRESENTATION_ITEM ( )  RATIONAL_B_SPLINE_SURFACE ( (
 ( 1.000000000000000000, 1.000000000000000000),
 ( 0.7789835883360578528, 0.9689951854195403280),
 ( 0.7789835883360578528, 0.9689951854195403280),
 ( 1.000000000000000000, 1.000000000000000000) ) ) 
 REPRESENTATION_ITEM ( '' )  SURFACE ( )  );
#11691 = VERTEX_POINT ( 'NONE', #4975 ) ;
#11692 = ORIENTED_EDGE ( 'NONE', *, *, #4648, .F. ) ;
#11693 = CARTESIAN_POINT ( 'NONE',  ( 26.11404676487257603, -113.2169081140373947, -1.130420376098323576 ) ) ;
#11694 = B_SPLINE_CURVE_WITH_KNOTS ( 'NONE', 3,
 ( #17067, #3836, #24128, #17481, #17206, #1795, #26267 ),
 .UNSPECIFIED., .F., .F.,
 ( 4, 3, 4 ),
 ( 0.000000000000000000, 0.02398743853561358108, 0.04000277880656216700 ),
 .UNSPECIFIED. ) ;
#11695 = EDGE_CURVE ( 'NONE', #27740, #6545, #24726, .T. ) ;
#11696 = DIRECTION ( 'NONE',  ( -1.000000000000000000, -0.000000000000000000, -0.000000000000000000 ) ) ;
#11697 = CARTESIAN_POINT ( 'NONE',  ( -55.24390624410018802, 0.007503127514282199352, -0.007245494385991655198 ) ) ;
#11698 = PRODUCT_DEFINITION_CONTEXT ( 'detailed design', #28110, 'design' ) ;
#11699 = CARTESIAN_POINT ( 'NONE',  ( 109.1587776205901861, 0.006661366261223553367, -0.003057017121600569438 ) ) ;
#11700 = CARTESIAN_POINT ( 'NONE',  ( 25.64681081121879203, 107.2555980796241215, 35.28660243342585545 ) ) ;
#11701 = CARTESIAN_POINT ( 'NONE',  ( -1.619063947482197729, 2.489035965910801895, 46.30105812165545842 ) ) ;
#11702 = CARTESIAN_POINT ( 'NONE',  ( 25.70243777736189728, -35.59945151684150488, 107.1912711514953713 ) ) ;
#11703 = CARTESIAN_POINT ( 'NONE',  ( 25.73574536432413851, 112.9674920590232858, 0.8061344836373177669 ) ) ;
#11704 = CARTESIAN_POINT ( 'NONE',  ( 28.43349137099834323, 4.052139611198435354, 124.1860347533534963 ) ) ;
#11705 = EDGE_CURVE ( 'NONE', #12310, #384, #14630, .T. ) ;
#11706 = CARTESIAN_POINT ( 'NONE',  ( -16.86833981943425442, 20.94590537750608661, -38.94907963570727816 ) ) ;
#11707 = CARTESIAN_POINT ( 'NONE',  ( 5.340103556456496925, -117.9209211572679976, -88.52145167812714988 ) ) ;
#11708 = CARTESIAN_POINT ( 'NONE',  ( -1.619063947482201282, 11.94059994246159384, -44.80407745103787676 ) ) ;
#11709 = EDGE_CURVE ( 'NONE', #22192, #26713, #10233, .T. ) ;
#11710 = CARTESIAN_POINT ( 'NONE',  ( -23.79248802219731118, -28.61009539422396131, -16.82188324679470881 ) ) ;
#11711 = CARTESIAN_POINT ( 'NONE',  ( 26.11404676487259024, 76.59696442953192275, 83.38016054979810576 ) ) ;
#11712 = CARTESIAN_POINT ( 'NONE',  ( -1.049817751779871688, -37.35030165458155693, 26.50542916749608580 ) ) ;
#11713 = CARTESIAN_POINT ( 'NONE',  ( 109.1721716018069657, -0.003746085893652680628, -0.01665253177026228618 ) ) ;
#11714 = CARTESIAN_POINT ( 'NONE',  ( -8.786685647604890903, -9.545808661480982948, -52.67761315067281913 ) ) ;
#11715 = ORIENTED_EDGE ( 'NONE', *, *, #10538, .F. ) ;
#11716 = LINE ( 'NONE', #7263, #3782 ) ;
#11717 = ORIENTED_EDGE ( 'NONE', *, *, #19743, .F. ) ;
#11718 = DIRECTION ( 'NONE',  ( 0.000000000000000000, 5.223019709707975211E-21, -1.000000000000000000 ) ) ;
#11719 = CARTESIAN_POINT ( 'NONE',  ( -1.583189561560255143, 36.01941156322830295, 29.24830400313125267 ) ) ;
#11720 = ORIENTED_EDGE ( 'NONE', *, *, #15901, .F. ) ;
#11721 = ORIENTED_EDGE ( 'NONE', *, *, #18532, .F. ) ;
#11722 =( BOUNDED_SURFACE ( )  B_SPLINE_SURFACE ( 3, 1, ( 
 ( #19844, #26323 ),
 ( #11072, #6479 ),
 ( #271, #8501 ),
 ( #2268, #17539 ) ),
 .UNSPECIFIED., .F., .F., .F. ) 
 B_SPLINE_SURFACE_WITH_KNOTS ( ( 4, 4 ),
 ( 2, 2 ),
 ( 0.000000000000000000, 1.000000000000000000 ),
 ( 0.000000000000000000, 1.000000000000000000 ),
 .UNSPECIFIED. ) 
 GEOMETRIC_REPRESENTATION_ITEM ( )  RATIONAL_B_SPLINE_SURFACE ( (
 ( 1.000000000000000000, 1.000000000000000000),
 ( 0.9593753223639863714, 0.9995975284513187731),
 ( 0.9593753223639863714, 0.9995975284513187731),
 ( 1.000000000000000000, 1.000000000000000000) ) ) 
 REPRESENTATION_ITEM ( '' )  SURFACE ( )  );
#11723 = ORIENTED_EDGE ( 'NONE', *, *, #12677, .T. ) ;
#11724 = B_SPLINE_CURVE_WITH_KNOTS ( 'NONE', 3,
 ( #2962, #22396, #9298, #24844, #26691, #4685, #15906, #22254 ),
 .UNSPECIFIED., .F., .F.,
 ( 4, 2, 2, 4 ),
 ( 6.938893903907228378E-18, 0.0002429588503611240595, 0.0004859177007222411802, 0.0009718354014444684826 ),
 .UNSPECIFIED. ) ;
#11725 = CARTESIAN_POINT ( 'NONE',  ( -1.031422197589711987, 12.69107518035501414, -44.01264471863851213 ) ) ;
#11726 = CARTESIAN_POINT ( 'NONE',  ( 28.37644542392841984, -123.1691345231581494, -17.02293047611490096 ) ) ;
#11727 = CARTESIAN_POINT ( 'NONE',  ( 109.1586900883932856, 0.005833932871487514972, -0.004113747441000937220 ) ) ;
#11728 = CARTESIAN_POINT ( 'NONE',  ( -28.41354790283022069, 19.47297445639567925, 12.60397206714810814 ) ) ;
#11729 = CARTESIAN_POINT ( 'NONE',  ( -55.24271866751342941, -0.008488649505342596782, -0.004256484107795601053 ) ) ;
#11730 = DIRECTION ( 'NONE',  ( 0.000000000000000000, 0.000000000000000000, 1.000000000000000000 ) ) ;
#11731 = CARTESIAN_POINT ( 'NONE',  ( 109.1586900883932856, -0.002995460350180851900, 0.006479576224403776723 ) ) ;
#11732 = CARTESIAN_POINT ( 'NONE',  ( 5.340103556456367251, 84.79482753886546220, 120.6284720803327986 ) ) ;
#11733 = ADVANCED_FACE ( 'NONE', ( #2976 ), #16840, .F. ) ;
#11734 = DIRECTION ( 'NONE',  ( 0.5946245182733607137, 0.6977579871484563823, -0.3994439555666204344 ) ) ;
#11736 = CARTESIAN_POINT ( 'NONE',  ( 13.36082413113063083, -25.56125765253554860, 150.7747251079861428 ) ) ;
#11735 = CARTESIAN_POINT ( 'NONE',  ( 1.833485406944043827, 84.86072343962567288, 117.7091014914953320 ) ) ;
#11737 = CARTESIAN_POINT ( 'NONE',  ( -1.044556982611271279, -1.643392503293034768, -45.76404732357878657 ) ) ;
#11739 = ORIENTED_EDGE ( 'NONE', *, *, #8930, .F. ) ;
#11738 = EDGE_CURVE ( 'NONE', #20356, #14085, #24278, .T. ) ;
#11740 = ORIENTED_EDGE ( 'NONE', *, *, #26954, .F. ) ;
#11741 = CARTESIAN_POINT ( 'NONE',  ( -1.619063947482197729, 11.94059994246222622, 44.80407745103770623 ) ) ;
#11743 = CARTESIAN_POINT ( 'NONE',  ( 109.1587776205901577, -0.004842060007774085656, -0.005502145856754143277 ) ) ;
#11742 = DIRECTION ( 'NONE',  ( -0.5914120900931443270, 0.07630783613001886068, -0.8027508043202528087 ) ) ;
#11744 = ADVANCED_FACE ( 'NONE', ( #23411 ), #14021, .F. ) ;
#11745 = CARTESIAN_POINT ( 'NONE',  ( -2.265401668238148591, -46.93990709177548837, -2.645701981445641504 ) ) ;
#11746 = CARTESIAN_POINT ( 'NONE',  ( 1.832998868059890096, -45.34898734666140285, 137.8420662456168770 ) ) ;
#11747 = CARTESIAN_POINT ( 'NONE',  ( 2.263178113027038307, 138.7064940342184514, -43.59477710889581914 ) ) ;
#11748 = CARTESIAN_POINT ( 'NONE',  ( -1.155001620486255431, -35.88346938217574689, -28.62773628245655644 ) ) ;
#11749 = VERTEX_POINT ( 'NONE', #27279 ) ;
#11750 = CARTESIAN_POINT ( 'NONE',  ( 30.58324630866347604, 120.8793175557613324, -3.944468862008090326 ) ) ;
#11751 = CARTESIAN_POINT ( 'NONE',  ( 109.1592201516379674, 0.007856029051018016685, 0.0003082430541935266563 ) ) ;
#11752 = CARTESIAN_POINT ( 'NONE',  ( 13.36082413113063083, -84.67697637120498655, 127.3428651193245287 ) ) ;
#11753 = ORIENTED_EDGE ( 'NONE', *, *, #27078, .T. ) ;
#11754 = CARTESIAN_POINT ( 'NONE',  ( -7.078251931573400491, -47.71415099571819951, -20.86696228105206075 ) ) ;
#11755 = VERTEX_POINT ( 'NONE', #18940 ) ;
#11756 = CARTESIAN_POINT ( 'NONE',  ( 32.73300124599732186, 0.000000000000000000, 0.000000000000000000 ) ) ;
#11757 = B_SPLINE_CURVE_WITH_KNOTS ( 'NONE', 3,
 ( #28481, #6499, #20002, #13370 ),
 .UNSPECIFIED., .F., .F.,
 ( 4, 4 ),
 ( 3.511136132061045056E-16, 0.01077107486149755586 ),
 .UNSPECIFIED. ) ;
#11758 = LINE ( 'NONE', #18512, #17948 ) ;
#11759 = VERTEX_POINT ( 'NONE', #25281 ) ;
#11761 = ADVANCED_FACE ( 'NONE', ( #14609 ), #14799, .F. ) ;
#11760 = FACE_OUTER_BOUND ( 'NONE', #18032, .T. ) ;
#11762 = ORIENTED_EDGE ( 'NONE', *, *, #17276, .F. ) ;
#11763 =( BOUNDED_SURFACE ( )  B_SPLINE_SURFACE ( 3, 1, ( 
 ( #11875, #3655 ),
 ( #18775, #12164 ),
 ( #931, #3381 ),
 ( #14305, #20930 ) ),
 .UNSPECIFIED., .F., .F., .F. ) 
 B_SPLINE_SURFACE_WITH_KNOTS ( ( 4, 4 ),
 ( 2, 2 ),
 ( 0.000000000000000000, 1.000000000000000000 ),
 ( 0.000000000000000000, 1.000000000000000000 ),
 .UNSPECIFIED. ) 
 GEOMETRIC_REPRESENTATION_ITEM ( )  RATIONAL_B_SPLINE_SURFACE ( (
 ( 1.000000000000000000, 1.000000000000000000),
 ( 0.9956975270656954757, 0.8568959468854893125),
 ( 0.9956975270656954757, 0.8568959468854893125),
 ( 1.000000000000000000, 1.000000000000000000) ) ) 
 REPRESENTATION_ITEM ( '' )  SURFACE ( )  );
#11764 = CARTESIAN_POINT ( 'NONE',  ( 8.186469777910781787, -71.65198614410293487, 131.0413692044509162 ) ) ;
#11765 = B_SPLINE_CURVE_WITH_KNOTS ( 'NONE', 3,
 ( #1267, #18389, #22892, #27173, #1136, #25178 ),
 .UNSPECIFIED., .F., .F.,
 ( 4, 2, 4 ),
 ( 0.000000000000000000, 0.0004335184443140220763, 0.0008670368886280441527 ),
 .UNSPECIFIED. ) ;
#11766 = ORIENTED_EDGE ( 'NONE', *, *, #290, .T. ) ;
#11767 = DIRECTION ( 'NONE',  ( 1.110440577024103043E-16, -0.2896204557599233453, 0.9571415734390679164 ) ) ;
#11768 = EDGE_CURVE ( 'NONE', #19215, #5961, #17026, .T. ) ;
#11769 = LINE ( 'NONE', #13764, #6958 ) ;
#11770 = DIRECTION ( 'NONE',  ( 0.000000000000000000, -1.000000000000000000, 0.000000000000000000 ) ) ;
#11771 = CARTESIAN_POINT ( 'NONE',  ( -1.619063947482201282, 16.67502769180561728, -43.26576862488438735 ) ) ;
#11772 = DIRECTION ( 'NONE',  ( -1.000000000000000000, -0.000000000000000000, -0.000000000000000000 ) ) ;
#11773 = EDGE_CURVE ( 'NONE', #21319, #2536, #6741, .T. ) ;
#11774 = VERTEX_POINT ( 'NONE', #12037 ) ;
#11775 =( BOUNDED_SURFACE ( )  B_SPLINE_SURFACE ( 3, 1, ( 
 ( #9889, #10328 ),
 ( #21087, #5996 ),
 ( #18653, #8287 ),
 ( #12312, #10035 ) ),
 .UNSPECIFIED., .F., .F., .F. ) 
 B_SPLINE_SURFACE_WITH_KNOTS ( ( 4, 4 ),
 ( 2, 2 ),
 ( 0.000000000000000000, 1.000000000000000000 ),
 ( 0.000000000000000000, 1.000000000000000000 ),
 .UNSPECIFIED. ) 
 GEOMETRIC_REPRESENTATION_ITEM ( )  RATIONAL_B_SPLINE_SURFACE ( (
 ( 1.000000000000000000, 1.000000000000000000),
 ( 0.9956975270656955868, 0.8568959468854907557),
 ( 0.9956975270656955868, 0.8568959468854907557),
 ( 1.000000000000000000, 1.000000000000000000) ) ) 
 REPRESENTATION_ITEM ( '' )  SURFACE ( )  );
#11776 = EDGE_CURVE ( 'NONE', #7508, #976, #14467, .T. ) ;
#11777 = CARTESIAN_POINT ( 'NONE',  ( 8.186469829614228644, -34.43598812953204202, 145.3272524103320222 ) ) ;
#11778 = CARTESIAN_POINT ( 'NONE',  ( 1.833485406944043827, 72.09189602597706426, 125.9346397303438039 ) ) ;
#11779 = CARTESIAN_POINT ( 'NONE',  ( 25.81918753295377300, 98.34688456803397116, 55.70247894228205610 ) ) ;
#11780 = EDGE_LOOP ( 'NONE', ( #17183, #2688, #27864, #22916 ) ) ;
#11781 = ORIENTED_EDGE ( 'NONE', *, *, #25291, .F. ) ;
#11782 = ORIENTED_EDGE ( 'NONE', *, *, #20539, .T. ) ;
#11783 = CARTESIAN_POINT ( 'NONE',  ( -25.21435515916025594, 1.749597353048488237E-16, -4.373993382621220594E-17 ) ) ;
#11784 = CARTESIAN_POINT ( 'NONE',  ( -20.57838717382308147, -10.78122205916981358, 27.96569011373096814 ) ) ;
#11785 = CARTESIAN_POINT ( 'NONE',  ( -12.82751273423877869, -48.43568301531143305, 6.573887447703340214 ) ) ;
#11786 = CARTESIAN_POINT ( 'NONE',  ( 109.1586900883932856, 0.005236795036860546551, -0.004851151255037378096 ) ) ;
#11787 = CARTESIAN_POINT ( 'NONE',  ( 2.433796855181233454, 145.5024947199069913, -1.451562450950139249 ) ) ;
#11788 = LINE ( 'NONE', #5442, #8377 ) ;
#11789 = CARTESIAN_POINT ( 'NONE',  ( -55.24340739397742084, 0.01010924026184365637, 0.0007387096945736542795 ) ) ;
#11790 = VERTEX_POINT ( 'NONE', #12177 ) ;
#11791 = CARTESIAN_POINT ( 'NONE',  ( -20.20700224038492721, 28.44216453106536946, -8.199606986804427677 ) ) ;
#11792 = CARTESIAN_POINT ( 'NONE',  ( -1.058473599757830286, -15.81436910992550438, -42.99101666105224240 ) ) ;
#11793 = PLANE ( 'NONE',  #25345 ) ;
#11794 = CARTESIAN_POINT ( 'NONE',  ( 109.1778270068192853, 0.009293669915260186279, 0.0006237116683871661354 ) ) ;
#11795 = CARTESIAN_POINT ( 'NONE',  ( -25.21435515916025594, 1.749597353048488237E-16, -4.373993382621220594E-17 ) ) ;
#11796 = CARTESIAN_POINT ( 'NONE',  ( 25.87036335909425588, -84.67915015758804032, -74.91347493818344105 ) ) ;
#11797 = CARTESIAN_POINT ( 'NONE',  ( 6.224689322667647851, -33.28770499679229999, -144.2687111683198964 ) ) ;
#11798 = CARTESIAN_POINT ( 'NONE',  ( -21.41427618760448581, 7.777551129310475098, 29.81030852927058206 ) ) ;
#11799 = CARTESIAN_POINT ( 'NONE',  ( 109.1586900883932856, -0.003481399864218472865, 0.006231977675084978893 ) ) ;
#11800 = ORIENTED_EDGE ( 'NONE', *, *, #2500, .F. ) ;
#11801 = ORIENTED_EDGE ( 'NONE', *, *, #19981, .T. ) ;
#11802 = EDGE_LOOP ( 'NONE', ( #17420, #22523, #19733, #4513 ) ) ;
#11803 = CARTESIAN_POINT ( 'NONE',  ( -1.048172774974307053, -45.78636862970790133, 1.020161070261597303 ) ) ;
#11804 = CARTESIAN_POINT ( 'NONE',  ( 25.64692232868535626, -23.79507962493545747, -110.3753891203788982 ) ) ;
#11805 = ADVANCED_FACE ( 'NONE', ( #20811 ), #15884, .F. ) ;
#11806 = CARTESIAN_POINT ( 'NONE',  ( -55.24390624410018802, 0.004572280736702236288, 0.009374879212970765180 ) ) ;
#11807 = ADVANCED_FACE ( 'NONE', ( #21082 ), #23652, .F. ) ;
#11808 = DIRECTION ( 'NONE',  ( 0.000000000000000000, 5.223019709708190374E-21, -1.000000000000000000 ) ) ;
#11809 = CARTESIAN_POINT ( 'NONE',  ( 0.000000000000000000, 0.000000000000000000, 0.000000000000000000 ) ) ;
#11810 = ORIENTED_EDGE ( 'NONE', *, *, #12158, .F. ) ;
#11811 = CARTESIAN_POINT ( 'NONE',  ( 26.28373643307403995, 108.3320567928000173, -67.34887744616673899 ) ) ;
#11812 = CARTESIAN_POINT ( 'NONE',  ( 25.64699802086724745, -103.0525896353904898, 46.14225289916271322 ) ) ;
#11813 = DIRECTION ( 'NONE',  ( -0.7637818620346800147, -0.5345501402766327237, -0.3617919495470695579 ) ) ;
#11814 = ORIENTED_EDGE ( 'NONE', *, *, #25016, .F. ) ;
#11815 =( BOUNDED_SURFACE ( )  B_SPLINE_SURFACE ( 3, 1, ( 
 ( #11731, #7861 ),
 ( #2959, #27261 ),
 ( #5390, #18926 ),
 ( #22831, #13881 ) ),
 .UNSPECIFIED., .F., .F., .F. ) 
 B_SPLINE_SURFACE_WITH_KNOTS ( ( 4, 4 ),
 ( 2, 2 ),
 ( 0.000000000000000000, 1.000000000000000000 ),
 ( 0.000000000000000000, 1.000000000000000000 ),
 .UNSPECIFIED. ) 
 GEOMETRIC_REPRESENTATION_ITEM ( )  RATIONAL_B_SPLINE_SURFACE ( (
 ( 1.000000000000000000, 1.000000000000000000),
 ( 0.9956975270656955868, 0.8568959468854907557),
 ( 0.9956975270656955868, 0.8568959468854907557),
 ( 1.000000000000000000, 1.000000000000000000) ) ) 
 REPRESENTATION_ITEM ( '' )  SURFACE ( )  );
#11816 = EDGE_LOOP ( 'NONE', ( #4310, #13955, #21732, #18892 ) ) ;
#11817 = FACE_OUTER_BOUND ( 'NONE', #10925, .T. ) ;
#11818 = CARTESIAN_POINT ( 'NONE',  ( -1.049819825607596124, -36.75053263699369666, 27.33096219556280815 ) ) ;
#11819 = CARTESIAN_POINT ( 'NONE',  ( -6.588769196390758864, 51.10255870850473769, 4.956336548259831609 ) ) ;
#11820 = CARTESIAN_POINT ( 'NONE',  ( 9.884929003653626367, 149.2134106160918634, -19.90991253123092974 ) ) ;
#11821 = CARTESIAN_POINT ( 'NONE',  ( 32.73300124599737160, -113.0038235389604466, 32.68291970228198551 ) ) ;
#11822 = PLANE ( 'NONE',  #26345 ) ;
#11823 = CARTESIAN_POINT ( 'NONE',  ( 2.430230287190589422, 142.6294793592097960, 28.83279105684476207 ) ) ;
#11824 = VERTEX_POINT ( 'NONE', #3956 ) ;
#11825 = CARTESIAN_POINT ( 'NONE',  ( -55.24198130335446422, -0.004276389980779660843, 0.008252882783648829434 ) ) ;
#11826 = CARTESIAN_POINT ( 'NONE',  ( -10.86508079875781618, -36.95527278096552237, -35.35100740321762913 ) ) ;
#11827 = CARTESIAN_POINT ( 'NONE',  ( 25.70243777736189728, -65.79472741891204635, -91.80600962488466621 ) ) ;
#11828 = CARTESIAN_POINT ( 'NONE',  ( 109.1778270068192853, 0.004958088776549099581, 0.007885345421917318992 ) ) ;
#11829 = CARTESIAN_POINT ( 'NONE',  ( -55.24198130335446422, -0.009190321388308575826, -0.001391250620105316613 ) ) ;
#11830 = VERTEX_POINT ( 'NONE', #1785 ) ;
#11831 = CARTESIAN_POINT ( 'NONE',  ( 21.16825799904903604, -112.1052598354960281, -75.99073816868427400 ) ) ;
#11832 = ORIENTED_EDGE ( 'NONE', *, *, #27399, .F. ) ;
#11833 = ORIENTED_EDGE ( 'NONE', *, *, #15361, .T. ) ;
#11834 = VERTEX_POINT ( 'NONE', #1649 ) ;
#11835 = EDGE_CURVE ( 'NONE', #27304, #25524, #27329, .T. ) ;
#11836 = CARTESIAN_POINT ( 'NONE',  ( 5.340103579038184556, 32.90561047415598495, 143.7310399932977987 ) ) ;
#11837 = EDGE_CURVE ( 'NONE', #18454, #25074, #10524, .T. ) ;
#11838 = CARTESIAN_POINT ( 'NONE',  ( 1.832998868059858122, -144.3700883710218363, 14.63705790013961305 ) ) ;
#11839 = CARTESIAN_POINT ( 'NONE',  ( 5.340103579038260051, -140.9275371836308750, -43.36842539899515714 ) ) ;
#11840 = ADVANCED_FACE ( 'NONE', ( #15301 ), #3732, .T. ) ;
#11841 = CARTESIAN_POINT ( 'NONE',  ( -8.786685647604890903, 37.00619870957935120, -38.68584556812312059 ) ) ;
#11842 = CARTESIAN_POINT ( 'NONE',  ( 10.93730112726003156, 119.3442956573285443, -92.80059208661575099 ) ) ;
#11843 = CARTESIAN_POINT ( 'NONE',  ( 25.65782528836482257, 112.9169519833626509, 0.5778133093781777641 ) ) ;
#11844 = B_SPLINE_CURVE_WITH_KNOTS ( 'NONE', 3,
 ( #4264, #19383, #6173, #8317, #4126, #13046, #14919, #28292 ),
 .UNSPECIFIED., .F., .F.,
 ( 4, 2, 2, 4 ),
 ( 2.251264292202123005E-16, 0.002761568181852863766, 0.005523136363705502885, 0.01104627272741079413 ),
 .UNSPECIFIED. ) ;
#11845 = CARTESIAN_POINT ( 'NONE',  ( -21.81686047589426636, 27.83628745321488296, 26.62923599424938459 ) ) ;
#11846 = DIRECTION ( 'NONE',  ( -0.5914120900931443270, 0.7398809652418005811, 0.3206367055789464127 ) ) ;
#11847 = CARTESIAN_POINT ( 'NONE',  ( 25.64670758986457955, -56.02376616805354814, -98.03181353150543487 ) ) ;
#11849 = CARTESIAN_POINT ( 'NONE',  ( 13.36082413113061307, 150.7747251079865123, -25.56125765253303328 ) ) ;
#11848 = CARTESIAN_POINT ( 'NONE',  ( -55.24728320129491266, 0.0006547948648751116246, -0.01453410071985669280 ) ) ;
#11850 = CARTESIAN_POINT ( 'NONE',  ( 2.433796855181205476, -144.5536872373190818, -16.65276281464712582 ) ) ;
#11851 = CARTESIAN_POINT ( 'NONE',  ( 25.64681081121879203, 45.54494737132223747, 103.3177883989780952 ) ) ;
#11852 = CARTESIAN_POINT ( 'NONE',  ( -1.056502255334264895, -0.5104472526223093887, -45.80535052436396626 ) ) ;
#11853 = CARTESIAN_POINT ( 'NONE',  ( 26.28373643307407548, -123.8418562193900812, 30.57614217577425464 ) ) ;
#11854 =( BOUNDED_SURFACE ( )  B_SPLINE_SURFACE ( 3, 1, ( 
 ( #21784, #8541 ),
 ( #17305, #23953 ),
 ( #4212, #12994 ),
 ( #2045, #10848 ) ),
 .UNSPECIFIED., .F., .F., .F. ) 
 B_SPLINE_SURFACE_WITH_KNOTS ( ( 4, 4 ),
 ( 2, 2 ),
 ( 0.000000000000000000, 1.000000000000000000 ),
 ( 0.000000000000000000, 1.000000000000000000 ),
 .UNSPECIFIED. ) 
 GEOMETRIC_REPRESENTATION_ITEM ( )  RATIONAL_B_SPLINE_SURFACE ( (
 ( 1.000000000000000000, 1.000000000000000000),
 ( 0.9960225298536222738, 0.9999952330161893110),
 ( 0.9960225298536222738, 0.9999952330161893110),
 ( 1.000000000000000000, 1.000000000000000000) ) ) 
 REPRESENTATION_ITEM ( '' )  SURFACE ( )  );
#11855 = ORIENTED_EDGE ( 'NONE', *, *, #4913, .T. ) ;
#11856 = CARTESIAN_POINT ( 'NONE',  ( 109.1778270068192853, 0.005755170886745426644, -0.007323887274071915615 ) ) ;
#11857 = EDGE_LOOP ( 'NONE', ( #4809, #10329, #14147, #18113 ) ) ;
#11858 = CARTESIAN_POINT ( 'NONE',  ( 109.1586900883932856, -0.002109621908814847055, 0.006819617742893393543 ) ) ;
#11859 = CARTESIAN_POINT ( 'NONE',  ( -1.048172774974298616, 27.73787987941060607, 36.44231470008685392 ) ) ;
#11860 = ORIENTED_EDGE ( 'NONE', *, *, #3506, .F. ) ;
#11861 = VERTEX_POINT ( 'NONE', #12586 ) ;
#11862 = ORIENTED_EDGE ( 'NONE', *, *, #24968, .F. ) ;
#11863 = EDGE_CURVE ( 'NONE', #243, #12327, #23580, .T. ) ;
#11864 = EDGE_CURVE ( 'NONE', #15398, #20457, #18401, .T. ) ;
#11865 = CARTESIAN_POINT ( 'NONE',  ( -20.20700224038492010, 27.82980252387833886, 10.08426345511560207 ) ) ;
#11866 = EDGE_CURVE ( 'NONE', #7658, #21416, #209, .T. ) ;
#11867 = B_SPLINE_CURVE_WITH_KNOTS ( 'NONE', 3,
 ( #1844, #6201, #10649, #8084, #19416, #8487 ),
 .UNSPECIFIED., .F., .F.,
 ( 4, 2, 4 ),
 ( 1.734723475976807094E-18, 0.0004335184443140250579, 0.0008670368886280483810 ),
 .UNSPECIFIED. ) ;
#11868 = DIRECTION ( 'NONE',  ( -1.000000000000000000, 6.938893903907226837E-18, -1.734723475976806709E-18 ) ) ;
#11869 = CARTESIAN_POINT ( 'NONE',  ( 1.833485406944043827, 144.2578170162065021, -15.69895494453236395 ) ) ;
#11870 = DIRECTION ( 'NONE',  ( -0.7071067818211355105, 9.150583771627656306E-17, -0.7071067805519596350 ) ) ;
#11871 = B_SPLINE_CURVE_WITH_KNOTS ( 'NONE', 3,
 ( #11134, #6825, #18023, #13708, #11413, #8838, #2332, #19754, #17742, #192 ),
 .UNSPECIFIED., .F., .F.,
 ( 4, 3, 3, 4 ),
 ( 1.962615573354718958E-17, 0.0002669559177086076006, 0.0005339118354150894060, 0.001067817517169171188 ),
 .UNSPECIFIED. ) ;
#11872 = CARTESIAN_POINT ( 'NONE',  ( 5.340103579038161463, 62.06990748397846858, 133.7487108093465906 ) ) ;
#11873 = CARTESIAN_POINT ( 'NONE',  ( 55.79472521941426777, -35.74479459808802773, -63.36760613016260635 ) ) ;
#11874 = CARTESIAN_POINT ( 'NONE',  ( 109.1592201516379674, -0.001331853079208366458, -0.007748443302128551168 ) ) ;
#11875 = CARTESIAN_POINT ( 'NONE',  ( 109.1592201516379674, -0.002720803050361364321, 0.007376275279030867701 ) ) ;
#11876 = CARTESIAN_POINT ( 'NONE',  ( 26.11404676487259024, -47.08215554553450488, -102.9690087468806325 ) ) ;
#11877 = VERTEX_POINT ( 'NONE', #12726 ) ;
#11878 = ORIENTED_EDGE ( 'NONE', *, *, #8618, .T. ) ;
#11879 = FACE_OUTER_BOUND ( 'NONE', #3642, .T. ) ;
#11881 = CARTESIAN_POINT ( 'NONE',  ( 25.64703792032467078, -91.25955007190263757, 66.48786612795848328 ) ) ;
#11880 = CARTESIAN_POINT ( 'NONE',  ( 1.833485406944043827, 85.72460230293692973, 117.0814567582547596 ) ) ;
#11882 = DIRECTION ( 'NONE',  ( -1.000000000000000000, -0.000000000000000000, -0.000000000000000000 ) ) ;
#11883 = CARTESIAN_POINT ( 'NONE',  ( 32.73300124599736449, -116.5274707358856574, 16.10546300444784507 ) ) ;
#11884 = CARTESIAN_POINT ( 'NONE',  ( -1.259920593601977057, -35.85909937955943860, -28.82601305773640732 ) ) ;
#11885 = VERTEX_POINT ( 'NONE', #4094 ) ;
#11886 = CARTESIAN_POINT ( 'NONE',  ( 25.64670758986457599, 98.03181353150564803, -56.02376616805318577 ) ) ;
#11887 = CARTESIAN_POINT ( 'NONE',  ( -1.463510566862832096, 35.90603835816546763, 29.09194585123793786 ) ) ;
#11888 = CARTESIAN_POINT ( 'NONE',  ( -1.539763995773682614, -38.84665165401045073, 25.17088606276588791 ) ) ;
#11889 = EDGE_LOOP ( 'NONE', ( #15622, #5707, #20653, #22165 ) ) ;
#11890 = CARTESIAN_POINT ( 'NONE',  ( -9.156249394959706578, -48.78605533024757079, -24.29252099376471818 ) ) ;
#11891 = CARTESIAN_POINT ( 'NONE',  ( 10.93730112725932635, 0.000000000000000000, 0.000000000000000000 ) ) ;
#11892 = VECTOR ( 'NONE', #12439, 1000.000000000000000 ) ;
#11893 = VECTOR ( 'NONE', #20814, 1000.000000000000000 ) ;
#11894 = CARTESIAN_POINT ( 'NONE',  ( -1.539760825549686185, 2.469813586483733392, 46.22267384399377477 ) ) ;
#11895 = CARTESIAN_POINT ( 'NONE',  ( -1.045287976400365970, 45.76855895860946077, 1.530335034933974381 ) ) ;
#11896 = EDGE_CURVE ( 'NONE', #22323, #24458, #10866, .T. ) ;
#11897 = B_SPLINE_CURVE_WITH_KNOTS ( 'NONE', 3,
 ( #5441, #3560, #25313, #12341, #21406, #7625, #27594 ),
 .UNSPECIFIED., .F., .F.,
 ( 4, 3, 4 ),
 ( 1.734723475976807094E-18, 0.009512539173626401862, 0.02506242213020843518 ),
 .UNSPECIFIED. ) ;
#11898 = ORIENTED_EDGE ( 'NONE', *, *, #26411, .F. ) ;
#11899 = CARTESIAN_POINT ( 'NONE',  ( 1.834118845439484335, -45.01070051384498072, -137.9527673765110194 ) ) ;
#11900 = EDGE_LOOP ( 'NONE', ( #14219, #3954, #18914, #10841 ) ) ;
#11901 = EDGE_CURVE ( 'NONE', #12482, #24160, #3973, .T. ) ;
#11902 = CARTESIAN_POINT ( 'NONE',  ( 10.93730112725990722, -136.0306644680979389, -65.95960219663263047 ) ) ;
#11903 = ORIENTED_EDGE ( 'NONE', *, *, #4608, .F. ) ;
#11904 = EDGE_CURVE ( 'NONE', #17689, #18738, #17325, .T. ) ;
#11905 = CARTESIAN_POINT ( 'NONE',  ( -1.539760825549686407, -38.84664866728793697, -25.17088484262129455 ) ) ;
#11906 = CARTESIAN_POINT ( 'NONE',  ( 25.64700659047696263, 107.4550658295756023, -34.67498789830337103 ) ) ;
#11907 = CARTESIAN_POINT ( 'NONE',  ( 1.833750490713743853, 0.2669522761665648058, -145.1094586213657180 ) ) ;
#11908 = CARTESIAN_POINT ( 'NONE',  ( 2.263178607246673746, -141.9207363487296618, 31.59906277834177146 ) ) ;
#11909 = ORIENTED_EDGE ( 'NONE', *, *, #3674, .F. ) ;
#11910 = CARTESIAN_POINT ( 'NONE',  ( -1.048171036023512803, -15.11933492062798656, 43.23005599774316465 ) ) ;
#11911 = CARTESIAN_POINT ( 'NONE',  ( -7.078251931573400491, -44.92740138729146082, 26.33626633876272649 ) ) ;
#11912 = DIRECTION ( 'NONE',  ( 0.000000000000000000, 0.000000000000000000, 1.000000000000000000 ) ) ;
#11913 = VERTEX_POINT ( 'NONE', #21512 ) ;
#11914 = EDGE_LOOP ( 'NONE', ( #11717, #28354, #1928, #25551 ) ) ;
#11916 = ORIENTED_EDGE ( 'NONE', *, *, #17768, .T. ) ;
#11915 = B_SPLINE_CURVE_WITH_KNOTS ( 'NONE', 3,
 ( #8524, #6234, #4615, #13383, #17422, #6360, #22182 ),
 .UNSPECIFIED., .F., .F.,
 ( 4, 3, 4 ),
 ( 1.298148181579757605E-17, 0.009512539173626401862, 0.02506242213020844906 ),
 .UNSPECIFIED. ) ;
#11917 = CARTESIAN_POINT ( 'NONE',  ( -1.046936909428679785, 37.78538189376546086, 25.87632113675119427 ) ) ;
#11918 = CARTESIAN_POINT ( 'NONE',  ( -20.20700224038492010, -0.9908225410480588913, -29.58392382092672435 ) ) ;
#11920 = CARTESIAN_POINT ( 'NONE',  ( -1.056502255334264895, 37.35734037467673119, 26.51074901220462721 ) ) ;
#11919 = CARTESIAN_POINT ( 'NONE',  ( 1.833721034905660074, 107.5990973104336064, -97.36162733017604864 ) ) ;
#11921 = B_SPLINE_CURVE_WITH_KNOTS ( 'NONE', 3,
 ( #22515, #24963, #11281, #18170, #630, #20049, #20338 ),
 .UNSPECIFIED., .F., .F.,
 ( 4, 3, 4 ),
 ( 0.000000000000000000, 0.02398743853561332434, 0.04000277880656220170 ),
 .UNSPECIFIED. ) ;
#11922 = CARTESIAN_POINT ( 'NONE',  ( 14.74894986621300319, -5.136656239696338858E-17, 37.50000000000001421 ) ) ;
#11923 = CARTESIAN_POINT ( 'NONE',  ( -1.239374126674604337, -11.92219841463799135, 44.48112152129359487 ) ) ;
#11924 = CARTESIAN_POINT ( 'NONE',  ( -12.82751273423882843, 44.03362901247002981, -21.21958768041810117 ) ) ;
#11925 = CARTESIAN_POINT ( 'NONE',  ( -1.031422197589711987, -36.13727897780105991, 28.14735071801782595 ) ) ;
#11926 = ORIENTED_EDGE ( 'NONE', *, *, #676, .T. ) ;
#11927 = CARTESIAN_POINT ( 'NONE',  ( -23.79248802219729697, -24.83956736572394064, 22.01156985585195258 ) ) ;
#11928 = LINE ( 'NONE', #20416, #11114 ) ;
#11929 = CARTESIAN_POINT ( 'NONE',  ( 25.98107933586698692, -67.37827847766595823, 90.88151529733785594 ) ) ;
#11930 = CARTESIAN_POINT ( 'NONE',  ( 26.04756280548354752, -67.42001818240403566, -90.90573670389308347 ) ) ;
#11931 = LINE ( 'NONE', #9784, #975 ) ;
#11932 = CARTESIAN_POINT ( 'NONE',  ( 5.340103556456475609, -120.6284720803331680, 84.79482753886512114 ) ) ;
#11933 = ORIENTED_EDGE ( 'NONE', *, *, #26093, .F. ) ;
#11934 = CARTESIAN_POINT ( 'NONE',  ( 55.79472521941428198, -71.00924468211167095, 15.83764557006246676 ) ) ;
#11935 = CARTESIAN_POINT ( 'NONE',  ( 16.75465622695653067, -108.7410129416641098, 91.67104679059862349 ) ) ;
#11936 = B_SPLINE_CURVE_WITH_KNOTS ( 'NONE', 3,
 ( #18872, #5929, #9968, #27645, #1451, #10257, #25212, #14245 ),
 .UNSPECIFIED., .F., .F.,
 ( 4, 2, 2, 4 ),
 ( 1.734723475976807094E-18, 0.0002429588503611233819, 0.0004859177007222450291, 0.0009718354014444937445 ),
 .UNSPECIFIED. ) ;
#11937 = CARTESIAN_POINT ( 'NONE',  ( 55.79472521941428198, -72.27573336313959373, 8.328398066091525109 ) ) ;
#11938 = EDGE_CURVE ( 'NONE', #4019, #20744, #21321, .T. ) ;
#11939 = ORIENTED_EDGE ( 'NONE', *, *, #10371, .T. ) ;
#11940 = EDGE_LOOP ( 'NONE', ( #3475, #12497, #18478, #14533 ) ) ;
#11941 = EDGE_CURVE ( 'NONE', #13547, #14894, #7887, .T. ) ;
#11942 = CARTESIAN_POINT ( 'NONE',  ( -1.048171036023517466, -45.78635789057865679, -1.020520027228972504 ) ) ;
#11943 = CARTESIAN_POINT ( 'NONE',  ( -1.048996300304493978, -43.78665266739846373, -13.42280206896960060 ) ) ;
#11944 = CARTESIAN_POINT ( 'NONE',  ( -20.20700224038492010, 16.58740185276710832, -24.51628800869052682 ) ) ;
#11945 = CARTESIAN_POINT ( 'NONE',  ( 19.66333377628712853, -77.29039328249547225, -114.0223162644910673 ) ) ;
#11946 = CARTESIAN_POINT ( 'NONE',  ( 1.833750490713699666, 125.8019536335930297, -72.32354185792426904 ) ) ;
#11947 = ORIENTED_EDGE ( 'NONE', *, *, #16551, .F. ) ;
#11948 = CARTESIAN_POINT ( 'NONE',  ( 5.340103579038300907, 84.79482754232432740, -120.6284720963478065 ) ) ;
#11949 = CARTESIAN_POINT ( 'NONE',  ( 25.64708228042118776, 34.85404436489494628, 107.3971738194632906 ) ) ;
#11950 = CARTESIAN_POINT ( 'NONE',  ( 109.1586900883932856, -0.004701023939945749193, 0.005371970278528625728 ) ) ;
#11951 = VERTEX_POINT ( 'NONE', #24550 ) ;
#11952 = ORIENTED_EDGE ( 'NONE', *, *, #886, .T. ) ;
#11953 = CARTESIAN_POINT ( 'NONE',  ( -1.048171036023512803, -43.23005599774311492, -15.11933492062811801 ) ) ;
#11954 = CARTESIAN_POINT ( 'NONE',  ( 109.1586059443104944, -0.006637156007970172224, 0.002447596125914148699 ) ) ;
#11955 = CARTESIAN_POINT ( 'NONE',  ( -20.24399999263415140, 27.76448601145554562, 10.36954246768216059 ) ) ;
#11956 = B_SPLINE_CURVE_WITH_KNOTS ( 'NONE', 3,
 ( #24667, #17722, #2465, #308, #2309, #24511, #9096, #26641 ),
 .UNSPECIFIED., .F., .F.,
 ( 4, 2, 2, 4 ),
 ( 9.813077866773594792E-18, 0.0002429592666046763807, 0.0004859185332093429494, 0.0009718370664186761409 ),
 .UNSPECIFIED. ) ;
#11957 = CARTESIAN_POINT ( 'NONE',  ( 2.433796855181205476, -84.34988187690851191, -118.5671979538065273 ) ) ;
#11958 = CARTESIAN_POINT ( 'NONE',  ( 1.833838850093453043, -138.0075846865483982, 44.84138612521046241 ) ) ;
#11959 = ORIENTED_EDGE ( 'NONE', *, *, #25943, .F. ) ;
#11960 = CARTESIAN_POINT ( 'NONE',  ( 25.70243777736187951, 84.42566495012547989, -75.03063812271970789 ) ) ;
#11961 = CARTESIAN_POINT ( 'NONE',  ( 1.832998868059858122, -137.8420662456167065, -45.34898734666188602 ) ) ;
#11962 = CARTESIAN_POINT ( 'NONE',  ( 55.79472521941426777, -72.75035398477136539, -0.7279028900801322033 ) ) ;
#11963 = CARTESIAN_POINT ( 'NONE',  ( 109.1592201516379674, -0.001127733110579631293, 0.007780772729118876421 ) ) ;
#11964 = FACE_OUTER_BOUND ( 'NONE', #6274, .T. ) ;
#11965 = CARTESIAN_POINT ( 'NONE',  ( -1.539760825549679080, 38.84664866728813593, 25.17088484262099612 ) ) ;
#11966 = EDGE_CURVE ( 'NONE', #13932, #21238, #17178, .T. ) ;
#11967 = EDGE_CURVE ( 'NONE', #5205, #25606, #6053, .T. ) ;
#11968 = ORIENTED_EDGE ( 'NONE', *, *, #11671, .T. ) ;
#11969 = CARTESIAN_POINT ( 'NONE',  ( 25.73574536432415627, 22.69874377039439395, 110.6664861019684878 ) ) ;
#11970 = ORIENTED_EDGE ( 'NONE', *, *, #22999, .T. ) ;
#11971 = EDGE_CURVE ( 'NONE', #5935, #2087, #10181, .T. ) ;
#11972 = EDGE_CURVE ( 'NONE', #20933, #19163, #22114, .T. ) ;
#11973 = ORIENTED_EDGE ( 'NONE', *, *, #19307, .T. ) ;
#11974 = EDGE_LOOP ( 'NONE', ( #10113, #8639, #5749, #11781 ) ) ;
#11975 = CONICAL_SURFACE ( 'NONE', #11508, 34.60786435723138510, 0.8559913436420825139 ) ;
#11976 = VECTOR ( 'NONE', #13908, 1000.000000000000114 ) ;
#11977 = CARTESIAN_POINT ( 'NONE',  ( -1.048994561756796839, 43.31369460697995777, 14.87838255483211469 ) ) ;
#11978 = DIRECTION ( 'NONE',  ( -1.000000000000000000, -0.000000000000000000, -0.000000000000000000 ) ) ;
#11980 = VECTOR ( 'NONE', #3910, 1000.000000000000114 ) ;
#11979 =( BOUNDED_SURFACE ( )  B_SPLINE_SURFACE ( 3, 1, ( 
 ( #11256, #6806 ),
 ( #9243, #24366 ),
 ( #6953, #20026 ),
 ( #4629, #13549 ) ),
 .UNSPECIFIED., .F., .F., .F. ) 
 B_SPLINE_SURFACE_WITH_KNOTS ( ( 4, 4 ),
 ( 2, 2 ),
 ( 0.000000000000000000, 1.000000000000000000 ),
 ( 0.000000000000000000, 1.000000000000000000 ),
 .UNSPECIFIED. ) 
 GEOMETRIC_REPRESENTATION_ITEM ( )  RATIONAL_B_SPLINE_SURFACE ( (
 ( 1.000000000000000000, 1.000000000000000000),
 ( 0.7789835883360576307, 0.9689951854195403280),
 ( 0.7789835883360576307, 0.9689951854195403280),
 ( 1.000000000000000000, 1.000000000000000000) ) ) 
 REPRESENTATION_ITEM ( '' )  SURFACE ( )  );
#11981 = CARTESIAN_POINT ( 'NONE',  ( 109.1592201516379674, -0.003661068210037343815, -0.006957642258146904887 ) ) ;
#11982 = CARTESIAN_POINT ( 'NONE',  ( 1.893872463202051604, -97.83022426232032842, 107.2274879309823632 ) ) ;
#11983 = CARTESIAN_POINT ( 'NONE',  ( 109.1592201516379674, -0.005631912476303850730, 0.005485778713202916178 ) ) ;
#11984 = CARTESIAN_POINT ( 'NONE',  ( 1.833750490713671244, 132.4555075118568368, 59.26520711749913772 ) ) ;
#11985 = CARTESIAN_POINT ( 'NONE',  ( 2.108985857320898827, -133.2480631238189517, -57.92316197981790538 ) ) ;
#11986 = CARTESIAN_POINT ( 'NONE',  ( -15.02187109954780553, 33.49412687891621232, 32.04062513125082035 ) ) ;
#11987 = CARTESIAN_POINT ( 'NONE',  ( 30.58324630866343696, 41.10517620771203440, 113.7441547345748489 ) ) ;
#11988 = CARTESIAN_POINT ( 'NONE',  ( -25.21435515916043713, -4.655591116594118617, 34.29329011225960500 ) ) ;
#11989 = EDGE_CURVE ( 'NONE', #23103, #9163, #20950, .T. ) ;
#11990 = AXIS2_PLACEMENT_3D ( 'NONE', #26822, #20344, #11718 ) ;
#11991 = CIRCLE ( 'NONE', #17919, 34.60786435723138510 ) ;
#11992 = VECTOR ( 'NONE', #15357, 1000.000000000000000 ) ;
#11993 = CARTESIAN_POINT ( 'NONE',  ( -4.473127245936434626, -26.34600523034507802, 41.70021447285083127 ) ) ;
#11994 = B_SPLINE_CURVE_WITH_KNOTS ( 'NONE', 3,
 ( #12343, #10215, #18976, #8056, #23444, #3706, #19797, #2524, #11035, #4544 ),
 .UNSPECIFIED., .F., .F.,
 ( 4, 2, 2, 2, 4 ),
 ( 2.847672227753435151E-16, 0.0003346187017559034554, 0.0006692374035115221994, 0.001003856105267140727, 0.001338474807022759470 ),
 .UNSPECIFIED. ) ;
#11995 = B_SPLINE_CURVE_WITH_KNOTS ( 'NONE', 3,
 ( #26315, #17391, #4576, #4156, #2408, #26044, #23903, #19690, #6470, #21865 ),
 .UNSPECIFIED., .F., .F.,
 ( 4, 3, 3, 4 ),
 ( 1.387778780781445676E-17, 0.0002669560319015654788, 0.0005492286108966274675, 0.0008315040496093373083 ),
 .UNSPECIFIED. ) ;
#11996 = LINE ( 'NONE', #9846, #714 ) ;
#11997 = CARTESIAN_POINT ( 'NONE',  ( 10.93730112725997294, 26.59437931460951177, -148.8212007290660210 ) ) ;
#11998 = EDGE_CURVE ( 'NONE', #3886, #25165, #2378, .T. ) ;
#11999 = ORIENTED_EDGE ( 'NONE', *, *, #13183, .T. ) ;
#12000 = CARTESIAN_POINT ( 'NONE',  ( 32.73300124599732186, 0.000000000000000000, 0.000000000000000000 ) ) ;
#12001 = AXIS2_PLACEMENT_3D ( 'NONE', #23590, #27881, #9914 ) ;
#12002 = EDGE_CURVE ( 'NONE', #25271, #2611, #5510, .T. ) ;
#12003 = VERTEX_POINT ( 'NONE', #9275 ) ;
#12004 = CARTESIAN_POINT ( 'NONE',  ( -1.050229599974473516, 43.63650726458064355, -13.90955673306141627 ) ) ;
#12005 = DIRECTION ( 'NONE',  ( 0.000000000000000000, 1.000000000000000000, 3.469446951953603342E-16 ) ) ;
#12006 = ORIENTED_EDGE ( 'NONE', *, *, #21785, .T. ) ;
#12007 = ORIENTED_EDGE ( 'NONE', *, *, #17438, .T. ) ;
#12008 = VERTEX_POINT ( 'NONE', #13868 ) ;
#12009 = ORIENTED_EDGE ( 'NONE', *, *, #11313, .F. ) ;
#12010 = CARTESIAN_POINT ( 'NONE',  ( 109.1624594426973260, 0.01476644236456051487, -0.006066618937909722294 ) ) ;
#12011 = AXIS2_PLACEMENT_3D ( 'NONE', #21259, #17075, #25866 ) ;
#12012 = DIRECTION ( 'NONE',  ( 0.000000000000000000, 0.000000000000000000, 1.000000000000000000 ) ) ;
#12013 = AXIS2_PLACEMENT_3D ( 'NONE', #17814, #15652, #9059 ) ;
#12014 = CARTESIAN_POINT ( 'NONE',  ( 25.69398547355839568, 107.6418378907644353, 34.19446713634620494 ) ) ;
#12015 = CARTESIAN_POINT ( 'NONE',  ( -1.031422197589716205, 25.67058493451498080, 37.93675465142445091 ) ) ;
#12016 = CARTESIAN_POINT ( 'NONE',  ( 26.11404676487257603, 36.06104232266594067, -107.3263591096426666 ) ) ;
#12017 = CARTESIAN_POINT ( 'NONE',  ( 109.1587776205901861, -0.003057017121600591122, -0.006661366261223543826 ) ) ;
#12018 = CARTESIAN_POINT ( 'NONE',  ( -1.539760825549678636, 25.17088484262142956, -38.84664866728784460 ) ) ;
#12019 =( BOUNDED_SURFACE ( )  B_SPLINE_SURFACE ( 3, 1, ( 
 ( #20065, #28271 ),
 ( #10876, #13160 ),
 ( #15164, #23988 ),
 ( #19933, #6995 ) ),
 .UNSPECIFIED., .F., .F., .F. ) 
 B_SPLINE_SURFACE_WITH_KNOTS ( ( 4, 4 ),
 ( 2, 2 ),
 ( 0.000000000000000000, 1.000000000000000000 ),
 ( 0.000000000000000000, 1.000000000000000000 ),
 .UNSPECIFIED. ) 
 GEOMETRIC_REPRESENTATION_ITEM ( )  RATIONAL_B_SPLINE_SURFACE ( (
 ( 1.000000000000000000, 1.000000000000000000),
 ( 0.9956975270656955868, 0.8568959468854907557),
 ( 0.9956975270656955868, 0.8568959468854907557),
 ( 1.000000000000000000, 1.000000000000000000) ) ) 
 REPRESENTATION_ITEM ( '' )  SURFACE ( )  );
#12020 = FACE_OUTER_BOUND ( 'NONE', #22409, .T. ) ;
#12022 = CARTESIAN_POINT ( 'NONE',  ( 109.1592201516379674, 0.007780772729122757865, -0.001127733110588145750 ) ) ;
#12021 = CARTESIAN_POINT ( 'NONE',  ( 1.833206308920112049, 59.70089323729912678, -132.2594750499820009 ) ) ;
#12023 = CARTESIAN_POINT ( 'NONE',  ( 30.59138290137885008, -49.72302320601725967, -105.0379801549013337 ) ) ;
#12024 = EDGE_CURVE ( 'NONE', #14776, #17694, #26232, .T. ) ;
#12025 = ORIENTED_EDGE ( 'NONE', *, *, #18654, .T. ) ;
#12026 = CARTESIAN_POINT ( 'NONE',  ( 32.73300124599732186, 0.000000000000000000, 0.000000000000000000 ) ) ;
#12027 = ADVANCED_FACE ( 'NONE', ( #24396 ), #24565, .F. ) ;
#12029 = CARTESIAN_POINT ( 'NONE',  ( -1.044557008772710294, 25.56990300677035677, 37.98985164565299755 ) ) ;
#12028 = CARTESIAN_POINT ( 'NONE',  ( 1.833485406944043827, 84.86072343962567288, 117.7091014914953320 ) ) ;
#12030 = CARTESIAN_POINT ( 'NONE',  ( 1.833485406944057594, -84.86072343962649711, 117.7091014914947209 ) ) ;
#12031 = DIRECTION ( 'NONE',  ( -1.000000000000000000, -0.000000000000000000, -0.000000000000000000 ) ) ;
#12032 = CARTESIAN_POINT ( 'NONE',  ( 2.108985857320881063, 144.6256801373127701, 13.91228467251867507 ) ) ;
#12033 = B_SPLINE_CURVE_WITH_KNOTS ( 'NONE', 3,
 ( #28123, #4230, #10579, #17752 ),
 .UNSPECIFIED., .F., .F.,
 ( 4, 4 ),
 ( 3.385911829997767421E-16, 0.01077107486149848914 ),
 .UNSPECIFIED. ) ;
#12034 = ORIENTED_EDGE ( 'NONE', *, *, #8172, .T. ) ;
#12035 = CARTESIAN_POINT ( 'NONE',  ( 1.833750490713730974, 44.58740205676330248, 138.0897889879340710 ) ) ;
#12036 = EDGE_CURVE ( 'NONE', #12242, #17470, #13053, .T. ) ;
#12037 = CARTESIAN_POINT ( 'NONE',  ( 1.833485406944085350, 132.3460930279899515, -59.50871042846091541 ) ) ;
#12038 = CARTESIAN_POINT ( 'NONE',  ( 10.93730112725936188, 148.8212007290658505, 26.59437931460817595 ) ) ;
#12039 = ORIENTED_EDGE ( 'NONE', *, *, #22610, .T. ) ;
#12040 = DIRECTION ( 'NONE',  ( -0.5946245182733607137, -0.3994439555666277619, 0.6977579871484522744 ) ) ;
#12041 = AXIS2_PLACEMENT_3D ( 'NONE', #20976, #16090, #24894 ) ;
#12042 = CARTESIAN_POINT ( 'NONE',  ( 109.1586900883932856, 0.006757191295060844746, 0.002301750759599800571 ) ) ;
#12043 = ADVANCED_FACE ( 'NONE', ( #5825 ), #10014, .F. ) ;
#12044 = CIRCLE ( 'NONE', #28106, 34.60786435723138510 ) ;
#12045 = CARTESIAN_POINT ( 'NONE',  ( 28.37599760073042177, -65.97809271467072278, -93.86375353586234382 ) ) ;
#12046 = EDGE_LOOP ( 'NONE', ( #25690, #4880, #21700, #12204 ) ) ;
#12047 = CARTESIAN_POINT ( 'NONE',  ( 1.833485406944043827, -96.69979900902094982, -108.1939177044935860 ) ) ;
#12048 = ORIENTED_EDGE ( 'NONE', *, *, #681, .F. ) ;
#12049 = LINE ( 'NONE', #20820, #15209 ) ;
#12050 = LINE ( 'NONE', #8164, #954 ) ;
#12051 = ORIENTED_EDGE ( 'NONE', *, *, #2431, .T. ) ;
#12052 = CARTESIAN_POINT ( 'NONE',  ( 2.108393763691212452, -60.26375949664278409, 132.2055356348359112 ) ) ;
#12053 = CARTESIAN_POINT ( 'NONE',  ( 2.433796855181233454, -118.5671979538051062, -84.34988187691051564 ) ) ;
#12054 = CARTESIAN_POINT ( 'NONE',  ( 1.832998868059890096, -59.50898020732598326, 132.3466930259791923 ) ) ;
#12055 = ORIENTED_EDGE ( 'NONE', *, *, #14405, .T. ) ;
#12056 = VECTOR ( 'NONE', #10317, 1000.000000000000000 ) ;
#12057 = CARTESIAN_POINT ( 'NONE',  ( -7.078251931573400491, 50.86685171665412497, -11.16394717458693897 ) ) ;
#12059 = CARTESIAN_POINT ( 'NONE',  ( -1.583189561560252701, -38.94740041318275559, 25.21827308671274182 ) ) ;
#12058 = CARTESIAN_POINT ( 'NONE',  ( 1.833838848569414148, 85.14939661881724930, -117.5008734796303429 ) ) ;
#12060 = CARTESIAN_POINT ( 'NONE',  ( 16.75465622695626422, -120.7871673903172223, -75.09093759626998121 ) ) ;
#12061 = ORIENTED_EDGE ( 'NONE', *, *, #6087, .T. ) ;
#12062 = CIRCLE ( 'NONE', #22656, 53.53553390275978785 ) ;
#12063 = EDGE_LOOP ( 'NONE', ( #15500, #25036, #13353, #21827 ) ) ;
#12064 = ORIENTED_EDGE ( 'NONE', *, *, #11901, .F. ) ;
#12065 = CARTESIAN_POINT ( 'NONE',  ( -1.045287976400383290, -44.00138577190632816, 12.68782741917368106 ) ) ;
#12066 = CARTESIAN_POINT ( 'NONE',  ( -1.031422197589711987, -12.69107518035471394, 44.01264471863858319 ) ) ;
#12067 = ADVANCED_FACE ( 'NONE', ( #27391 ), #11531, .T. ) ;
#12069 = CARTESIAN_POINT ( 'NONE',  ( -20.57838717382308147, -7.715628353033886278, -28.96176188950215646 ) ) ;
#12068 = CARTESIAN_POINT ( 'NONE',  ( 10.93730112725943471, 119.3442956573271516, 92.80059208661684522 ) ) ;
#12070 = CARTESIAN_POINT ( 'NONE',  ( -20.20612092514785019, 27.77903665678167400, -10.22177639105870384 ) ) ;
#12071 = CARTESIAN_POINT ( 'NONE',  ( 1.833750490713671244, -132.4555075118564389, -59.26520711749999748 ) ) ;
#12072 = ORIENTED_EDGE ( 'NONE', *, *, #10168, .F. ) ;
#12073 = CARTESIAN_POINT ( 'NONE',  ( 1.833838850093465700, 107.8375718686139351, 97.09738119087744224 ) ) ;
#12074 = CARTESIAN_POINT ( 'NONE',  ( 25.64681081121879203, 45.54494737132363724, -103.3177883989774841 ) ) ;
#12075 = ORIENTED_EDGE ( 'NONE', *, *, #10774, .T. ) ;
#12076 = CARTESIAN_POINT ( 'NONE',  ( 109.1778270068192853, 0.008236503545668636198, 0.004349865064721274849 ) ) ;
#12077 = CARTESIAN_POINT ( 'NONE',  ( -1.019300379054419725, -38.21680004809182662, -25.26451264419630860 ) ) ;
#12078 = CARTESIAN_POINT ( 'NONE',  ( 25.70243777736190793, 110.3252221127465447, 24.19989514742760051 ) ) ;
#12079 = CARTESIAN_POINT ( 'NONE',  ( 2.433796855181205476, -133.5135467655521779, 57.85512797797844087 ) ) ;
#12080 = EDGE_CURVE ( 'NONE', #17967, #24477, #21974, .T. ) ;
#12081 = CARTESIAN_POINT ( 'NONE',  ( 10.93730112726003156, 71.28103789255123957, -133.3192575531793693 ) ) ;
#12082 = CARTESIAN_POINT ( 'NONE',  ( 2.433796855181205476, -109.1007109081232471, 96.28145139437646094 ) ) ;
#12083 = CARTESIAN_POINT ( 'NONE',  ( -21.41427618760447871, 29.81030852927067443, -7.777551129310157130 ) ) ;
#12084 = ORIENTED_EDGE ( 'NONE', *, *, #23574, .F. ) ;
#12085 = CARTESIAN_POINT ( 'NONE',  ( 109.1589550718174877, 0.007507020724817403678, 0.001014448720240663810 ) ) ;
#12086 = CARTESIAN_POINT ( 'NONE',  ( -90.83090735639699176, 0.000000000000000000, 0.000000000000000000 ) ) ;
#12087 = VECTOR ( 'NONE', #8510, 1000.000000000000341 ) ;
#12088 = CARTESIAN_POINT ( 'NONE',  ( 30.58324630866349381, 52.76949945162388644, 108.8243914523531686 ) ) ;
#12089 = AXIS2_PLACEMENT_3D ( 'NONE', #8351, #15362, #24036 ) ;
#12090 = VERTEX_POINT ( 'NONE', #25108 ) ;
#12091 = VERTEX_POINT ( 'NONE', #12151 ) ;
#12092 = CIRCLE ( 'NONE', #23114, 117.6351876552689504 ) ;
#12093 = CARTESIAN_POINT ( 'NONE',  ( -55.24198130335446422, -0.004163123460805480056, 0.008310594958150618883 ) ) ;
#12094 = CARTESIAN_POINT ( 'NONE',  ( -25.21435515916043713, -30.48034229288627017, 16.39063784838775462 ) ) ;
#12095 = B_SPLINE_CURVE_WITH_KNOTS ( 'NONE', 3,
 ( #1683, #3437, #8060, #21122, #11178, #22113, #26560 ),
 .UNSPECIFIED., .F., .F.,
 ( 4, 3, 4 ),
 ( 0.000000000000000000, 0.006568092053401763247, 0.02506242213020846987 ),
 .UNSPECIFIED. ) ;
#12096 = CARTESIAN_POINT ( 'NONE',  ( 25.64704443564077607, -23.60610532597032218, 110.4160069635933326 ) ) ;
#12097 = CARTESIAN_POINT ( 'NONE',  ( -28.41354790283022069, -14.62505768302813713, -18.00456980371894744 ) ) ;
#12098 = CARTESIAN_POINT ( 'NONE',  ( 2.108393763691201350, -144.6252321290182579, 13.91282116576931394 ) ) ;
#12099 = CARTESIAN_POINT ( 'NONE',  ( -4.178947244162634966, 37.51424432987651159, -31.41809272265936315 ) ) ;
#12100 = CARTESIAN_POINT ( 'NONE',  ( 109.1587776205901577, -0.005502145856754194451, 0.004842060007774028410 ) ) ;
#12101 = EDGE_LOOP ( 'NONE', ( #11414, #8992, #24773, #6404 ) ) ;
#12102 = ORIENTED_EDGE ( 'NONE', *, *, #14718, .F. ) ;
#12103 = CARTESIAN_POINT ( 'NONE',  ( -15.02187109954782862, -41.75590530176324222, -20.12219089991075904 ) ) ;
#12104 = CARTESIAN_POINT ( 'NONE',  ( -8.786685647604885574, 6.096987947571466530E-17, -1.524246986892866633E-17 ) ) ;
#12105 = EDGE_CURVE ( 'NONE', #21619, #20671, #13833, .T. ) ;
#12106 = CARTESIAN_POINT ( 'NONE',  ( 55.49584447822657296, 48.74506217377955863, -53.73688382046214684 ) ) ;
#12107 = CARTESIAN_POINT ( 'NONE',  ( -1.045287976400383290, 12.68782741917383738, 44.00138577190627842 ) ) ;
#12108 = CARTESIAN_POINT ( 'NONE',  ( -6.574463467970654840, 5.014313797967739461, 51.07975593197901532 ) ) ;
#12109 = CIRCLE ( 'NONE', #1067, 151.1787379149930359 ) ;
#12110 = DIRECTION ( 'NONE',  ( 0.000000000000000000, 0.000000000000000000, 1.000000000000000000 ) ) ;
#12111 = ORIENTED_EDGE ( 'NONE', *, *, #6974, .T. ) ;
#12112 = CARTESIAN_POINT ( 'NONE',  ( -28.41354790283022069, 8.345538364877384652, 21.64275480268738860 ) ) ;
#12113 = CARTESIAN_POINT ( 'NONE',  ( -8.786685647604885574, 6.096987947571466530E-17, -1.524246986892866633E-17 ) ) ;
#12114 = VECTOR ( 'NONE', #27762, 999.9999999999998863 ) ;
#12115 = CARTESIAN_POINT ( 'NONE',  ( 10.93730112725953596, 92.80059208661681680, 119.3442956573276206 ) ) ;
#12116 = ADVANCED_FACE ( 'NONE', ( #7998 ), #18660, .F. ) ;
#12117 = EDGE_CURVE ( 'NONE', #20493, #5939, #28133, .T. ) ;
#12118 = CARTESIAN_POINT ( 'NONE',  ( -2.904412668506658246, -40.16685646686189415, 25.64203923793618145 ) ) ;
#12119 = DIRECTION ( 'NONE',  ( -0.5914120900931443270, -0.7643865440136122791, 0.2567974902965066142 ) ) ;
#12120 = VERTEX_POINT ( 'NONE', #7847 ) ;
#12121 = CARTESIAN_POINT ( 'NONE',  ( -7.078251931573406708, -11.16394717458641850, 50.86685171665422445 ) ) ;
#12122 = CARTESIAN_POINT ( 'NONE',  ( -21.41427618760458884, -28.68857606049974862, -11.22988868156173581 ) ) ;
#12123 = ORIENTED_EDGE ( 'NONE', *, *, #10563, .T. ) ;
#12124 = EDGE_LOOP ( 'NONE', ( #17726, #21563, #1630, #25058 ) ) ;
#12125 = VECTOR ( 'NONE', #6769, 1000.000000000000000 ) ;
#12126 = VERTEX_POINT ( 'NONE', #20772 ) ;
#12127 = CARTESIAN_POINT ( 'NONE',  ( -25.21435515916025594, 1.749597353048488237E-16, -4.373993382621220594E-17 ) ) ;
#12128 = EDGE_CURVE ( 'NONE', #12494, #27772, #4797, .T. ) ;
#12129 = DIRECTION ( 'NONE',  ( 0.000000000000000000, 5.223019709708233256E-21, -1.000000000000000000 ) ) ;
#12130 = VECTOR ( 'NONE', #13808, 1000.000000000000114 ) ;
#12131 = FACE_OUTER_BOUND ( 'NONE', #24287, .T. ) ;
#12132 = CARTESIAN_POINT ( 'NONE',  ( 2.108985857320926360, -126.4634971826979211, -71.53406810961618589 ) ) ;
#12133 = EDGE_CURVE ( 'NONE', #5543, #5967, #13399, .T. ) ;
#12134 = CARTESIAN_POINT ( 'NONE',  ( 21.16825799904930605, 135.0813719997364899, 9.757279788663185016 ) ) ;
#12135 = B_SPLINE_CURVE_WITH_KNOTS ( 'NONE', 3,
 ( #14861, #12830, #10836, #3633, #16891, #25542 ),
 .UNSPECIFIED., .F., .F.,
 ( 4, 2, 4 ),
 ( 3.709064347514218400E-16, 0.003576372551511170905, 0.007152745103021971446 ),
 .UNSPECIFIED. ) ;
#12136 = CARTESIAN_POINT ( 'NONE',  ( -20.57838717382308147, 18.89542499756533545, 23.26537097894084383 ) ) ;
#12137 = CARTESIAN_POINT ( 'NONE',  ( 25.64681081121879203, 84.18689316040048709, 75.24277141833519522 ) ) ;
#12138 = ADVANCED_FACE ( 'NONE', ( #20629 ), #1012, .F. ) ;
#12139 = CARTESIAN_POINT ( 'NONE',  ( -23.79248802219730052, 24.83956736572410051, -22.01156985585177495 ) ) ;
#12140 = DIRECTION ( 'NONE',  ( 0.7637818620346801257, 0.02150485345384395286, -0.6451161201712182214 ) ) ;
#12141 = CARTESIAN_POINT ( 'NONE',  ( -8.786685647604896232, 23.24040270374459993, 48.22796981442743913 ) ) ;
#12142 = CARTESIAN_POINT ( 'NONE',  ( 55.49584447822657296, 22.16497542184496794, -69.08290406177557941 ) ) ;
#12143 = CARTESIAN_POINT ( 'NONE',  ( 25.64660436782553887, -83.52001792470935015, 75.98230157781821958 ) ) ;
#12144 = CARTESIAN_POINT ( 'NONE',  ( 25.87036335909428075, -22.53739730344121384, 110.7910326764401390 ) ) ;
#12145 = DIRECTION ( 'NONE',  ( 1.000000000000000000, -6.938893903907226837E-18, 1.734723475976806709E-18 ) ) ;
#12146 = FACE_OUTER_BOUND ( 'NONE', #20390, .T. ) ;
#12147 = CARTESIAN_POINT ( 'NONE',  ( -1.619063947482197729, 16.67502769180622835, 43.26576862488415287 ) ) ;
#12148 = ORIENTED_EDGE ( 'NONE', *, *, #26257, .T. ) ;
#12149 = CARTESIAN_POINT ( 'NONE',  ( -1.045287976400362417, 25.66401692419989899, -37.92705037016767733 ) ) ;
#12150 = ORIENTED_EDGE ( 'NONE', *, *, #19929, .T. ) ;
#12151 = CARTESIAN_POINT ( 'NONE',  ( 10.93730112725990011, -151.0983828010091656, -4.928439153521871674 ) ) ;
#12152 = CARTESIAN_POINT ( 'NONE',  ( 2.430230287190581429, 138.8342928068226172, -43.58368230469247351 ) ) ;
#12153 = ORIENTED_EDGE ( 'NONE', *, *, #27850, .F. ) ;
#12154 = VERTEX_POINT ( 'NONE', #12698 ) ;
#12155 = ORIENTED_EDGE ( 'NONE', *, *, #22267, .T. ) ;
#12156 = B_SPLINE_CURVE_WITH_KNOTS ( 'NONE', 3,
 ( #7737, #16491, #4232, #23840 ),
 .UNSPECIFIED., .F., .F.,
 ( 4, 4 ),
 ( 6.662151249755524083E-16, 0.008383748772660135420 ),
 .UNSPECIFIED. ) ;
#12157 = CARTESIAN_POINT ( 'NONE',  ( 1.832998868059858122, -15.69902610990472880, 144.2584710144579958 ) ) ;
#12158 = EDGE_CURVE ( 'NONE', #18255, #711, #24377, .T. ) ;
#12159 = CARTESIAN_POINT ( 'NONE',  ( 55.79472521941428198, 68.96476385670696629, -23.17337251492691763 ) ) ;
#12160 = EDGE_CURVE ( 'NONE', #10148, #12210, #11689, .T. ) ;
#12161 = CARTESIAN_POINT ( 'NONE',  ( 109.1592201516379674, 0.001127733110579580769, -0.007780772729118883360 ) ) ;
#12162 = CARTESIAN_POINT ( 'NONE',  ( 25.73574536432415627, 35.67555431182972825, -107.1893601970590879 ) ) ;
#12163 = DIRECTION ( 'NONE',  ( 0.5914120900931444380, 0.3962188444547191657, 0.7023121577978167496 ) ) ;
#12164 = CARTESIAN_POINT ( 'NONE',  ( 2.063896406836609909, -31.51663808384454768, -141.8093313989364219 ) ) ;
#12165 = FACE_OUTER_BOUND ( 'NONE', #6183, .T. ) ;
#12166 = CARTESIAN_POINT ( 'NONE',  ( -2.265401668238147259, -43.82493763960398070, -17.02144111536863136 ) ) ;
#12167 = EDGE_LOOP ( 'NONE', ( #21896, #28401, #1659, #10357 ) ) ;
#12168 = ORIENTED_EDGE ( 'NONE', *, *, #22090, .F. ) ;
#12169 = CARTESIAN_POINT ( 'NONE',  ( -2.265401668238145483, -39.53028715828216377, 25.45016726748356817 ) ) ;
#12171 = FACE_OUTER_BOUND ( 'NONE', #14474, .T. ) ;
#12170 = DIRECTION ( 'NONE',  ( 0.000000000000000000, 1.000000000000000000, 0.000000000000000000 ) ) ;
#12172 = CARTESIAN_POINT ( 'NONE',  ( -6.574463467970648622, -20.55340846381166742, -47.03022655117394635 ) ) ;
#12173 = CARTESIAN_POINT ( 'NONE',  ( 2.430230287190581429, -116.8646894862406214, -86.70145658344777928 ) ) ;
#12174 = VERTEX_POINT ( 'NONE', #17296 ) ;
#12175 = ORIENTED_EDGE ( 'NONE', *, *, #23260, .F. ) ;
#12176 = DIRECTION ( 'NONE',  ( 0.000000000000000000, 0.000000000000000000, 1.000000000000000000 ) ) ;
#12177 = CARTESIAN_POINT ( 'NONE',  ( 26.11404676487257603, 36.06104232266594067, -107.3263591096426666 ) ) ;
#12178 = CARTESIAN_POINT ( 'NONE',  ( 5.340103579038194326, -84.79482754232353159, 120.6284720963482755 ) ) ;
#12179 = CARTESIAN_POINT ( 'NONE',  ( 109.1624594426973118, 0.001206615835669453849, -0.01591840958353240090 ) ) ;
#12180 = CARTESIAN_POINT ( 'NONE',  ( -25.21435515916025594, 1.749597353048488237E-16, -4.373993382621220594E-17 ) ) ;
#12181 = ORIENTED_EDGE ( 'NONE', *, *, #19272, .T. ) ;
#12182 = ORIENTED_EDGE ( 'NONE', *, *, #6532, .T. ) ;
#12183 = CARTESIAN_POINT ( 'NONE',  ( -55.24271866751342941, -0.009388511352199774979, 0.001425019990778928110 ) ) ;
#12184 = EDGE_CURVE ( 'NONE', #15111, #21211, #17033, .T. ) ;
#12185 = ORIENTED_EDGE ( 'NONE', *, *, #939, .F. ) ;
#12186 = FACE_OUTER_BOUND ( 'NONE', #9216, .T. ) ;
#12187 = CARTESIAN_POINT ( 'NONE',  ( -22.34422965417125795, 33.39267070835848017, 17.95715691811010828 ) ) ;
#12188 = EDGE_CURVE ( 'NONE', #19755, #10995, #21620, .T. ) ;
#12189 = CARTESIAN_POINT ( 'NONE',  ( 0.000000000000000000, 0.000000000000000000, 0.000000000000000000 ) ) ;
#12190 =( BOUNDED_SURFACE ( )  B_SPLINE_SURFACE ( 3, 1, ( 
 ( #225, #6428 ),
 ( #15325, #13307 ),
 ( #15043, #19516 ),
 ( #2513, #22256 ) ),
 .UNSPECIFIED., .F., .F., .F. ) 
 B_SPLINE_SURFACE_WITH_KNOTS ( ( 4, 4 ),
 ( 2, 2 ),
 ( 0.000000000000000000, 1.000000000000000000 ),
 ( 0.000000000000000000, 1.000000000000000000 ),
 .UNSPECIFIED. ) 
 GEOMETRIC_REPRESENTATION_ITEM ( )  RATIONAL_B_SPLINE_SURFACE ( (
 ( 1.000000000000000000, 1.000000000000000000),
 ( 0.9934239774497837239, 0.8357310067453919133),
 ( 0.9934239774497837239, 0.8357310067453919133),
 ( 1.000000000000000000, 1.000000000000000000) ) ) 
 REPRESENTATION_ITEM ( '' )  SURFACE ( )  );
#12191 = CARTESIAN_POINT ( 'NONE',  ( -55.24390624410018802, -0.009374879212966679906, -0.004572280736703028189 ) ) ;
#12192 = ADVANCED_FACE ( 'NONE', ( #4202 ), #8011, .F. ) ;
#12193 = DIRECTION ( 'NONE',  ( 0.5946245182733607137, 0.3297108033645267944, -0.7332888028688915316 ) ) ;
#12194 = CARTESIAN_POINT ( 'NONE',  ( 109.1589550718175161, -0.007359857714025710984, 0.001793588804100470059 ) ) ;
#12195 = LINE ( 'NONE', #27442, #28088 ) ;
#12196 = ORIENTED_EDGE ( 'NONE', *, *, #16820, .T. ) ;
#12197 = EDGE_CURVE ( 'NONE', #9317, #26534, #23746, .T. ) ;
#12198 = CARTESIAN_POINT ( 'NONE',  ( 109.1624594426973118, 0.01570508117120617345, 0.002863932759303145122 ) ) ;
#12200 = CARTESIAN_POINT ( 'NONE',  ( -1.048171036023507252, 43.86077206077069235, -13.17819047681618372 ) ) ;
#12199 = CARTESIAN_POINT ( 'NONE',  ( 1.833721034905648084, 85.00517831633841581, -117.6051524288275232 ) ) ;
#12201 = DIRECTION ( 'NONE',  ( 0.000000000000000000, 0.000000000000000000, -1.000000000000000000 ) ) ;
#12202 = EDGE_LOOP ( 'NONE', ( #25522, #12453, #15742, #17600 ) ) ;
#12203 = ORIENTED_EDGE ( 'NONE', *, *, #16617, .F. ) ;
#12204 = ORIENTED_EDGE ( 'NONE', *, *, #19599, .F. ) ;
#12205 = CARTESIAN_POINT ( 'NONE',  ( 19.66333377628728485, 77.29039328249602647, 114.0223162644902004 ) ) ;
#12207 = DIRECTION ( 'NONE',  ( 0.000000000000000000, 5.223019709708233256E-21, -1.000000000000000000 ) ) ;
#12206 = CARTESIAN_POINT ( 'NONE',  ( 25.64681081121879203, 112.9102952884414464, -0.4157506337731811663 ) ) ;
#12208 = CARTESIAN_POINT ( 'NONE',  ( -20.20700224038492721, 27.82980252387819675, -10.08426345511598932 ) ) ;
#12209 = CARTESIAN_POINT ( 'NONE',  ( 1.833721034905658520, -132.7087680342064004, -58.69612512971738028 ) ) ;
#12210 = VERTEX_POINT ( 'NONE', #28096 ) ;
#12211 = CARTESIAN_POINT ( 'NONE',  ( -1.031422197589716205, -28.14735071801769095, -36.13727897780117360 ) ) ;
#12212 = CARTESIAN_POINT ( 'NONE',  ( 25.64708228042117710, 45.96113332231483639, -103.1335618347708021 ) ) ;
#12213 = VERTEX_POINT ( 'NONE', #1899 ) ;
#12214 = CARTESIAN_POINT ( 'NONE',  ( -1.323830074806768398, -43.04593525292981582, -16.42382241777520946 ) ) ;
#12215 = LINE ( 'NONE', #1553, #21216 ) ;
#12216 = CARTESIAN_POINT ( 'NONE',  ( 109.1721716018069515, -0.003350975118860853846, -0.01673651515802107581 ) ) ;
#12217 = CARTESIAN_POINT ( 'NONE',  ( 30.59141879584319312, 88.14706749784174633, -75.73279557183218458 ) ) ;
#12218 = CARTESIAN_POINT ( 'NONE',  ( 1.831572820252008738, -71.69925593429721289, -126.1609924456737133 ) ) ;
#12219 = CARTESIAN_POINT ( 'NONE',  ( -12.94347594948481373, -23.08810053288719999, -42.93165645342850212 ) ) ;
#12220 = LINE ( 'NONE', #7483, #5938 ) ;
#12221 = ORIENTED_EDGE ( 'NONE', *, *, #18702, .T. ) ;
#12222 = CARTESIAN_POINT ( 'NONE',  ( 32.73300124599738581, 51.32617430725051832, -105.8473486001045387 ) ) ;
#12223 = CARTESIAN_POINT ( 'NONE',  ( 25.87036335909426654, 110.3794299719623524, -24.47383578007024241 ) ) ;
#12224 = CARTESIAN_POINT ( 'NONE',  ( 109.1587776205901577, -0.004375189885414207044, 0.005880209827416975170 ) ) ;
#12225 = EDGE_LOOP ( 'NONE', ( #12168, #17436, #7724, #4381 ) ) ;
#12226 = CARTESIAN_POINT ( 'NONE',  ( -1.049819825607602342, 36.75053263699390271, -27.33096219556254169 ) ) ;
#12227 = ORIENTED_EDGE ( 'NONE', *, *, #8024, .F. ) ;
#12228 = EDGE_CURVE ( 'NONE', #15588, #182, #19579, .T. ) ;
#12229 = B_SPLINE_CURVE_WITH_KNOTS ( 'NONE', 3,
 ( #13164, #21953, #6710, #12874, #21669, #4679 ),
 .UNSPECIFIED., .F., .F.,
 ( 4, 2, 4 ),
 ( 1.734723475976806902E-18, 0.0004335151646191491353, 0.0008670303292382965359 ),
 .UNSPECIFIED. ) ;
#12230 = EDGE_CURVE ( 'NONE', #4452, #6648, #11317, .T. ) ;
#12231 = CARTESIAN_POINT ( 'NONE',  ( -1.056502255334264895, 26.51074901220504643, -37.35734037467642565 ) ) ;
#12232 = CARTESIAN_POINT ( 'NONE',  ( -1.048994561756802169, -43.31369460697986540, -14.87838255483240246 ) ) ;
#12233 =( BOUNDED_SURFACE ( )  B_SPLINE_SURFACE ( 3, 1, ( 
 ( #14491, #16665 ),
 ( #5734, #10048 ),
 ( #5430, #20833 ),
 ( #28006, #10199 ) ),
 .UNSPECIFIED., .F., .F., .F. ) 
 B_SPLINE_SURFACE_WITH_KNOTS ( ( 4, 4 ),
 ( 2, 2 ),
 ( 0.000000000000000000, 1.000000000000000000 ),
 ( 0.000000000000000000, 1.000000000000000000 ),
 .UNSPECIFIED. ) 
 GEOMETRIC_REPRESENTATION_ITEM ( )  RATIONAL_B_SPLINE_SURFACE ( (
 ( 1.000000000000000000, 1.000000000000000000),
 ( 0.9934239774497837239, 0.8357310067453919133),
 ( 0.9934239774497837239, 0.8357310067453919133),
 ( 1.000000000000000000, 1.000000000000000000) ) ) 
 REPRESENTATION_ITEM ( '' )  SURFACE ( )  );
#12234 = EDGE_CURVE ( 'NONE', #11877, #3600, #9290, .T. ) ;
#12235 = CARTESIAN_POINT ( 'NONE',  ( 109.1586900883932856, -0.006819617742892453323, 0.002109621908824125657 ) ) ;
#12236 = CARTESIAN_POINT ( 'NONE',  ( 1.833721034905666736, 137.8972080590637290, -45.17977675814169203 ) ) ;
#12237 = CARTESIAN_POINT ( 'NONE',  ( 25.69398547355841345, 75.02007992711823192, -84.42756928260500615 ) ) ;
#12238 = B_SPLINE_CURVE_WITH_KNOTS ( 'NONE', 3,
 ( #21574, #1710, #21298, #4016, #10244, #27912, #1580, #25636, #10508, #14672 ),
 .UNSPECIFIED., .F., .F.,
 ( 4, 2, 2, 2, 4 ),
 ( 0.000000000000000000, 0.0003346267210630921333, 0.0006692534421261842666, 0.001003880163189276292, 0.001338506884252368533 ),
 .UNSPECIFIED. ) ;
#12239 = CARTESIAN_POINT ( 'NONE',  ( 1.833838850855487257, -125.6242502389381173, -72.63194208529603202 ) ) ;
#12240 = CARTESIAN_POINT ( 'NONE',  ( -20.37983603106074426, -27.81368274044719868, -10.62371319148630455 ) ) ;
#12241 = ORIENTED_EDGE ( 'NONE', *, *, #1846, .F. ) ;
#12242 = VERTEX_POINT ( 'NONE', #22195 ) ;
#12243 = CARTESIAN_POINT ( 'NONE',  ( 109.1586059443104944, 0.001198897580748340026, 0.006971743774738788611 ) ) ;
#12244 = CARTESIAN_POINT ( 'NONE',  ( -1.044556982611281493, 43.01635920718349126, -15.70482750345250267 ) ) ;
#12245 = CARTESIAN_POINT ( 'NONE',  ( 13.36082413113061307, 137.0038452127800213, 67.94366799842862292 ) ) ;
#12246 = CARTESIAN_POINT ( 'NONE',  ( 25.64708228042119131, -83.88307475436008076, -75.58165863986127420 ) ) ;
#12247 = CARTESIAN_POINT ( 'NONE',  ( 8.186469777910954093, 108.6390983781771098, -102.4860666868853656 ) ) ;
#12248 = CARTESIAN_POINT ( 'NONE',  ( 10.93730112725970827, 42.00474393596263667, 145.2260730187401236 ) ) ;
#12249 = ORIENTED_EDGE ( 'NONE', *, *, #20765, .T. ) ;
#12250 = CARTESIAN_POINT ( 'NONE',  ( 1.833838850093414186, -144.3148362521194770, 15.16810397409735423 ) ) ;
#12251 = CARTESIAN_POINT ( 'NONE',  ( -21.81686047589426636, -27.83628745321466624, -26.62923599424956933 ) ) ;
#12252 = CARTESIAN_POINT ( 'NONE',  ( 2.430230287190589422, -96.28466919684173320, 109.1043569252011025 ) ) ;
#12253 = CARTESIAN_POINT ( 'NONE',  ( -20.20700224038492721, -24.51628800869059432, -16.58740185276701951 ) ) ;
#12254 = CARTESIAN_POINT ( 'NONE',  ( 25.64681081121879203, 0.4157506337743640534, -112.9102952884414464 ) ) ;
#12255 = CIRCLE ( 'NONE', #9928, 44.74884827092600403 ) ;
#12256 = ORIENTED_EDGE ( 'NONE', *, *, #21326, .F. ) ;
#12257 = CARTESIAN_POINT ( 'NONE',  ( 25.64708228042122329, -75.58165863986093314, 83.88307475436030813 ) ) ;
#12258 = CARTESIAN_POINT ( 'NONE',  ( 32.73300124599740002, 103.7392577722183660, -55.46353551261898218 ) ) ;
#12259 = EDGE_LOOP ( 'NONE', ( #5720, #17917, #18198, #27554 ) ) ;
#12260 = EDGE_LOOP ( 'NONE', ( #24723, #1656, #13188, #3966 ) ) ;
#12261 = VERTEX_POINT ( 'NONE', #6805 ) ;
#12262 = EDGE_CURVE ( 'NONE', #13553, #6393, #27102, .T. ) ;
#12263 = CARTESIAN_POINT ( 'NONE',  ( 2.433796855181205476, 28.83182736670536528, 142.6247129145649239 ) ) ;
#12264 = CARTESIAN_POINT ( 'NONE',  ( -8.786685647604885574, 6.096987947571466530E-17, -1.524246986892866633E-17 ) ) ;
#12265 = EDGE_CURVE ( 'NONE', #12820, #10995, #15807, .T. ) ;
#12266 = CARTESIAN_POINT ( 'NONE',  ( -8.786685647604885574, 6.096987947571466530E-17, -1.524246986892866633E-17 ) ) ;
#12267 = EDGE_CURVE ( 'NONE', #10482, #14469, #1376, .T. ) ;
#12268 = CARTESIAN_POINT ( 'NONE',  ( 1.832998868059890096, -107.4798986104853498, -97.49378069860902940 ) ) ;
#12269 = CARTESIAN_POINT ( 'NONE',  ( 26.11404676487257603, -98.61392875273325842, -55.62948129436350087 ) ) ;
#12270 = VERTEX_POINT ( 'NONE', #307 ) ;
#12271 = CARTESIAN_POINT ( 'NONE',  ( 25.64681081121879203, 107.5125461021407318, -34.49579773461672971 ) ) ;
#12272 = CARTESIAN_POINT ( 'NONE',  ( 10.93730112725971004, 51.37919228020272300, 142.1801301103785420 ) ) ;
#12273 = CARTESIAN_POINT ( 'NONE',  ( 30.59138290137908101, -26.79783179610930333, -113.0806461017757272 ) ) ;
#12274 = CARTESIAN_POINT ( 'NONE',  ( 25.64681081121880624, -75.86069728268932977, -83.63051021305977883 ) ) ;
#12275 = CARTESIAN_POINT ( 'NONE',  ( 1.833691583653510815, -141.8642667235906174, -30.51806994139743878 ) ) ;
#12276 = CARTESIAN_POINT ( 'NONE',  ( -1.583189561560252701, 44.83405390829673109, -11.94859433442916874 ) ) ;
#12277 = CARTESIAN_POINT ( 'NONE',  ( 2.263178607246686624, 16.59120332983143342, 144.4462811785176939 ) ) ;
#12278 = CARTESIAN_POINT ( 'NONE',  ( 109.1592201516379674, 0.007051465909552763651, -0.003476928926134732496 ) ) ;
#12279 = DIRECTION ( 'NONE',  ( 1.000000000000000000, -6.938893903907226837E-18, -5.541455922705464902E-20 ) ) ;
#12280 = CARTESIAN_POINT ( 'NONE',  ( 28.37644542392846958, 119.4444529625694287, -34.54617949427969847 ) ) ;
#12281 = ORIENTED_EDGE ( 'NONE', *, *, #20602, .F. ) ;
#12282 = CARTESIAN_POINT ( 'NONE',  ( 6.224689322667647851, 33.28770499679335160, 144.2687111683196406 ) ) ;
#12283 = VERTEX_POINT ( 'NONE', #26784 ) ;
#12284 = CARTESIAN_POINT ( 'NONE',  ( -20.24399999263415140, 7.930419334766598993, 28.55700515887712854 ) ) ;
#12285 = CARTESIAN_POINT ( 'NONE',  ( 2.430230287190572103, -60.50928654924845063, 132.3371620660948906 ) ) ;
#12286 = ORIENTED_EDGE ( 'NONE', *, *, #13025, .T. ) ;
#12287 = EDGE_LOOP ( 'NONE', ( #2501, #25475, #10734, #17432 ) ) ;
#12288 = ORIENTED_EDGE ( 'NONE', *, *, #3123, .T. ) ;
#12289 = B_SPLINE_CURVE_WITH_KNOTS ( 'NONE', 3,
 ( #23218, #14552, #8100, #7673, #3607, #16726, #5795 ),
 .UNSPECIFIED., .F., .F.,
 ( 4, 3, 4 ),
 ( 0.000000000000000000, 0.02398743853561319250, 0.04000277880656216700 ),
 .UNSPECIFIED. ) ;
#12290 = EDGE_CURVE ( 'NONE', #24693, #391, #27842, .T. ) ;
#12291 = CARTESIAN_POINT ( 'NONE',  ( -55.24390624410018802, 0.004896917417131886954, -0.009209468562452662738 ) ) ;
#12292 = CARTESIAN_POINT ( 'NONE',  ( -12.82751273423878757, -33.78816682541312844, -35.32125660155435298 ) ) ;
#12293 = LINE ( 'NONE', #20105, #8980 ) ;
#12294 = CARTESIAN_POINT ( 'NONE',  ( 9.884929003653608603, 144.4113244745777820, -42.50195158090882330 ) ) ;
#12295 = CARTESIAN_POINT ( 'NONE',  ( -55.24390624410018802, 0.004896917417128144288, 0.009209468562451129242 ) ) ;
#12296 = CARTESIAN_POINT ( 'NONE',  ( 10.93730112725932635, 0.000000000000000000, 0.000000000000000000 ) ) ;
#12297 = CARTESIAN_POINT ( 'NONE',  ( -2.904412668506655582, -44.35433137608953302, -17.42365698954681719 ) ) ;
#12298 = ORIENTED_EDGE ( 'NONE', *, *, #99, .F. ) ;
#12299 = ORIENTED_EDGE ( 'NONE', *, *, #11671, .F. ) ;
#12300 = CARTESIAN_POINT ( 'NONE',  ( -8.786685647604896232, 9.545808661481343549, 52.67761315067276229 ) ) ;
#12302 = CARTESIAN_POINT ( 'NONE',  ( 8.186469777910954093, 57.56191611950492160, -137.8131828745822247 ) ) ;
#12301 = CARTESIAN_POINT ( 'NONE',  ( -4.178947244162533714, -41.47292084251643729, -25.96944194166775333 ) ) ;
#12303 = CARTESIAN_POINT ( 'NONE',  ( 32.73300124599738581, -39.98094346392232268, -110.6325518752277759 ) ) ;
#12304 = B_SPLINE_CURVE_WITH_KNOTS ( 'NONE', 3,
 ( #13819, #21440, #3744, #3595, #28053, #27635, #12514, #8492, #1850, #19008 ),
 .UNSPECIFIED., .F., .F.,
 ( 4, 2, 2, 2, 4 ),
 ( 1.301042606982605321E-18, 0.0003346267210630944101, 0.0006692534421261875192, 0.001003880163189280628, 0.001338506884252373737 ),
 .UNSPECIFIED. ) ;
#12305 = CARTESIAN_POINT ( 'NONE',  ( 109.1589550718174877, -0.003284595046925705905, 0.006826119083824063426 ) ) ;
#12306 = ORIENTED_EDGE ( 'NONE', *, *, #15511, .T. ) ;
#12307 = CARTESIAN_POINT ( 'NONE',  ( -28.13707043255157103, 21.52861750560939313, -7.802116958609079056 ) ) ;
#12308 = CARTESIAN_POINT ( 'NONE',  ( -55.24390624410018802, 0.007245494385991800047, -0.007503127514277958821 ) ) ;
#12309 = FACE_OUTER_BOUND ( 'NONE', #26059, .T. ) ;
#12310 = VERTEX_POINT ( 'NONE', #20310 ) ;
#12311 = CARTESIAN_POINT ( 'NONE',  ( 9.884929003653608603, -148.0628878137282243, 27.17402761732295957 ) ) ;
#12312 = CARTESIAN_POINT ( 'NONE',  ( 109.1592201516379674, 0.005485778713202931790, 0.005631912476303835985 ) ) ;
#12313 = EDGE_CURVE ( 'NONE', #27728, #1601, #23048, .T. ) ;
#12314 = ORIENTED_EDGE ( 'NONE', *, *, #10736, .F. ) ;
#12315 = EDGE_LOOP ( 'NONE', ( #23528, #11071, #7477, #9671 ) ) ;
#12316 = EDGE_CURVE ( 'NONE', #15270, #20885, #23377, .T. ) ;
#12317 = EDGE_CURVE ( 'NONE', #9129, #26116, #25019, .T. ) ;
#12318 = CARTESIAN_POINT ( 'NONE',  ( 1.894214914920927972, -86.08679174687999591, -116.8658096527531853 ) ) ;
#12319 = ORIENTED_EDGE ( 'NONE', *, *, #3934, .T. ) ;
#12320 = CARTESIAN_POINT ( 'NONE',  ( -1.113548883309555482, -42.96943836789115778, -16.03115934825511957 ) ) ;
#12321 = FACE_OUTER_BOUND ( 'NONE', #22959, .T. ) ;
#12322 = CARTESIAN_POINT ( 'NONE',  ( -1.583189561560253589, 46.33203782964461936, -2.490696082060032790 ) ) ;
#12323 = FACE_OUTER_BOUND ( 'NONE', #2096, .T. ) ;
#12324 = CARTESIAN_POINT ( 'NONE',  ( 32.73300124599740002, 116.5274707358857142, -16.10546300444702794 ) ) ;
#12325 = CARTESIAN_POINT ( 'NONE',  ( -25.21435515916025594, 1.749597353048488237E-16, -4.373993382621220594E-17 ) ) ;
#12326 = CARTESIAN_POINT ( 'NONE',  ( -20.20700224038492721, 27.82980252387819675, -10.08426345511598932 ) ) ;
#12327 = VERTEX_POINT ( 'NONE', #4628 ) ;
#12328 = CARTESIAN_POINT ( 'NONE',  ( 26.11404676487257603, -74.91683232331033082, 84.89295829319468112 ) ) ;
#12330 = CARTESIAN_POINT ( 'NONE',  ( -1.464342487929859660, -46.14921266389556820, 2.431462367721817230 ) ) ;
#12329 = CARTESIAN_POINT ( 'NONE',  ( 26.28373643307406127, -127.2291519022770672, -9.189598927293246788 ) ) ;
#12331 = CARTESIAN_POINT ( 'NONE',  ( -1.045287976400383290, 28.14015102489806708, -36.12803364096618708 ) ) ;
#12332 = ORIENTED_EDGE ( 'NONE', *, *, #27976, .T. ) ;
#12333 = ORIENTED_EDGE ( 'NONE', *, *, #21591, .T. ) ;
#12334 = ORIENTED_EDGE ( 'NONE', *, *, #3131, .T. ) ;
#12335 = CARTESIAN_POINT ( 'NONE',  ( 55.79472521941426777, -69.41463258328526820, 21.78881894124680230 ) ) ;
#12336 = B_SPLINE_CURVE_WITH_KNOTS ( 'NONE', 3,
 ( #1241, #22861, #3121, #25149, #5418, #3831, #12597, #21387 ),
 .UNSPECIFIED., .F., .F.,
 ( 4, 2, 2, 4 ),
 ( 0.000000000000000000, 0.0002429588503611243848, 0.0004859177007222487696, 0.0009718354014444800836 ),
 .UNSPECIFIED. ) ;
#12337 = DIRECTION ( 'NONE',  ( 0.000000000000000000, 0.000000000000000000, 1.000000000000000000 ) ) ;
#12339 = CARTESIAN_POINT ( 'NONE',  ( -55.24271866751342941, -0.004256484107792937385, -0.008488649505346276131 ) ) ;
#12338 = LINE ( 'NONE', #6170, #20806 ) ;
#12340 = CARTESIAN_POINT ( 'NONE',  ( 19.66333377628707524, 51.89484018353834927, 127.6002314355559122 ) ) ;
#12341 = CARTESIAN_POINT ( 'NONE',  ( -15.02187109954785527, 32.04062513125116141, -33.49412687891580021 ) ) ;
#12342 = EDGE_LOOP ( 'NONE', ( #23785, #23266, #12619, #10368 ) ) ;
#12343 = CARTESIAN_POINT ( 'NONE',  ( -1.045287976400383290, 12.68782741917383738, 44.00138577190627842 ) ) ;
#12344 = CARTESIAN_POINT ( 'NONE',  ( -1.155001620486255209, -44.25209926692301110, 12.20337535396725492 ) ) ;
#12345 = ORIENTED_EDGE ( 'NONE', *, *, #6565, .F. ) ;
#12346 = FACE_OUTER_BOUND ( 'NONE', #11802, .T. ) ;
#12347 = CARTESIAN_POINT ( 'NONE',  ( 55.49584447822657296, -0.2676470673961756641, 72.55110015779771970 ) ) ;
#12348 = CARTESIAN_POINT ( 'NONE',  ( -20.20700224038492721, -10.08426345511609235, -27.82980252387815767 ) ) ;
#12349 = ADVANCED_FACE ( 'NONE', ( #9240 ), #2912, .T. ) ;
#12350 = CARTESIAN_POINT ( 'NONE',  ( 2.430230287190592531, 96.28466919684248637, -109.1043569252004488 ) ) ;
#12351 = CARTESIAN_POINT ( 'NONE',  ( 2.433796855181233454, 71.49415740225254012, -126.7346379669248222 ) ) ;
#12352 = CARTESIAN_POINT ( 'NONE',  ( 25.70243777736187951, -110.6300896395618736, 22.76560620137025737 ) ) ;
#12353 = CARTESIAN_POINT ( 'NONE',  ( 25.64681081121879203, -84.18689316039996129, -75.24277141833577787 ) ) ;
#12354 = VERTEX_POINT ( 'NONE', #19734 ) ;
#12355 = FACE_OUTER_BOUND ( 'NONE', #6492, .T. ) ;
#12357 = EDGE_CURVE ( 'NONE', #9135, #8797, #17577, .T. ) ;
#12356 = CARTESIAN_POINT ( 'NONE',  ( -20.57838717382308147, -1.611677988432151709, 29.92853265176832878 ) ) ;
#12358 = CARTESIAN_POINT ( 'NONE',  ( 21.16825799904895078, 121.8625396241606182, -59.09063383105223011 ) ) ;
#12359 =( BOUNDED_SURFACE ( )  B_SPLINE_SURFACE ( 3, 1, ( 
 ( #11109, #19879 ),
 ( #7199, #20699 ),
 ( #5161, #13 ),
 ( #16243, #25050 ) ),
 .UNSPECIFIED., .F., .F., .F. ) 
 B_SPLINE_SURFACE_WITH_KNOTS ( ( 4, 4 ),
 ( 2, 2 ),
 ( 0.000000000000000000, 1.000000000000000000 ),
 ( 0.000000000000000000, 1.000000000000000000 ),
 .UNSPECIFIED. ) 
 GEOMETRIC_REPRESENTATION_ITEM ( )  RATIONAL_B_SPLINE_SURFACE ( (
 ( 1.000000000000000000, 1.000000000000000000),
 ( 0.9960225298536222738, 0.9999952330161893110),
 ( 0.9960225298536222738, 0.9999952330161893110),
 ( 1.000000000000000000, 1.000000000000000000) ) ) 
 REPRESENTATION_ITEM ( '' )  SURFACE ( )  );
#12360 = ORIENTED_EDGE ( 'NONE', *, *, #9890, .T. ) ;
#12361 = CARTESIAN_POINT ( 'NONE',  ( -55.24390624410018802, 0.009374879212967415429, 0.004572280736702902422 ) ) ;
#12362 = CARTESIAN_POINT ( 'NONE',  ( -55.24271866751342941, -0.001425019990781919424, 0.009388511352197656881 ) ) ;
#12363 = CARTESIAN_POINT ( 'NONE',  ( -1.619063947482197729, -35.99532424477401094, -29.22875152547743838 ) ) ;
#12364 = CARTESIAN_POINT ( 'NONE',  ( -1.050230346682671678, -14.15335421912552860, 43.55729751025877761 ) ) ;
#12365 = CARTESIAN_POINT ( 'NONE',  ( 25.64700659047695552, -23.69811251893808901, 110.3963107228935741 ) ) ;
#12366 = CARTESIAN_POINT ( 'NONE',  ( 1.833691583653536350, 138.1170938425798056, -44.50270951807404174 ) ) ;
#12367 = CARTESIAN_POINT ( 'NONE',  ( 32.73300124599735739, -55.46353551262085091, 103.7392577722174565 ) ) ;
#12368 = CARTESIAN_POINT ( 'NONE',  ( -55.25297051322618813, 0.001818774723749727032, -0.01483298743815054943 ) ) ;
#12369 = CARTESIAN_POINT ( 'NONE',  ( 25.64703792032470275, 112.2770217641849655, -11.95040607427869261 ) ) ;
#12370 = CARTESIAN_POINT ( 'NONE',  ( 1.893872463202024736, -16.11957794552867540, 144.2520230501565663 ) ) ;
#12371 = ORIENTED_EDGE ( 'NONE', *, *, #15749, .T. ) ;
#12372 = VERTEX_POINT ( 'NONE', #22043 ) ;
#12373 = CARTESIAN_POINT ( 'NONE',  ( 109.1586900883932856, 0.002109621908824149943, 0.006819617742892446384 ) ) ;
#12374 = CARTESIAN_POINT ( 'NONE',  ( 2.433796855181205476, 107.1581411821785821, 98.43889364293895028 ) ) ;
#12375 = CARTESIAN_POINT ( 'NONE',  ( 25.64681081121879203, -83.63051021305953725, 75.86069728268962820 ) ) ;
#12376 = CARTESIAN_POINT ( 'NONE',  ( -1.464342487929860992, 11.94843286121917814, -44.64187261869783896 ) ) ;
#12377 = CARTESIAN_POINT ( 'NONE',  ( -25.21435515916025594, 1.749597353048488237E-16, -4.373993382621220594E-17 ) ) ;
#12378 = ORIENTED_EDGE ( 'NONE', *, *, #17705, .F. ) ;
#12379 = CARTESIAN_POINT ( 'NONE',  ( 109.1592201516379674, -0.007748443302128564178, 0.001331853079208289697 ) ) ;
#12380 = FACE_OUTER_BOUND ( 'NONE', #2490, .T. ) ;
#12381 = CARTESIAN_POINT ( 'NONE',  ( -20.57838717382308147, -23.26537097894118133, -18.89542499756491978 ) ) ;
#12382 = ADVANCED_FACE ( 'NONE', ( #2307 ), #16983, .F. ) ;
#12383 = EDGE_CURVE ( 'NONE', #22024, #10268, #16847, .T. ) ;
#12384 = CARTESIAN_POINT ( 'NONE',  ( 25.64660436782551756, 0.5800540083551843917, 112.9095526718341489 ) ) ;
#12385 = CARTESIAN_POINT ( 'NONE',  ( 1.832998868059858122, 0.5339089137748035396, 145.1092030902949830 ) ) ;
#12386 = ORIENTED_EDGE ( 'NONE', *, *, #25940, .F. ) ;
#12388 = EDGE_CURVE ( 'NONE', #28027, #7211, #14066, .T. ) ;
#12387 = CARTESIAN_POINT ( 'NONE',  ( 2.433796855181233454, -46.34326152018648060, -137.9325382748289996 ) ) ;
#12389 = CARTESIAN_POINT ( 'NONE',  ( -8.786685647604885574, 6.617461520090397715E-15, -53.53553390275978785 ) ) ;
#12390 = VERTEX_POINT ( 'NONE', #9825 ) ;
#12391 = EDGE_CURVE ( 'NONE', #19494, #13159, #3116, .T. ) ;
#12392 = ORIENTED_EDGE ( 'NONE', *, *, #26251, .F. ) ;
#12393 = ORIENTED_EDGE ( 'NONE', *, *, #8549, .F. ) ;
#12394 =( BOUNDED_SURFACE ( )  B_SPLINE_SURFACE ( 3, 1, ( 
 ( #15568, #2774 ),
 ( #324, #4650 ),
 ( #20183, #24536 ),
 ( #623, #5071 ) ),
 .UNSPECIFIED., .F., .F., .F. ) 
 B_SPLINE_SURFACE_WITH_KNOTS ( ( 4, 4 ),
 ( 2, 2 ),
 ( 0.000000000000000000, 1.000000000000000000 ),
 ( 0.000000000000000000, 1.000000000000000000 ),
 .UNSPECIFIED. ) 
 GEOMETRIC_REPRESENTATION_ITEM ( )  RATIONAL_B_SPLINE_SURFACE ( (
 ( 1.000000000000000000, 1.000000000000000000),
 ( 0.9956975270656955868, 0.8568959468854907557),
 ( 0.9956975270656955868, 0.8568959468854907557),
 ( 1.000000000000000000, 1.000000000000000000) ) ) 
 REPRESENTATION_ITEM ( '' )  SURFACE ( )  );
#12395 = CARTESIAN_POINT ( 'NONE',  ( -55.25297051322618813, 0.01093108995494865114, -0.01019003092403491552 ) ) ;
#12396 = CARTESIAN_POINT ( 'NONE',  ( 24.01988960052061373, -125.8850824254503493, 36.40943914739857945 ) ) ;
#12397 = CARTESIAN_POINT ( 'NONE',  ( -55.24728320129491266, 0.01214321324516798306, 0.008013189884950450148 ) ) ;
#12398 = CARTESIAN_POINT ( 'NONE',  ( 6.224689322667630975, 118.2566963816771022, 89.08920297664251109 ) ) ;
#12399 = ORIENTED_EDGE ( 'NONE', *, *, #27725, .F. ) ;
#12400 = CARTESIAN_POINT ( 'NONE',  ( -1.031422197589711764, 12.69107518035563587, 44.01264471863832739 ) ) ;
#12401 = CARTESIAN_POINT ( 'NONE',  ( 10.93730112726006354, 149.7554878793152966, -20.69552240458195413 ) ) ;
#12402 = CARTESIAN_POINT ( 'NONE',  ( -23.77929240705206482, 35.68044874544704470, 6.464423883190010933 ) ) ;
#12403 = CARTESIAN_POINT ( 'NONE',  ( 25.64692232868535982, -75.79483800045719022, -83.69035111837278862 ) ) ;
#12404 = CARTESIAN_POINT ( 'NONE',  ( 26.04756280548352976, -110.4687147111161636, 24.61655718144302796 ) ) ;
#12405 = CARTESIAN_POINT ( 'NONE',  ( 1.833838850855461056, -141.9202662332486113, -30.25705358194998240 ) ) ;
#12406 = CARTESIAN_POINT ( 'NONE',  ( 2.433796855181205476, 74.00833731765735024, -125.2830755159746445 ) ) ;
#12407 = EDGE_CURVE ( 'NONE', #2427, #18428, #6895, .T. ) ;
#12408 = CARTESIAN_POINT ( 'NONE',  ( 26.11404676487257603, -22.43340081644687345, -110.9778746459749499 ) ) ;
#12409 = CARTESIAN_POINT ( 'NONE',  ( 109.1589550718174877, -0.004900004919105039811, -0.005777059646704573760 ) ) ;
#12410 = CARTESIAN_POINT ( 'NONE',  ( 26.11404676487257603, -24.64483677384923865, 110.5078194225160360 ) ) ;
#12411 = CARTESIAN_POINT ( 'NONE',  ( -20.57838717382308147, -10.78122205916981358, 27.96569011373096814 ) ) ;
#12412 = VERTEX_POINT ( 'NONE', #7966 ) ;
#12413 = ORIENTED_EDGE ( 'NONE', *, *, #3144, .F. ) ;
#12415 = ADVANCED_FACE ( 'NONE', ( #11687 ), #9848, .F. ) ;
#12414 = CARTESIAN_POINT ( 'NONE',  ( -1.583189561560255143, -16.68617981233672509, 43.29471907393757846 ) ) ;
#12417 = ORIENTED_EDGE ( 'NONE', *, *, #8839, .T. ) ;
#12416 = CARTESIAN_POINT ( 'NONE',  ( -1.048171036023513247, 26.08692787913922473, 37.64178826568577563 ) ) ;
#12418 = ORIENTED_EDGE ( 'NONE', *, *, #1341, .F. ) ;
#12419 = B_SPLINE_CURVE_WITH_KNOTS ( 'NONE', 3,
 ( #2544, #1985, #17379, #15626, #15488, #10785, #8481, #9039, #24301, #19679 ),
 .UNSPECIFIED., .F., .F.,
 ( 4, 3, 3, 4 ),
 ( 1.387778780781445676E-17, 0.0002669560319015803866, 0.0005492286108966434053, 0.0008315040496093427293 ),
 .UNSPECIFIED. ) ;
#12420 = AXIS2_PLACEMENT_3D ( 'NONE', #17971, #9505, #24484 ) ;
#12421 = ORIENTED_EDGE ( 'NONE', *, *, #22315, .F. ) ;
#12422 = ORIENTED_EDGE ( 'NONE', *, *, #10816, .F. ) ;
#12423 = LINE ( 'NONE', #27835, #25782 ) ;
#12424 = CARTESIAN_POINT ( 'NONE',  ( 2.263178113027060956, -73.90841366068468687, 125.2099934853448389 ) ) ;
#12425 =( BOUNDED_SURFACE ( )  B_SPLINE_SURFACE ( 3, 1, ( 
 ( #6711, #6421 ),
 ( #1799, #12744 ),
 ( #28278, #17486 ),
 ( #21673, #6159 ) ),
 .UNSPECIFIED., .F., .F., .F. ) 
 B_SPLINE_SURFACE_WITH_KNOTS ( ( 4, 4 ),
 ( 2, 2 ),
 ( 0.000000000000000000, 1.000000000000000000 ),
 ( 0.000000000000000000, 1.000000000000000000 ),
 .UNSPECIFIED. ) 
 GEOMETRIC_REPRESENTATION_ITEM ( )  RATIONAL_B_SPLINE_SURFACE ( (
 ( 1.000000000000000000, 1.000000000000000000),
 ( 0.6386103224230302855, 0.9954351624131538845),
 ( 0.6386103224230302855, 0.9954351624131538845),
 ( 1.000000000000000000, 1.000000000000000000) ) ) 
 REPRESENTATION_ITEM ( '' )  SURFACE ( )  );
#12426 = CARTESIAN_POINT ( 'NONE',  ( 9.884929003653626367, 27.17402761732548555, -148.0628878137277979 ) ) ;
#12427 = CARTESIAN_POINT ( 'NONE',  ( -20.47566338032508426, 1.586617869344308041, 29.82700953060495408 ) ) ;
#12428 = VECTOR ( 'NONE', #15981, 1000.000000000000000 ) ;
#12429 = CARTESIAN_POINT ( 'NONE',  ( 32.73300124599736449, -66.00340565729409548, 97.37344512919831629 ) ) ;
#12430 = VECTOR ( 'NONE', #27515, 999.9999999999998863 ) ;
#12431 = CARTESIAN_POINT ( 'NONE',  ( 10.93730112725971360, 26.59437931460756488, 148.8212007290661916 ) ) ;
#12432 = CARTESIAN_POINT ( 'NONE',  ( 9.884929003653608603, -135.7578851563881983, -65.04493172071613571 ) ) ;
#12433 =( NAMED_UNIT ( * ) SI_UNIT ( $, .STERADIAN. ) SOLID_ANGLE_UNIT ( ) );
#12434 = AXIS2_PLACEMENT_3D ( 'NONE', #12957, #8517, #15248 ) ;
#12435 = ORIENTED_EDGE ( 'NONE', *, *, #8291, .T. ) ;
#12436 = ORIENTED_EDGE ( 'NONE', *, *, #7284, .F. ) ;
#12437 = CARTESIAN_POINT ( 'NONE',  ( -1.045287976400365970, -25.66401692419961833, 37.92705037016786918 ) ) ;
#12439 = DIRECTION ( 'NONE',  ( 0.7563875759206388771, -0.1685564395263385584, -0.6320336713238493553 ) ) ;
#12438 = CARTESIAN_POINT ( 'NONE',  ( 1.833206308920070082, 144.3905119031281856, -14.42724735286700088 ) ) ;
#12440 = EDGE_CURVE ( 'NONE', #23510, #7205, #4195, .T. ) ;
#12441 = CARTESIAN_POINT ( 'NONE',  ( -5.986830583229483693, -19.95149887249887399, -46.64941882410793283 ) ) ;
#12442 = CARTESIAN_POINT ( 'NONE',  ( -20.20700224038492721, 10.08426345511588984, -27.82980252387822517 ) ) ;
#12443 = DIRECTION ( 'NONE',  ( 0.000000000000000000, 0.000000000000000000, 1.000000000000000000 ) ) ;
#12444 = VERTEX_POINT ( 'NONE', #27361 ) ;
#12445 = CARTESIAN_POINT ( 'NONE',  ( -2.265401668238146815, -25.45016726748341540, -39.53028715828224904 ) ) ;
#12447 = EDGE_CURVE ( 'NONE', #22240, #11372, #26405, .T. ) ;
#12446 = CARTESIAN_POINT ( 'NONE',  ( -1.539763995773681504, 35.94321074656937753, 29.16712963492422617 ) ) ;
#12448 = CARTESIAN_POINT ( 'NONE',  ( 16.05277956358234803, 141.0713346807230266, 25.20902801311412844 ) ) ;
#12449 = VERTEX_POINT ( 'NONE', #21315 ) ;
#12450 = ORIENTED_EDGE ( 'NONE', *, *, #27691, .T. ) ;
#12451 = EDGE_CURVE ( 'NONE', #16711, #26886, #18879, .T. ) ;
#12452 = DIRECTION ( 'NONE',  ( -0.5914120900931443270, -0.4674599267565393013, 0.6570486713847228932 ) ) ;
#12453 = ORIENTED_EDGE ( 'NONE', *, *, #25433, .F. ) ;
#12454 = ORIENTED_EDGE ( 'NONE', *, *, #7172, .F. ) ;
#12455 = CONICAL_SURFACE ( 'NONE', #24405, 117.6351876552689504, 0.9945805576725580410 ) ;
#12456 = VECTOR ( 'NONE', #16627, 1000.000000000000227 ) ;
#12457 = CARTESIAN_POINT ( 'NONE',  ( 109.1721716018069515, -0.01706748904931388797, -0.0002019688922687420615 ) ) ;
#12458 = AXIS2_PLACEMENT_3D ( 'NONE', #14017, #20639, #3092 ) ;
#12459 = EDGE_LOOP ( 'NONE', ( #27007, #22594, #3191, #26051 ) ) ;
#12460 = CARTESIAN_POINT ( 'NONE',  ( 1.832998868059890096, -144.2584710144581663, 15.69902610990327574 ) ) ;
#12461 = CARTESIAN_POINT ( 'NONE',  ( 16.05277956358208868, -67.56865019683935714, 126.3767940428302552 ) ) ;
#12462 = B_SPLINE_CURVE_WITH_KNOTS ( 'NONE', 3,
 ( #27070, #11836, #7107, #7378 ),
 .UNSPECIFIED., .F., .F.,
 ( 4, 4 ),
 ( 3.076313952674417705E-16, 0.01077107486149805025 ),
 .UNSPECIFIED. ) ;
#12463 = DIRECTION ( 'NONE',  ( 0.7637818620346800147, -0.5345501402766247301, 0.3617919495470812152 ) ) ;
#12464 = DIRECTION ( 'NONE',  ( -1.000000000000000000, -0.000000000000000000, -0.000000000000000000 ) ) ;
#12465 = CARTESIAN_POINT ( 'NONE',  ( 25.73574536432417403, -46.68445899255561926, 102.8730547980548522 ) ) ;
#12466 = CARTESIAN_POINT ( 'NONE',  ( 1.833485406944057594, -108.1939177044919376, -96.69979900902278303 ) ) ;
#12467 = VERTEX_POINT ( 'NONE', #28067 ) ;
#12468 = EDGE_CURVE ( 'NONE', #21344, #18869, #23685, .T. ) ;
#12469 = CARTESIAN_POINT ( 'NONE',  ( 5.340103556456481826, -143.7310399800115874, -32.90561046456862471 ) ) ;
#12471 = CARTESIAN_POINT ( 'NONE',  ( 1.833485406944043827, -107.4794113447402566, -97.49333871408801144 ) ) ;
#12470 = CARTESIAN_POINT ( 'NONE',  ( 1.833838850855463720, 85.36536653357504179, -117.3439621615255675 ) ) ;
#12472 = CARTESIAN_POINT ( 'NONE',  ( -1.045287976400383290, -12.68782741917353185, -44.00138577190637079 ) ) ;
#12473 = ORIENTED_EDGE ( 'NONE', *, *, #8523, .T. ) ;
#12474 = ORIENTED_EDGE ( 'NONE', *, *, #16511, .F. ) ;
#12475 = CARTESIAN_POINT ( 'NONE',  ( -20.21097721712958872, 8.835581498567860237, 28.26295595852175779 ) ) ;
#12476 = CARTESIAN_POINT ( 'NONE',  ( 109.1586900883932856, 0.002995460350188396646, 0.006479576224398257700 ) ) ;
#12478 = CARTESIAN_POINT ( 'NONE',  ( 25.86096068574580897, -98.40249579084552067, 55.66087367585372903 ) ) ;
#12477 = CARTESIAN_POINT ( 'NONE',  ( 32.73300124599734318, 16.10546300444822165, 116.5274707358856290 ) ) ;
#12479 = EDGE_CURVE ( 'NONE', #22454, #5205, #19878, .T. ) ;
#12480 = CARTESIAN_POINT ( 'NONE',  ( -20.38016308990359349, 27.81387210821422329, -10.62413300760995583 ) ) ;
#12481 = CARTESIAN_POINT ( 'NONE',  ( -40.00000000000000000, 0.000000000000000000, 0.000000000000000000 ) ) ;
#12482 = VERTEX_POINT ( 'NONE', #27932 ) ;
#12483 = CARTESIAN_POINT ( 'NONE',  ( -25.21435515916043713, -23.92354251275954979, -25.00736669481013053 ) ) ;
#12484 = DIRECTION ( 'NONE',  ( 1.000000000000000000, -6.938893903907226837E-18, 1.734723475976806709E-18 ) ) ;
#12485 = ORIENTED_EDGE ( 'NONE', *, *, #3812, .F. ) ;
#12486 = CARTESIAN_POINT ( 'NONE',  ( 10.93730112725990189, -148.8212007290660495, -26.59437931460901439 ) ) ;
#12487 = DIRECTION ( 'NONE',  ( 0.5946245182733607137, 0.002950380665390443108, -0.8039981203473692828 ) ) ;
#12488 = CIRCLE ( 'NONE', #21663, 117.6351876552689504 ) ;
#12489 = CARTESIAN_POINT ( 'NONE',  ( -1.048171036023517688, 15.11933492062827966, -43.23005599774305807 ) ) ;
#12490 = CARTESIAN_POINT ( 'NONE',  ( 2.433796855181219243, -43.58222566461740399, 138.8296532063086772 ) ) ;
#12491 = FACE_OUTER_BOUND ( 'NONE', #1904, .T. ) ;
#12492 = CARTESIAN_POINT ( 'NONE',  ( -6.588769196390762417, 44.25609997968906839, -26.02756986588556742 ) ) ;
#12493 = CARTESIAN_POINT ( 'NONE',  ( -20.57838717382308147, -1.611677988432151709, 29.92853265176832878 ) ) ;
#12494 = VERTEX_POINT ( 'NONE', #19435 ) ;
#12495 = CARTESIAN_POINT ( 'NONE',  ( 109.1624594426973118, -0.01591840958353240090, -0.001206615835669402025 ) ) ;
#12496 = CARTESIAN_POINT ( 'NONE',  ( 30.58324630866341209, 108.8243914523538223, -52.76949945162287037 ) ) ;
#12497 = ORIENTED_EDGE ( 'NONE', *, *, #8461, .F. ) ;
#12498 = CARTESIAN_POINT ( 'NONE',  ( 16.75465622695652712, -91.67104679059826822, -108.7410129416645077 ) ) ;
#12499 = CARTESIAN_POINT ( 'NONE',  ( -28.41354790283022069, 21.64275480268759821, 8.345538364876851745 ) ) ;
#12500 =( NAMED_UNIT ( * ) SI_UNIT ( $, .STERADIAN. ) SOLID_ANGLE_UNIT ( ) );
#12501 = AXIS2_PLACEMENT_3D ( 'NONE', #23247, #1203, #25250 ) ;
#12502 = CARTESIAN_POINT ( 'NONE',  ( 109.1586059443104944, -0.007068659269321313221, 0.0002768082440288505358 ) ) ;
#12503 = CARTESIAN_POINT ( 'NONE',  ( -25.21435515916043713, -15.02493970636168896, -31.17620025257581062 ) ) ;
#12504 = CARTESIAN_POINT ( 'NONE',  ( 25.64660436782542163, 75.12017330820604855, -84.29628170537191068 ) ) ;
#12505 = CARTESIAN_POINT ( 'NONE',  ( 2.433796855181233454, -74.00833731765476386, -125.2830755159761935 ) ) ;
#12506 = EDGE_CURVE ( 'NONE', #23219, #8435, #1674, .T. ) ;
#12507 = CARTESIAN_POINT ( 'NONE',  ( 32.73300124599739291, 92.86301839380121237, -72.21147546950456331 ) ) ;
#12508 = CARTESIAN_POINT ( 'NONE',  ( 1.833485406944057594, 145.1085452359073429, -0.5339064996889759662 ) ) ;
#12509 = VERTEX_POINT ( 'NONE', #19023 ) ;
#12510 = EDGE_CURVE ( 'NONE', #6049, #9341, #14725, .T. ) ;
#12511 = VERTEX_POINT ( 'NONE', #27804 ) ;
#12512 =( BOUNDED_SURFACE ( )  B_SPLINE_SURFACE ( 3, 1, ( 
 ( #16086, #3427 ),
 ( #692, #1126 ),
 ( #25310, #18235 ),
 ( #7324, #2854 ) ),
 .UNSPECIFIED., .F., .F., .F. ) 
 B_SPLINE_SURFACE_WITH_KNOTS ( ( 4, 4 ),
 ( 2, 2 ),
 ( 0.000000000000000000, 1.000000000000000000 ),
 ( 0.000000000000000000, 1.000000000000000000 ),
 .UNSPECIFIED. ) 
 GEOMETRIC_REPRESENTATION_ITEM ( )  RATIONAL_B_SPLINE_SURFACE ( (
 ( 1.000000000000000000, 1.000000000000000000),
 ( 0.9956975270656954757, 0.8568959468854893125),
 ( 0.9956975270656954757, 0.8568959468854893125),
 ( 1.000000000000000000, 1.000000000000000000) ) ) 
 REPRESENTATION_ITEM ( '' )  SURFACE ( )  );
#12513 = ORIENTED_EDGE ( 'NONE', *, *, #193, .T. ) ;
#12514 = CARTESIAN_POINT ( 'NONE',  ( -1.113427685306989767, -42.96952363574823863, 16.03057832159198171 ) ) ;
#12515 = CARTESIAN_POINT ( 'NONE',  ( 109.1592201516379674, 0.002134489919768143857, -0.007566779963325576466 ) ) ;
#12516 = CARTESIAN_POINT ( 'NONE',  ( 1.833206310202321498, 84.68961945193613872, -117.8322271314356016 ) ) ;
#12517 = CARTESIAN_POINT ( 'NONE',  ( 30.59138290137885008, -105.0379801549012058, 49.72302320601758652 ) ) ;
#12518 = CARTESIAN_POINT ( 'NONE',  ( -1.583189561560255143, -25.21827308671260326, -38.94740041318284796 ) ) ;
#12519 = CARTESIAN_POINT ( 'NONE',  ( 19.66333377628670576, 72.72773398758388907, -116.9853418557804901 ) ) ;
#12520 = CARTESIAN_POINT ( 'NONE',  ( -1.031422197589716205, -45.78027046666446154, -1.530725436377304183 ) ) ;
#12521 = ORIENTED_EDGE ( 'NONE', *, *, #15179, .F. ) ;
#12522 = CARTESIAN_POINT ( 'NONE',  ( 8.186469829614033245, 118.7566730983347725, 90.56875932797599660 ) ) ;
#12523 = CARTESIAN_POINT ( 'NONE',  ( -1.031422197589716205, -12.69107518035472637, 44.01264471863859740 ) ) ;
#12524 = DIRECTION ( 'NONE',  ( 0.000000000000000000, 0.000000000000000000, 1.000000000000000000 ) ) ;
#12526 =( BOUNDED_SURFACE ( )  B_SPLINE_SURFACE ( 3, 1, ( 
 ( #10850, #6528 ),
 ( #6385, #12426 ),
 ( #12842, #16902 ),
 ( #10434, #6251 ) ),
 .UNSPECIFIED., .F., .F., .F. ) 
 B_SPLINE_SURFACE_WITH_KNOTS ( ( 4, 4 ),
 ( 2, 2 ),
 ( 0.000000000000000000, 1.000000000000000000 ),
 ( 0.000000000000000000, 1.000000000000000000 ),
 .UNSPECIFIED. ) 
 GEOMETRIC_REPRESENTATION_ITEM ( )  RATIONAL_B_SPLINE_SURFACE ( (
 ( 1.000000000000000000, 1.000000000000000000),
 ( 0.6386103224230316178, 0.9954351624131538845),
 ( 0.6386103224230316178, 0.9954351624131538845),
 ( 1.000000000000000000, 1.000000000000000000) ) ) 
 REPRESENTATION_ITEM ( '' )  SURFACE ( )  );
#12525 = VECTOR ( 'NONE', #10640, 1000.000000000000114 ) ;
#12527 = CARTESIAN_POINT ( 'NONE',  ( 2.063896406836609909, 1.344106060020366256, 145.2631347824382715 ) ) ;
#12528 = VECTOR ( 'NONE', #4870, 1000.000000000000114 ) ;
#12529 = VERTEX_POINT ( 'NONE', #10811 ) ;
#12530 = CARTESIAN_POINT ( 'NONE',  ( -7.733045908741311258, -38.67583825854175217, -35.49239760110661024 ) ) ;
#12531 = CARTESIAN_POINT ( 'NONE',  ( 25.64692872815576408, -11.48248630407202775, -112.3258062264003314 ) ) ;
#12532 = ORIENTED_EDGE ( 'NONE', *, *, #5243, .F. ) ;
#12533 = B_SPLINE_CURVE_WITH_KNOTS ( 'NONE', 3,
 ( #14194, #7758, #16516, #20681, #4863, #13634 ),
 .UNSPECIFIED., .F., .F.,
 ( 4, 2, 4 ),
 ( 0.000000000000000000, 0.0004335184443140241905, 0.0008670368886280483810 ),
 .UNSPECIFIED. ) ;
#12534 = VERTEX_POINT ( 'NONE', #16992 ) ;
#12535 = ORIENTED_EDGE ( 'NONE', *, *, #9978, .T. ) ;
#12536 = B_SPLINE_CURVE_WITH_KNOTS ( 'NONE', 3,
 ( #28199, #4165, #13933, #11927, #7195, #22746 ),
 .UNSPECIFIED., .F., .F.,
 ( 4, 2, 4 ),
 ( 1.512296865354101973E-16, 0.003570751334075637860, 0.007141502668151123931 ),
 .UNSPECIFIED. ) ;
#12537 = CARTESIAN_POINT ( 'NONE',  ( 25.98107933586705443, -107.9289867379274597, 33.92073193606549353 ) ) ;
#12538 = CARTESIAN_POINT ( 'NONE',  ( 1.832998868059858122, -132.3466930259797891, 59.50898020732465454 ) ) ;
#12539 = EDGE_CURVE ( 'NONE', #7054, #15966, #27057, .T. ) ;
#12540 = ADVANCED_FACE ( 'NONE', ( #21171 ), #1184, .F. ) ;
#12541 = CARTESIAN_POINT ( 'NONE',  ( 2.108393763691196021, -133.2474712570797806, 57.92353377304240070 ) ) ;
#12542 = AXIS2_PLACEMENT_3D ( 'NONE', #27753, #14641, #3704 ) ;
#12543 = CARTESIAN_POINT ( 'NONE',  ( 109.1721716018069657, -0.008358834333183826765, 0.01488186354166055533 ) ) ;
#12544 = ORIENTED_EDGE ( 'NONE', *, *, #12317, .T. ) ;
#12545 = CARTESIAN_POINT ( 'NONE',  ( 109.1586900883932856, 0.003481399864227371996, 0.006231977675082120069 ) ) ;
#12546 = EDGE_CURVE ( 'NONE', #7068, #20579, #2694, .T. ) ;
#12547 = LINE ( 'NONE', #23663, #8831 ) ;
#12548 = CARTESIAN_POINT ( 'NONE',  ( 10.93730112726002979, 92.80059208661855052, -119.3442956573263558 ) ) ;
#12549 = EDGE_CURVE ( 'NONE', #16536, #12270, #419, .T. ) ;
#12550 = CARTESIAN_POINT ( 'NONE',  ( 109.1586059443104944, -0.007068659269322302013, -0.0002768082440195081284 ) ) ;
#12551 = CARTESIAN_POINT ( 'NONE',  ( -1.239374126674604337, 28.97829083655439675, -35.79060836339822060 ) ) ;
#12552 = CARTESIAN_POINT ( 'NONE',  ( 9.884929003653608603, 132.4189379373580664, -71.59798461011190795 ) ) ;
#12553 = FACE_OUTER_BOUND ( 'NONE', #23409, .T. ) ;
#12554 = FACE_OUTER_BOUND ( 'NONE', #21023, .T. ) ;
#12555 = CARTESIAN_POINT ( 'NONE',  ( 109.1778270068192853, -0.009177562596826690719, 0.001591747944959389944 ) ) ;
#12556 = CARTESIAN_POINT ( 'NONE',  ( -1.056502255334265339, -45.80535052436398757, -0.5104472526218417627 ) ) ;
#12557 = CARTESIAN_POINT ( 'NONE',  ( 26.28373643307407193, -100.6987277884689291, 78.30371666786361118 ) ) ;
#12558 = CARTESIAN_POINT ( 'NONE',  ( -19.53423201713129842, 1.550869255229030165E-16, 28.92774122539760384 ) ) ;
#12559 = ORIENTED_EDGE ( 'NONE', *, *, #28203, .T. ) ;
#12560 =( BOUNDED_SURFACE ( )  B_SPLINE_SURFACE ( 3, 1, ( 
 ( #2409, #13779 ),
 ( #22585, #5151 ),
 ( #15944, #15808 ),
 ( #17676, #26591 ) ),
 .UNSPECIFIED., .F., .F., .F. ) 
 B_SPLINE_SURFACE_WITH_KNOTS ( ( 4, 4 ),
 ( 2, 2 ),
 ( 0.000000000000000000, 1.000000000000000000 ),
 ( 0.000000000000000000, 1.000000000000000000 ),
 .UNSPECIFIED. ) 
 GEOMETRIC_REPRESENTATION_ITEM ( )  RATIONAL_B_SPLINE_SURFACE ( (
 ( 1.000000000000000000, 1.000000000000000000),
 ( 0.9956975270656955868, 0.8568959468854907557),
 ( 0.9956975270656955868, 0.8568959468854907557),
 ( 1.000000000000000000, 1.000000000000000000) ) ) 
 REPRESENTATION_ITEM ( '' )  SURFACE ( )  );
#12561 = VERTEX_POINT ( 'NONE', #22159 ) ;
#12562 = CARTESIAN_POINT ( 'NONE',  ( -1.323439229708135434, 38.58845475799802927, 25.17120723334049970 ) ) ;
#12564 = ORIENTED_EDGE ( 'NONE', *, *, #27284, .T. ) ;
#12563 = CARTESIAN_POINT ( 'NONE',  ( 24.22246935314087324, 90.00000000000005684, -40.00000000000000711 ) ) ;
#12565 = VERTEX_POINT ( 'NONE', #22311 ) ;
#12566 = EDGE_CURVE ( 'NONE', #194, #17492, #22660, .T. ) ;
#12567 = ORIENTED_EDGE ( 'NONE', *, *, #455, .F. ) ;
#12568 = VERTEX_POINT ( 'NONE', #9203 ) ;
#12569 = CARTESIAN_POINT ( 'NONE',  ( -1.048172774974290622, 43.86067135048637766, 13.17853518375252442 ) ) ;
#12570 = EDGE_CURVE ( 'NONE', #19470, #10229, #20283, .T. ) ;
#12571 = CARTESIAN_POINT ( 'NONE',  ( -1.619063947482201282, 43.26576862488434472, -16.67502769180576649 ) ) ;
#12572 = B_SPLINE_CURVE_WITH_KNOTS ( 'NONE', 3,
 ( #15211, #12778, #15071, #6323, #2249, #28178, #24164 ),
 .UNSPECIFIED., .F., .F.,
 ( 4, 3, 4 ),
 ( 0.000000000000000000, 0.006568092053401826565, 0.02506242213020857396 ),
 .UNSPECIFIED. ) ;
#12573 = LINE ( 'NONE', #10564, #7991 ) ;
#12574 = ADVANCED_FACE ( 'NONE', ( #24330 ), #9257, .T. ) ;
#12575 = CARTESIAN_POINT ( 'NONE',  ( 32.73300124599735739, 55.46353551262010484, 103.7392577722178260 ) ) ;
#12576 = CARTESIAN_POINT ( 'NONE',  ( 32.73300124599741423, 115.8010721414085822, -20.69176323058512423 ) ) ;
#12577 = ORIENTED_EDGE ( 'NONE', *, *, #7561, .F. ) ;
#12578 = ORIENTED_EDGE ( 'NONE', *, *, #10432, .F. ) ;
#12580 = CARTESIAN_POINT ( 'NONE',  ( -15.02187109954782507, -32.04062513125090561, 33.49412687891607021 ) ) ;
#12579 = CARTESIAN_POINT ( 'NONE',  ( -1.464342487929857439, 29.09292098541713401, 35.90631960086386698 ) ) ;
#12581 = CARTESIAN_POINT ( 'NONE',  ( -25.21435515916043713, -34.05351380035328646, 6.169479169075816394 ) ) ;
#12582 = DIRECTION ( 'NONE',  ( 1.000000000000000000, -6.938893903907226837E-18, 1.734723475976806709E-18 ) ) ;
#12583 = CARTESIAN_POINT ( 'NONE',  ( 25.98107933586699403, 90.88151529733809753, 67.37827847766564560 ) ) ;
#12584 = VERTEX_POINT ( 'NONE', #4591 ) ;
#12585 = CARTESIAN_POINT ( 'NONE',  ( 25.64703792032468499, 91.25955007190310653, -66.48786612795782958 ) ) ;
#12586 = CARTESIAN_POINT ( 'NONE',  ( -25.21435515916043713, 4.655591116594827383, 34.29329011225949841 ) ) ;
#12587 = CARTESIAN_POINT ( 'NONE',  ( -1.239374126674604337, 28.97829083655439675, -35.79060836339822060 ) ) ;
#12588 = ORIENTED_EDGE ( 'NONE', *, *, #2391, .F. ) ;
#12589 = ORIENTED_EDGE ( 'NONE', *, *, #24803, .T. ) ;
#12590 = B_SPLINE_CURVE_WITH_KNOTS ( 'NONE', 3,
 ( #7807, #1300, #21016, #22780, #5333, #16719, #1024, #27352, #8093, #18427, #27203, #3325, #9964 ),
 .UNSPECIFIED., .F., .F.,
 ( 4, 3, 3, 3, 4 ),
 ( 1.105886215935214523E-17, 0.0007657099931970556828, 0.001531419946797917854, 0.002296279302920152532, 0.003061450627205755497 ),
 .UNSPECIFIED. ) ;
#12591 = DIRECTION ( 'NONE',  ( 0.000000000000000000, 5.223019709707975211E-21, -1.000000000000000000 ) ) ;
#12592 = AXIS2_PLACEMENT_3D ( 'NONE', #11756, #5413, #14175 ) ;
#12593 = ORIENTED_EDGE ( 'NONE', *, *, #11998, .F. ) ;
#12594 =( BOUNDED_SURFACE ( )  B_SPLINE_SURFACE ( 3, 1, ( 
 ( #27306, #9345 ),
 ( #2852, #5002 ),
 ( #27160, #25167 ),
 ( #13926, #7187 ) ),
 .UNSPECIFIED., .F., .F., .F. ) 
 B_SPLINE_SURFACE_WITH_KNOTS ( ( 4, 4 ),
 ( 2, 2 ),
 ( 0.000000000000000000, 1.000000000000000000 ),
 ( 0.000000000000000000, 1.000000000000000000 ),
 .UNSPECIFIED. ) 
 GEOMETRIC_REPRESENTATION_ITEM ( )  RATIONAL_B_SPLINE_SURFACE ( (
 ( 1.000000000000000000, 1.000000000000000000),
 ( 0.7789835883360576307, 0.9689951854195403280),
 ( 0.7789835883360576307, 0.9689951854195403280),
 ( 1.000000000000000000, 1.000000000000000000) ) ) 
 REPRESENTATION_ITEM ( '' )  SURFACE ( )  );
#12595 = CARTESIAN_POINT ( 'NONE',  ( 2.430230287190592531, -142.6294793592095687, -28.83279105684573196 ) ) ;
#12596 = ORIENTED_EDGE ( 'NONE', *, *, #9276, .F. ) ;
#12597 = CARTESIAN_POINT ( 'NONE',  ( 25.98107933586740614, -45.01656174308500624, -103.7920584735896483 ) ) ;
#12598 = DIRECTION ( 'NONE',  ( 0.000000000000000000, 5.223019709707975211E-21, -1.000000000000000000 ) ) ;
#12599 = EDGE_CURVE ( 'NONE', #18219, #25686, #22285, .T. ) ;
#12600 = B_SPLINE_CURVE_WITH_KNOTS ( 'NONE', 3,
 ( #4720, #15937, #13921, #4862 ),
 .UNSPECIFIED., .F., .F.,
 ( 4, 4 ),
 ( 0.000000000000000000, 0.01077107196513801476 ),
 .UNSPECIFIED. ) ;
#12601 = CARTESIAN_POINT ( 'NONE',  ( -1.619063947482197729, -29.22875152547730337, 35.99532424477411041 ) ) ;
#12602 = EDGE_CURVE ( 'NONE', #17673, #24974, #4069, .T. ) ;
#12603 = CARTESIAN_POINT ( 'NONE',  ( 25.64681081121879203, -110.5293738517606954, -23.06870491922435207 ) ) ;
#12604 = CARTESIAN_POINT ( 'NONE',  ( 16.05277956358233027, 126.3767940428297578, 67.56865019683868923 ) ) ;
#12605 = CARTESIAN_POINT ( 'NONE',  ( -1.583189561560253589, 2.490696082060518624, 46.33203782964458384 ) ) ;
#12606 = DIRECTION ( 'NONE',  ( -0.5946245182733608248, 0.6977579871484534957, 0.3994439555666252639 ) ) ;
#12607 = EDGE_CURVE ( 'NONE', #4240, #27443, #3069, .T. ) ;
#12608 = CARTESIAN_POINT ( 'NONE',  ( 1.833750490713697445, 125.5350013574269781, 72.78591676343999950 ) ) ;
#12610 = LINE ( 'NONE', #8720, #8410 ) ;
#12609 = CARTESIAN_POINT ( 'NONE',  ( 25.64692872815576052, -97.62272225320907637, -56.73392579406814207 ) ) ;
#12611 = DIRECTION ( 'NONE',  ( -0.7563875759206388771, 0.6531865459554675457, -0.03500244528123232224 ) ) ;
#12612 = ORIENTED_EDGE ( 'NONE', *, *, #755, .T. ) ;
#12613 = VERTEX_POINT ( 'NONE', #6630 ) ;
#12614 = CARTESIAN_POINT ( 'NONE',  ( 25.64699802086722613, 56.24956056770159307, -97.90265915239973538 ) ) ;
#12615 = CARTESIAN_POINT ( 'NONE',  ( 1.832998868059890096, -14.63705790014106789, 144.3700883710216658 ) ) ;
#12616 = CARTESIAN_POINT ( 'NONE',  ( -20.20700224038492010, 27.82980252387833886, 10.08426345511560207 ) ) ;
#12617 = DIRECTION ( 'NONE',  ( 1.000000000000000000, -6.938893903907226837E-18, 1.734723475976806709E-18 ) ) ;
#12618 = CARTESIAN_POINT ( 'NONE',  ( 109.1586900883932856, 0.005371970278528643075, 0.004701023939945730111 ) ) ;
#12619 = ORIENTED_EDGE ( 'NONE', *, *, #14257, .F. ) ;
#12620 = CARTESIAN_POINT ( 'NONE',  ( -25.21435515916043713, -30.48034229288627017, 16.39063784838775462 ) ) ;
#12621 = CARTESIAN_POINT ( 'NONE',  ( 10.93730112725972070, -51.37919228020375328, 142.1801301103782293 ) ) ;
#12622 = VERTEX_POINT ( 'NONE', #15381 ) ;
#12623 = CARTESIAN_POINT ( 'NONE',  ( -1.031422197589711764, 1.530725436377463389, -45.78027046666443312 ) ) ;
#12624 = CARTESIAN_POINT ( 'NONE',  ( 1.834118845439484335, 141.9759513273464790, 29.99597360113117972 ) ) ;
#12625 = DIRECTION ( 'NONE',  ( 0.000000000000000000, 0.000000000000000000, 1.000000000000000000 ) ) ;
#12626 = CARTESIAN_POINT ( 'NONE',  ( -25.21435515916043713, 23.92354251275973809, 25.00736669480994934 ) ) ;
#12627 = CARTESIAN_POINT ( 'NONE',  ( 55.79472521941426777, 6.880567342319705126, 72.42790650415577147 ) ) ;
#12628 = B_SPLINE_CURVE_WITH_KNOTS ( 'NONE', 3,
 ( #18187, #11434, #2951, #494 ),
 .UNSPECIFIED., .F., .F.,
 ( 4, 4 ),
 ( 3.556521592274814591E-16, 0.01077107486149831393 ),
 .UNSPECIFIED. ) ;
#12629 = CARTESIAN_POINT ( 'NONE',  ( -55.25719721206881729, -0.007063345920776780730, 0.008651607285660046359 ) ) ;
#12630 = VERTEX_POINT ( 'NONE', #18118 ) ;
#12631 = B_SPLINE_CURVE_WITH_KNOTS ( 'NONE', 3,
 ( #15229, #24048, #6476, #4308 ),
 .UNSPECIFIED., .F., .F.,
 ( 4, 4 ),
 ( 5.059210310009494697E-16, 0.008383748772659972356 ),
 .UNSPECIFIED. ) ;
#12632 = B_SPLINE_CURVE_WITH_KNOTS ( 'NONE', 3,
 ( #25449, #21524, #23573, #3968, #3834, #12740 ),
 .UNSPECIFIED., .F., .F.,
 ( 4, 2, 4 ),
 ( 1.389302603484999005E-17, 0.0006311571484586087164, 0.001262314296917203555 ),
 .UNSPECIFIED. ) ;
#12633 = CARTESIAN_POINT ( 'NONE',  ( 109.1592201516379674, -0.004867031887010251669, 0.006174480289200302147 ) ) ;
#12634 = EDGE_CURVE ( 'NONE', #23136, #5458, #19520, .T. ) ;
#12635 = CARTESIAN_POINT ( 'NONE',  ( -28.41354790283022069, 21.64275480268748453, -8.345538364877153725 ) ) ;
#12636 = ORIENTED_EDGE ( 'NONE', *, *, #58, .T. ) ;
#12637 = EDGE_CURVE ( 'NONE', #5935, #12494, #16796, .T. ) ;
#12638 = CARTESIAN_POINT ( 'NONE',  ( 1.893872463202018075, 116.8661275359698664, 86.08597552418919463 ) ) ;
#12639 = ORIENTED_EDGE ( 'NONE', *, *, #21359, .T. ) ;
#12640 =( BOUNDED_SURFACE ( )  B_SPLINE_SURFACE ( 3, 1, ( 
 ( #25679, #7988 ),
 ( #10285, #28087 ),
 ( #27672, #12552 ),
 ( #5953, #21477 ) ),
 .UNSPECIFIED., .F., .F., .F. ) 
 B_SPLINE_SURFACE_WITH_KNOTS ( ( 4, 4 ),
 ( 2, 2 ),
 ( 0.000000000000000000, 1.000000000000000000 ),
 ( 0.000000000000000000, 1.000000000000000000 ),
 .UNSPECIFIED. ) 
 GEOMETRIC_REPRESENTATION_ITEM ( )  RATIONAL_B_SPLINE_SURFACE ( (
 ( 1.000000000000000000, 1.000000000000000000),
 ( 0.6386103224230302855, 0.9954351624131538845),
 ( 0.6386103224230302855, 0.9954351624131538845),
 ( 1.000000000000000000, 1.000000000000000000) ) ) 
 REPRESENTATION_ITEM ( '' )  SURFACE ( )  );
#12641 = DIRECTION ( 'NONE',  ( 1.000000000000000000, -0.000000000000000000, -0.000000000000000000 ) ) ;
#12642 = EDGE_CURVE ( 'NONE', #11017, #26529, #19358, .T. ) ;
#12643 = CARTESIAN_POINT ( 'NONE',  ( 2.263178607246654206, -116.7985473178708702, 86.59154415224561774 ) ) ;
#12644 = CARTESIAN_POINT ( 'NONE',  ( 1.834118845439484335, 30.34413640949891189, -141.9019470378984806 ) ) ;
#12645 = CARTESIAN_POINT ( 'NONE',  ( -1.056502255334264895, 0.5104472526226292439, 45.80535052436395915 ) ) ;
#12646 = CARTESIAN_POINT ( 'NONE',  ( 1.833485406944085350, 132.3460930279899515, -59.50871042846091541 ) ) ;
#12647 = DIRECTION ( 'NONE',  ( 0.7563875759206388771, 0.6531865459554678788, 0.03500244528122787441 ) ) ;
#12648 = CARTESIAN_POINT ( 'NONE',  ( 10.93730112725970827, 42.00474393596263667, 145.2260730187401236 ) ) ;
#12649 = B_SPLINE_CURVE_WITH_KNOTS ( 'NONE', 3,
 ( #18867, #7514, #20448, #27639, #7955, #16717 ),
 .UNSPECIFIED., .F., .F.,
 ( 4, 2, 4 ),
 ( 1.964531255190340430E-17, 0.0006311571484586096922, 0.001262314296917200086 ),
 .UNSPECIFIED. ) ;
#12650 = CARTESIAN_POINT ( 'NONE',  ( -2.911734481061421853, 36.84482841982651280, -30.23325065583374638 ) ) ;
#12651 = CARTESIAN_POINT ( 'NONE',  ( 1.831572820252008738, 132.1614873090348681, 59.92262167723481525 ) ) ;
#12652 = CARTESIAN_POINT ( 'NONE',  ( 25.64699802086724389, 34.66526531169786551, -107.4581924007661939 ) ) ;
#12653 = EDGE_LOOP ( 'NONE', ( #19666, #19999, #16854, #1760 ) ) ;
#12654 = ORIENTED_EDGE ( 'NONE', *, *, #3039, .F. ) ;
#12655 = ORIENTED_EDGE ( 'NONE', *, *, #20442, .T. ) ;
#12656 = FACE_OUTER_BOUND ( 'NONE', #9080, .T. ) ;
#12657 = CARTESIAN_POINT ( 'NONE',  ( 30.58324630866342630, -108.8243914523534670, 52.76949945162356670 ) ) ;
#12658 = LINE ( 'NONE', #6618, #4561 ) ;
#12659 = CARTESIAN_POINT ( 'NONE',  ( 32.73300124599738581, 28.19767303745763698, -114.2056417606545153 ) ) ;
#12660 = CARTESIAN_POINT ( 'NONE',  ( -1.464342487929863212, 43.13914623307960738, -16.57334911911526731 ) ) ;
#12661 = DIRECTION ( 'NONE',  ( 0.000000000000000000, 0.000000000000000000, 1.000000000000000000 ) ) ;
#12662 = CARTESIAN_POINT ( 'NONE',  ( 10.93730112725972781, -56.95489579269845137, 140.0398180619108359 ) ) ;
#12663 = ORIENTED_EDGE ( 'NONE', *, *, #26774, .F. ) ;
#12664 = CARTESIAN_POINT ( 'NONE',  ( 32.73300124599732186, 0.000000000000000000, 0.000000000000000000 ) ) ;
#12665 = CARTESIAN_POINT ( 'NONE',  ( -55.24198130335446422, 0.001391250620105636670, -0.009190321388309047670 ) ) ;
#12666 = CARTESIAN_POINT ( 'NONE',  ( 1.833485406944043827, -107.4794113447415924, 97.49333871408656194 ) ) ;
#12667 = B_SPLINE_CURVE_WITH_KNOTS ( 'NONE', 3,
 ( #20490, #13869, #26674, #5233, #11288, #22235 ),
 .UNSPECIFIED., .F., .F.,
 ( 4, 2, 4 ),
 ( 0.000000000000000000, 0.0006311636237756690446, 0.001262327247551338089 ),
 .UNSPECIFIED. ) ;
#12668 = CARTESIAN_POINT ( 'NONE',  ( 26.04756280548354042, 1.110889087302504574, 113.1727782765314032 ) ) ;
#12669 = CARTESIAN_POINT ( 'NONE',  ( 25.65782528836480481, 65.90345832277473903, 91.69136324939124449 ) ) ;
#12670 = ORIENTED_EDGE ( 'NONE', *, *, #13321, .T. ) ;
#12671 = CARTESIAN_POINT ( 'NONE',  ( -2.904412668506657358, 30.27712468694988601, -36.79926976721460363 ) ) ;
#12672 = CARTESIAN_POINT ( 'NONE',  ( 25.98552792386799482, -97.43552975939651617, 57.50018541500390512 ) ) ;
#12673 = VERTEX_POINT ( 'NONE', #998 ) ;
#12674 = VERTEX_POINT ( 'NONE', #20988 ) ;
#12675 = EDGE_CURVE ( 'NONE', #3917, #23740, #17474, .T. ) ;
#12676 = VERTEX_POINT ( 'NONE', #1275 ) ;
#12677 = EDGE_CURVE ( 'NONE', #13373, #7646, #27427, .T. ) ;
#12678 = ADVANCED_FACE ( 'NONE', ( #14215 ), #24907, .T. ) ;
#12679 = CARTESIAN_POINT ( 'NONE',  ( 25.64699802086725100, -110.4930320910559089, -23.24292564406151129 ) ) ;
#12680 = CARTESIAN_POINT ( 'NONE',  ( -20.24419206586952669, 10.37009329716804196, 27.76448493191432476 ) ) ;
#12681 = B_SPLINE_CURVE_WITH_KNOTS ( 'NONE', 3,
 ( #16113, #18130, #9510, #22768, #17975, #20291, #20145 ),
 .UNSPECIFIED., .F., .F.,
 ( 4, 3, 4 ),
 ( 1.201851678989727385E-17, 0.009512539173626329003, 0.02506242213020845599 ),
 .UNSPECIFIED. ) ;
#12682 = DIRECTION ( 'NONE',  ( 0.000000000000000000, 5.223019709708233256E-21, -1.000000000000000000 ) ) ;
#12683 = VERTEX_POINT ( 'NONE', #18560 ) ;
#12684 = CARTESIAN_POINT ( 'NONE',  ( 109.1624594426973260, 0.008380433676406057533, -0.01358749486988133394 ) ) ;
#12685 = DIRECTION ( 'NONE',  ( 0.000000000000000000, 0.000000000000000000, 1.000000000000000000 ) ) ;
#12686 = CARTESIAN_POINT ( 'NONE',  ( -2.911734481061392987, 2.802366807346851285, 47.57875121082947345 ) ) ;
#12687 = CARTESIAN_POINT ( 'NONE',  ( -1.031422197589711987, -1.530725436377782467, -45.78027046666441890 ) ) ;
#12688 =( BOUNDED_SURFACE ( )  B_SPLINE_SURFACE ( 3, 1, ( 
 ( #11528, #598 ),
 ( #24798, #5051 ),
 ( #22637, #20454 ),
 ( #27801, #1454 ) ),
 .UNSPECIFIED., .F., .F., .F. ) 
 B_SPLINE_SURFACE_WITH_KNOTS ( ( 4, 4 ),
 ( 2, 2 ),
 ( 0.000000000000000000, 1.000000000000000000 ),
 ( 0.000000000000000000, 1.000000000000000000 ),
 .UNSPECIFIED. ) 
 GEOMETRIC_REPRESENTATION_ITEM ( )  RATIONAL_B_SPLINE_SURFACE ( (
 ( 1.000000000000000000, 1.000000000000000000),
 ( 0.6386103224230316178, 0.9954351624131538845),
 ( 0.6386103224230316178, 0.9954351624131538845),
 ( 1.000000000000000000, 1.000000000000000000) ) ) 
 REPRESENTATION_ITEM ( '' )  SURFACE ( )  );
#12689 = CARTESIAN_POINT ( 'NONE',  ( 109.1586900883932856, -0.006819617742893414360, -0.002109621908814778967 ) ) ;
#12690 = CARTESIAN_POINT ( 'NONE',  ( -55.24271866751342941, -0.001425019990781919424, 0.009388511352197656881 ) ) ;
#12691 = CARTESIAN_POINT ( 'NONE',  ( 25.64692232868535626, -11.47740546588710941, 112.3263170481597086 ) ) ;
#12692 = CARTESIAN_POINT ( 'NONE',  ( 28.43349137099855284, 102.8504004831932832, 69.71646995966189309 ) ) ;
#12693 = FACE_OUTER_BOUND ( 'NONE', #22208, .T. ) ;
#12694 = CARTESIAN_POINT ( 'NONE',  ( -55.25297051322618813, -0.002853887643043501524, -0.01466904165775538733 ) ) ;
#12695 = VERTEX_POINT ( 'NONE', #16396 ) ;
#12696 = EDGE_CURVE ( 'NONE', #2900, #12695, #10282, .T. ) ;
#12697 = ORIENTED_EDGE ( 'NONE', *, *, #16867, .T. ) ;
#12698 = CARTESIAN_POINT ( 'NONE',  ( -25.21435515916043713, -15.02493970636168896, -31.17620025257581062 ) ) ;
#12700 = ORIENTED_EDGE ( 'NONE', *, *, #12546, .F. ) ;
#12699 = CARTESIAN_POINT ( 'NONE',  ( 16.75465622695661239, -39.51671382433843860, -136.6258322711653079 ) ) ;
#12701 = ORIENTED_EDGE ( 'NONE', *, *, #16903, .T. ) ;
#12702 = EDGE_LOOP ( 'NONE', ( #21422, #13709, #16130, #12298 ) ) ;
#12703 = ORIENTED_EDGE ( 'NONE', *, *, #3654, .F. ) ;
#12704 = ADVANCED_FACE ( 'NONE', ( #9935 ), #16152, .T. ) ;
#12705 = EDGE_CURVE ( 'NONE', #11630, #19484, #10967, .T. ) ;
#12706 = CARTESIAN_POINT ( 'NONE',  ( -55.24271866751342941, 0.001545935011631005204, -0.009369360294295841357 ) ) ;
#12707 = CARTESIAN_POINT ( 'NONE',  ( 26.11404676487257603, -83.38016054979729574, -76.59696442953277540 ) ) ;
#12708 = CARTESIAN_POINT ( 'NONE',  ( 1.834118845439484335, -58.85894970554831218, -132.6369225636079818 ) ) ;
#12709 = DIRECTION ( 'NONE',  ( -0.5914120900931443270, -0.8063295922669344584, 0.008020494142993420464 ) ) ;
#12710 = CARTESIAN_POINT ( 'NONE',  ( 26.11404676487257603, -10.71016160607490875, -112.7148551500681606 ) ) ;
#12711 = CARTESIAN_POINT ( 'NONE',  ( -22.34422965417122242, 27.39717383755282043, -26.20925041532862920 ) ) ;
#12712 = CARTESIAN_POINT ( 'NONE',  ( 1.834118845439484335, -72.70910183320481224, -125.5799175751977259 ) ) ;
#12713 = CARTESIAN_POINT ( 'NONE',  ( 109.1624594426973260, 0.01033277910988597038, 0.01216903288310111977 ) ) ;
#12714 =( LENGTH_UNIT ( ) NAMED_UNIT ( * ) SI_UNIT ( .MILLI., .METRE. ) );
#12715 =( BOUNDED_SURFACE ( )  B_SPLINE_SURFACE ( 3, 1, ( 
 ( #12022, #9573 ),
 ( #9872, #18640 ),
 ( #5695, #12432 ),
 ( #24996, #22836 ) ),
 .UNSPECIFIED., .F., .F., .F. ) 
 B_SPLINE_SURFACE_WITH_KNOTS ( ( 4, 4 ),
 ( 2, 2 ),
 ( 0.000000000000000000, 1.000000000000000000 ),
 ( 0.000000000000000000, 1.000000000000000000 ),
 .UNSPECIFIED. ) 
 GEOMETRIC_REPRESENTATION_ITEM ( )  RATIONAL_B_SPLINE_SURFACE ( (
 ( 1.000000000000000000, 1.000000000000000000),
 ( 0.6386103224230302855, 0.9954351624131538845),
 ( 0.6386103224230302855, 0.9954351624131538845),
 ( 1.000000000000000000, 1.000000000000000000) ) ) 
 REPRESENTATION_ITEM ( '' )  SURFACE ( )  );
#12716 = EDGE_LOOP ( 'NONE', ( #28431, #2791, #3189, #7869 ) ) ;
#12717 = EDGE_LOOP ( 'NONE', ( #227, #16668, #3964, #14086 ) ) ;
#12719 = CARTESIAN_POINT ( 'NONE',  ( -1.031422197589716205, -15.60268798220608844, 43.06660437151324317 ) ) ;
#12718 = CARTESIAN_POINT ( 'NONE',  ( 26.11404676487257603, -10.71016160607644174, 112.7148551500680185 ) ) ;
#12720 = CARTESIAN_POINT ( 'NONE',  ( -1.031422197589716205, 44.01264471863849082, -12.69107518035517046 ) ) ;
#12721 = DIRECTION ( 'NONE',  ( 0.000000000000000000, -1.000000000000000000, 0.000000000000000000 ) ) ;
#12722 = CARTESIAN_POINT ( 'NONE',  ( 109.1592201516379674, 0.006957642258146918765, -0.003661068210037320397 ) ) ;
#12723 = ORIENTED_EDGE ( 'NONE', *, *, #10921, .T. ) ;
#12724 = CARTESIAN_POINT ( 'NONE',  ( -1.583189561560253589, -2.490696082060195327, -46.33203782964460515 ) ) ;
#12725 = EDGE_CURVE ( 'NONE', #21979, #14003, #15747, .T. ) ;
#12726 = CARTESIAN_POINT ( 'NONE',  ( -1.619063947482197729, 44.80407745103800465, 11.94059994246113021 ) ) ;
#12727 = CARTESIAN_POINT ( 'NONE',  ( -28.13707043255157103, 22.88591869784691113, -0.7675454997507807908 ) ) ;
#12728 = EDGE_LOOP ( 'NONE', ( #15157, #21173, #4949, #27880 ) ) ;
#12729 = ORIENTED_EDGE ( 'NONE', *, *, #22098, .T. ) ;
#12730 = EDGE_CURVE ( 'NONE', #987, #15703, #26060, .T. ) ;
#12731 = B_SPLINE_CURVE_WITH_KNOTS ( 'NONE', 3,
 ( #5693, #23262, #16187, #3513 ),
 .UNSPECIFIED., .F., .F.,
 ( 4, 4 ),
 ( 1.877672896018868361E-16, 0.001982023823822947652 ),
 .UNSPECIFIED. ) ;
#12732 = DIRECTION ( 'NONE',  ( 1.000000000000000000, -6.938893903907226837E-18, 1.734723475976806709E-18 ) ) ;
#12733 = ORIENTED_EDGE ( 'NONE', *, *, #19395, .T. ) ;
#12734 = B_SPLINE_CURVE_WITH_KNOTS ( 'NONE', 3,
 ( #19074, #14741, #3518, #25703, #18782, #5841, #5982, #20935, #3661, #27849 ),
 .UNSPECIFIED., .F., .F.,
 ( 4, 3, 3, 4 ),
 ( 6.938893903907228378E-18, 0.0002669560319015836392, 0.0005492286108966428632, 0.0008315040496093566071 ),
 .UNSPECIFIED. ) ;
#12735 = VERTEX_POINT ( 'NONE', #6554 ) ;
#12736 = EDGE_CURVE ( 'NONE', #12813, #6178, #8567, .T. ) ;
#12737 = CARTESIAN_POINT ( 'NONE',  ( 1.833485406944043827, -14.63699153649261575, -144.3694338680886347 ) ) ;
#12738 = EDGE_CURVE ( 'NONE', #9533, #28300, #28269, .T. ) ;
#12739 = VERTEX_POINT ( 'NONE', #3576 ) ;
#12740 = CARTESIAN_POINT ( 'NONE',  ( 2.433796855181233454, -74.00833731765476386, -125.2830755159761935 ) ) ;
#12741 = CARTESIAN_POINT ( 'NONE',  ( 119.2224693531408803, -90.00000000000005684, 39.99999999999997158 ) ) ;
#12742 = CARTESIAN_POINT ( 'NONE',  ( -55.24271866751342941, 0.001425019990782615698, -0.009388511352197861579 ) ) ;
#12743 = CARTESIAN_POINT ( 'NONE',  ( 9.884929003653626367, -119.2676479132379512, 91.84919534721903744 ) ) ;
#12744 = CARTESIAN_POINT ( 'NONE',  ( 6.224689322667630975, 148.0369967195762797, 2.565137105444272425 ) ) ;
#12745 = CARTESIAN_POINT ( 'NONE',  ( 109.1587776205901861, 0.007297420966932447080, 0.0006832286435017099514 ) ) ;
#12746 = B_SPLINE_CURVE_WITH_KNOTS ( 'NONE', 3,
 ( #13054, #25746, #17092, #28434 ),
 .UNSPECIFIED., .F., .F.,
 ( 4, 4 ),
 ( 0.000000000000000000, 0.01077107196513890641 ),
 .UNSPECIFIED. ) ;
#12747 = CARTESIAN_POINT ( 'NONE',  ( 26.11404676487259024, -103.8885755249566643, -45.01677474591514283 ) ) ;
#12748 = CARTESIAN_POINT ( 'NONE',  ( 1.832998868059858122, -30.69214149074111475, 141.8272129421607701 ) ) ;
#12749 = CARTESIAN_POINT ( 'NONE',  ( 25.64681081121880624, -102.9795863647025556, -46.30456157731431688 ) ) ;
#12750 = EDGE_LOOP ( 'NONE', ( #20006, #4137, #25931, #7134 ) ) ;
#12751 = ORIENTED_EDGE ( 'NONE', *, *, #20267, .F. ) ;
#12752 = CARTESIAN_POINT ( 'NONE',  ( -55.24340739397742084, -0.005344433640972736689, -0.008612749836246649457 ) ) ;
#12753 = CARTESIAN_POINT ( 'NONE',  ( 24.22246935314087324, -90.00000000000005684, -40.00000000000002842 ) ) ;
#12754 = CARTESIAN_POINT ( 'NONE',  ( 2.063896406836609909, 144.3268707900449783, -16.52087515463630751 ) ) ;
#12755 = CARTESIAN_POINT ( 'NONE',  ( 19.66333377628705747, 64.94841092372186608, 121.4767361208137828 ) ) ;
#12756 = DIRECTION ( 'NONE',  ( 1.000000000000000000, -6.938893903907226837E-18, 1.734723475976806709E-18 ) ) ;
#12757 = CARTESIAN_POINT ( 'NONE',  ( -23.77929240705206837, -15.74261278740695502, -32.66578242509739027 ) ) ;
#12758 = CARTESIAN_POINT ( 'NONE',  ( 1.832998868059890096, 125.9352106559983895, 72.09222286251126377 ) ) ;
#12759 = ORIENTED_EDGE ( 'NONE', *, *, #7010, .T. ) ;
#12760 = CARTESIAN_POINT ( 'NONE',  ( 26.11404676487257603, 12.95861723607603544, -112.4785329405480780 ) ) ;
#12761 = CARTESIAN_POINT ( 'NONE',  ( -55.24300891470648622, 0.003362556190415182372, -0.009225237711098200136 ) ) ;
#12762 = FACE_OUTER_BOUND ( 'NONE', #20509, .T. ) ;
#12763 = CARTESIAN_POINT ( 'NONE',  ( 25.64660436782548203, -55.95243482911462962, 98.07256794792309051 ) ) ;
#12764 = ADVANCED_FACE ( 'NONE', ( #15306 ), #19737, .F. ) ;
#12765 = ORIENTED_EDGE ( 'NONE', *, *, #18024, .T. ) ;
#12766 = CARTESIAN_POINT ( 'NONE',  ( -55.24728320129491266, 0.003868537197317429340, 0.01402509393918536899 ) ) ;
#12767 =( BOUNDED_SURFACE ( )  B_SPLINE_SURFACE ( 3, 1, ( 
 ( #18572, #720 ),
 ( #27189, #24644 ),
 ( #24490, #16267 ),
 ( #22620, #4897 ) ),
 .UNSPECIFIED., .F., .F., .F. ) 
 B_SPLINE_SURFACE_WITH_KNOTS ( ( 4, 4 ),
 ( 2, 2 ),
 ( 0.000000000000000000, 1.000000000000000000 ),
 ( 0.000000000000000000, 1.000000000000000000 ),
 .UNSPECIFIED. ) 
 GEOMETRIC_REPRESENTATION_ITEM ( )  RATIONAL_B_SPLINE_SURFACE ( (
 ( 1.000000000000000000, 1.000000000000000000),
 ( 0.9934239774497838349, 0.8357310067453913582),
 ( 0.9934239774497838349, 0.8357310067453913582),
 ( 1.000000000000000000, 1.000000000000000000) ) ) 
 REPRESENTATION_ITEM ( '' )  SURFACE ( )  );
#12768 = EDGE_CURVE ( 'NONE', #15878, #238, #15073, .T. ) ;
#12769 = CARTESIAN_POINT ( 'NONE',  ( 2.263178607246644880, -137.8402782326814702, 46.26071628252405077 ) ) ;
#12770 = B_SPLINE_CURVE_WITH_KNOTS ( 'NONE', 3,
 ( #27545, #1214, #7035, #23116, #15793, #12014, #7718, #18922 ),
 .UNSPECIFIED., .F., .F.,
 ( 4, 2, 2, 4 ),
 ( 0.000000000000000000, 0.0002429592666046702821, 0.0004859185332093405641, 0.0009718370664186944639 ),
 .UNSPECIFIED. ) ;
#12771 = ADVANCED_FACE ( 'NONE', ( #17471 ), #7078, .F. ) ;
#12772 = ORIENTED_EDGE ( 'NONE', *, *, #11938, .F. ) ;
#12773 = CARTESIAN_POINT ( 'NONE',  ( -1.259920593601986383, 38.49623866863347388, -25.19630221849063290 ) ) ;
#12774 = CARTESIAN_POINT ( 'NONE',  ( 10.93730112725990189, -140.0398180619108075, -56.95489579269887059 ) ) ;
#12775 = CARTESIAN_POINT ( 'NONE',  ( 25.64692872815575342, 97.62272225320948849, 56.73392579406745284 ) ) ;
#12776 = DIRECTION ( 'NONE',  ( 0.000000000000000000, 0.000000000000000000, 1.000000000000000000 ) ) ;
#12777 = CARTESIAN_POINT ( 'NONE',  ( -25.21435515916043713, -23.92354251275918031, 25.00736669481048224 ) ) ;
#12778 = CARTESIAN_POINT ( 'NONE',  ( -23.77929240705205771, -26.20227034809537514, 25.06639637888449457 ) ) ;
#12779 = CARTESIAN_POINT ( 'NONE',  ( 30.59141879584290535, -109.6600586137411284, -38.47120193631578644 ) ) ;
#12780 = CARTESIAN_POINT ( 'NONE',  ( -2.911734481061404534, -2.802366807346520439, -47.57875121082949477 ) ) ;
#12781 = CARTESIAN_POINT ( 'NONE',  ( -1.583189561560253589, 43.29471907393742214, -16.68617981233717629 ) ) ;
#12782 = AXIS2_PLACEMENT_3D ( 'NONE', #9179, #17940, #24608 ) ;
#12783 = CARTESIAN_POINT ( 'NONE',  ( 26.04756280548354397, 110.9306483680202859, 22.44333019059037326 ) ) ;
#12784 = CONICAL_SURFACE ( 'NONE', #16469, 117.6351876552689504, 0.9945805576725580410 ) ;
#12785 = CARTESIAN_POINT ( 'NONE',  ( 32.73300124599740002, 72.21147546950675178, -92.86301839379947864 ) ) ;
#12786 = FACE_OUTER_BOUND ( 'NONE', #16238, .T. ) ;
#12787 = CARTESIAN_POINT ( 'NONE',  ( 2.433796855181233454, -57.85512797797981932, 133.5135467655516095 ) ) ;
#12788 = ORIENTED_EDGE ( 'NONE', *, *, #23369, .F. ) ;
#12789 = ORIENTED_EDGE ( 'NONE', *, *, #1434, .T. ) ;
#12790 = EDGE_LOOP ( 'NONE', ( #14254, #18025, #26479, #13775 ) ) ;
#12791 = CARTESIAN_POINT ( 'NONE',  ( 109.1586900883932856, -0.0006456433529069550677, 0.007109207791180748720 ) ) ;
#12792 = CARTESIAN_POINT ( 'NONE',  ( -20.57838717382308147, -28.96176188950213870, 7.715628353033985753 ) ) ;
#12793 = FACE_OUTER_BOUND ( 'NONE', #12459, .T. ) ;
#12794 = CARTESIAN_POINT ( 'NONE',  ( 1.833485406944043827, -97.49333871408619245, -107.4794113447419477 ) ) ;
#12795 = CARTESIAN_POINT ( 'NONE',  ( 26.11404676487259024, -92.25884714080363835, -65.63269960453335727 ) ) ;
#12796 = CARTESIAN_POINT ( 'NONE',  ( 109.1592201516379674, -0.004368284148525305825, 0.006536841731961986514 ) ) ;
#12797 = CARTESIAN_POINT ( 'NONE',  ( 2.063896406836609909, -1.344106060019351734, -145.2631347824382999 ) ) ;
#12798 = ORIENTED_EDGE ( 'NONE', *, *, #28203, .F. ) ;
#12799 = DIRECTION ( 'NONE',  ( -1.000000000000000000, -0.000000000000000000, -0.000000000000000000 ) ) ;
#12800 = CARTESIAN_POINT ( 'NONE',  ( -1.056502255334265339, -14.64009593116072949, 43.40574022158788381 ) ) ;
#12801 = CARTESIAN_POINT ( 'NONE',  ( -1.049819825607600121, -37.34982882986862052, -26.50610175068254293 ) ) ;
#12802 = B_SPLINE_CURVE_WITH_KNOTS ( 'NONE', 3,
 ( #26803, #17592, #7113, #4492, #2325, #4931, #13700 ),
 .UNSPECIFIED., .F., .F.,
 ( 4, 3, 4 ),
 ( 0.000000000000000000, 0.006568092053401789268, 0.02506242213020845946 ),
 .UNSPECIFIED. ) ;
#12803 = EDGE_CURVE ( 'NONE', #21106, #27239, #24706, .T. ) ;
#12804 = DIRECTION ( 'NONE',  ( 0.5946245182733607137, -0.6977579871484591578, 0.3994439555666155495 ) ) ;
#12805 =( BOUNDED_SURFACE ( )  B_SPLINE_SURFACE ( 3, 1, ( 
 ( #6208, #23774 ),
 ( #19148, #1716 ),
 ( #17534, #26318 ),
 ( #26180, #19559 ) ),
 .UNSPECIFIED., .F., .F., .F. ) 
 B_SPLINE_SURFACE_WITH_KNOTS ( ( 4, 4 ),
 ( 2, 2 ),
 ( 0.000000000000000000, 1.000000000000000000 ),
 ( 0.000000000000000000, 1.000000000000000000 ),
 .UNSPECIFIED. ) 
 GEOMETRIC_REPRESENTATION_ITEM ( )  RATIONAL_B_SPLINE_SURFACE ( (
 ( 1.000000000000000000, 1.000000000000000000),
 ( 0.9956975270656954757, 0.8568959468854893125),
 ( 0.9956975270656954757, 0.8568959468854893125),
 ( 1.000000000000000000, 1.000000000000000000) ) ) 
 REPRESENTATION_ITEM ( '' )  SURFACE ( )  );
#12806 = EDGE_LOOP ( 'NONE', ( #8275, #25209, #6807, #18411, #12862, #13094, #7563, #11284, #27180, #23202, #24687, #26617, #16174, #11204, #22557, #6893, #6143, #19263, #1870, #5964, #25707, #3963, #2776, #2170, #23392, #5406, #10402, #16769, #27006, #8819, #8770, #6784, #1273, #5453, #22420, #13545, #7761, #18181, #21245, #14992, #8500, #22860, #22935, #2140, #25550, #17098, #27688, #10347, #27305, #24332, #173, #12075, #25175, #19769, #8947, #23799, #9998, #6957, #18403, #22082, #19843, #14143, #11952, #2202, #4465, #18648, #24832, #8228, #14026, #26255, #9381, #24609, #20522, #8354, #13495, #10109, #21407, #425, #3102, #25472, #2975, #2072, #24999, #6281, #7171, #5999, #1822, #3307, #10428, #1682, #16803, #5415, #15994, #21399, #6804, #20278, #1379, #27964, #2223, #6021, #22840, #24281, #22317, #20063, #2380, #16437, #8403, #4172, #11878, #12954, #1251, #6129, #20817, #6556, #8745, #8320, #6223, #2613, #8145, #26711, #20741, #17834, #24911, #10114, #13512, #1922, #3270, #16733, #4755, #19706, #10653, #13584, #7801, #27580, #3640, #13825, #8688, #10074, #16055, #2940, #27508, #14863, #1848, #408, #5265, #17667, #14011, #3530, #14140, #1882, #15704, #8995, #21598, #4498, #9939, #2850, #2311, #10996, #4977, #9448, #11723, #22310, #7136, #2014, #9477, #4607, #27368, #23828, #15896, #19930, #14607, #12852, #3679, #13919, #17659, #5229, #556, #10956, #17838, #23385, #16372, #3502, #16542, #3124 ) ) ;
#12807 = CARTESIAN_POINT ( 'NONE',  ( 25.64681081121880624, -45.54494737132293380, 103.3177883989777825 ) ) ;
#12808 = EDGE_CURVE ( 'NONE', #4550, #27179, #7212, .T. ) ;
#12809 = CARTESIAN_POINT ( 'NONE',  ( -1.050230347699842692, 5.964912479342754695E-15, -45.79907861674080749 ) ) ;
#12810 = EDGE_LOOP ( 'NONE', ( #22760, #14889, #76, #15724 ) ) ;
#12811 = ADVANCED_FACE ( 'NONE', ( #22083 ), #21600, .F. ) ;
#12812 = AXIS2_PLACEMENT_3D ( 'NONE', #13420, #6535, #20044 ) ;
#12813 = VERTEX_POINT ( 'NONE', #15027 ) ;
#12814 = CIRCLE ( 'NONE', #20141, 117.6351876552689504 ) ;
#12815 = ORIENTED_EDGE ( 'NONE', *, *, #20807, .T. ) ;
#12816 = CARTESIAN_POINT ( 'NONE',  ( 2.430230287190581429, 98.44218333480918659, -107.1617224697454276 ) ) ;
#12817 = CARTESIAN_POINT ( 'NONE',  ( 30.59138290137910943, 66.10404757334188730, -95.58039132682482375 ) ) ;
#12818 = DIRECTION ( 'NONE',  ( 0.000000000000000000, 0.000000000000000000, 1.000000000000000000 ) ) ;
#12819 = CARTESIAN_POINT ( 'NONE',  ( 10.93730112726003156, 97.44200844886434254, -115.5857507957695276 ) ) ;
#12820 = VERTEX_POINT ( 'NONE', #23846 ) ;
#12821 = CARTESIAN_POINT ( 'NONE',  ( 1.833838850855476377, 59.10274688032031776, -132.5281727421680387 ) ) ;
#12822 = CARTESIAN_POINT ( 'NONE',  ( 1.893872463202080692, -0.9528309182407600497, 145.1467500857187360 ) ) ;
#12823 = EDGE_CURVE ( 'NONE', #5123, #19834, #4101, .T. ) ;
#12824 = CARTESIAN_POINT ( 'NONE',  ( 10.93730112725932635, 0.000000000000000000, 0.000000000000000000 ) ) ;
#12825 = DIRECTION ( 'NONE',  ( 0.7637818620346801257, 0.6201872550346656521, -0.1788995134688848854 ) ) ;
#12826 = CARTESIAN_POINT ( 'NONE',  ( 1.833838848569419477, -141.9757689770219997, -29.99593366454900334 ) ) ;
#12827 = ADVANCED_FACE ( 'NONE', ( #23424 ), #12917, .T. ) ;
#12828 = FACE_OUTER_BOUND ( 'NONE', #739, .T. ) ;
#12829 = CARTESIAN_POINT ( 'NONE',  ( 109.1624594426973260, -0.006914244825461735369, 0.01438905500501224191 ) ) ;
#12830 = CARTESIAN_POINT ( 'NONE',  ( -24.53239521893647179, -16.68574937150994231, -29.54733954334103174 ) ) ;
#12831 = ORIENTED_EDGE ( 'NONE', *, *, #25225, .F. ) ;
#12832 = ORIENTED_EDGE ( 'NONE', *, *, #9862, .F. ) ;
#12833 = CARTESIAN_POINT ( 'NONE',  ( 26.04756280548355818, -24.61655718144259808, -110.4687147111162631 ) ) ;
#12834 = CARTESIAN_POINT ( 'NONE',  ( -1.050231094221210970, 45.79908322896420003, -0.2545420581350661404 ) ) ;
#12835 = ORIENTED_EDGE ( 'NONE', *, *, #15318, .T. ) ;
#12836 = ORIENTED_EDGE ( 'NONE', *, *, #28375, .T. ) ;
#12837 = ORIENTED_EDGE ( 'NONE', *, *, #4323, .F. ) ;
#12838 = CARTESIAN_POINT ( 'NONE',  ( 1.833485406944043827, 137.8414413349085521, 45.34878176254281357 ) ) ;
#12839 = CARTESIAN_POINT ( 'NONE',  ( 2.433796855181219243, -144.5536872373193376, 16.65276281464516828 ) ) ;
#12840 = CARTESIAN_POINT ( 'NONE',  ( -8.786685647604890903, -37.00619870957961410, -38.68584556812286479 ) ) ;
#12841 =( BOUNDED_SURFACE ( )  B_SPLINE_SURFACE ( 3, 1, ( 
 ( #10797, #13082 ),
 ( #15226, #8494 ),
 ( #24178, #21581 ),
 ( #1852, #10656 ) ),
 .UNSPECIFIED., .F., .F., .F. ) 
 B_SPLINE_SURFACE_WITH_KNOTS ( ( 4, 4 ),
 ( 2, 2 ),
 ( 0.000000000000000000, 1.000000000000000000 ),
 ( 0.000000000000000000, 1.000000000000000000 ),
 .UNSPECIFIED. ) 
 GEOMETRIC_REPRESENTATION_ITEM ( )  RATIONAL_B_SPLINE_SURFACE ( (
 ( 1.000000000000000000, 1.000000000000000000),
 ( 0.9956975270656955868, 0.8568959468854907557),
 ( 0.9956975270656955868, 0.8568959468854907557),
 ( 1.000000000000000000, 1.000000000000000000) ) ) 
 REPRESENTATION_ITEM ( '' )  SURFACE ( )  );
#12842 = CARTESIAN_POINT ( 'NONE',  ( 109.1624594426973260, -0.01591840958352309932, 0.001206615835671121352 ) ) ;
#12843 = EDGE_CURVE ( 'NONE', #21851, #8890, #23328, .T. ) ;
#12844 = LINE ( 'NONE', #28243, #6569 ) ;
#12845 = CARTESIAN_POINT ( 'NONE',  ( 32.73300124599735739, 20.69176323058628597, 115.8010721414084543 ) ) ;
#12846 = CARTESIAN_POINT ( 'NONE',  ( -7.733045908741337016, 47.75066202881826882, 21.80378472388440514 ) ) ;
#12847 = EDGE_CURVE ( 'NONE', #8562, #13021, #26754, .T. ) ;
#12848 = CARTESIAN_POINT ( 'NONE',  ( 109.1586059443104944, 0.003127959656220996847, 0.006344953511159737332 ) ) ;
#12849 = CARTESIAN_POINT ( 'NONE',  ( -1.049817751779889008, 26.50542916749622080, 37.35030165458145746 ) ) ;
#12850 = EDGE_CURVE ( 'NONE', #26713, #27831, #12049, .T. ) ;
#12851 = VERTEX_POINT ( 'NONE', #21246 ) ;
#12852 = ORIENTED_EDGE ( 'NONE', *, *, #11120, .T. ) ;
#12854 = CARTESIAN_POINT ( 'NONE',  ( 28.37644542392833813, 34.54617949428102008, 119.4444529625692581 ) ) ;
#12853 = CARTESIAN_POINT ( 'NONE',  ( 2.263178113027065397, 133.3897502891102533, -57.85473702513737493 ) ) ;
#12855 = AXIS2_PLACEMENT_3D ( 'NONE', #17237, #27902, #8337 ) ;
#12856 = DIRECTION ( 'NONE',  ( 0.5946245182733607137, 0.7332888028688904214, 0.3297108033645291814 ) ) ;
#12857 = CARTESIAN_POINT ( 'NONE',  ( 2.433796855181233454, 96.28145139437833677, -109.1007109081216129 ) ) ;
#12858 = EDGE_LOOP ( 'NONE', ( #22351, #11947, #17885, #17681 ) ) ;
#12859 = CARTESIAN_POINT ( 'NONE',  ( -1.583189561560252701, 29.24830400313166123, -36.01941156322796900 ) ) ;
#12860 = DIRECTION ( 'NONE',  ( -1.000000000000000000, -0.000000000000000000, -0.000000000000000000 ) ) ;
#12861 = CARTESIAN_POINT ( 'NONE',  ( -1.048996300304493312, -27.53442103413720332, -36.59642367107734628 ) ) ;
#12862 = ORIENTED_EDGE ( 'NONE', *, *, #14534, .T. ) ;
#12863 = ORIENTED_EDGE ( 'NONE', *, *, #6493, .F. ) ;
#12864 = B_SPLINE_CURVE_WITH_KNOTS ( 'NONE', 3,
 ( #5727, #25155, #16508, #5573, #14626, #12053 ),
 .UNSPECIFIED., .F., .F.,
 ( 4, 2, 4 ),
 ( 1.964531255190340430E-17, 0.0006311571484586177153, 0.001262314296917215915 ),
 .UNSPECIFIED. ) ;
#12865 = CARTESIAN_POINT ( 'NONE',  ( -1.045287976400362417, -15.59869763335038506, 43.05558670614261985 ) ) ;
#12866 = CARTESIAN_POINT ( 'NONE',  ( -28.41354790283022069, -12.60397206714846341, -19.47297445639544833 ) ) ;
#12867 = ORIENTED_EDGE ( 'NONE', *, *, #14293, .F. ) ;
#12868 = CARTESIAN_POINT ( 'NONE',  ( -8.786685647604890903, -9.545808661480235102, 52.67761315067295413 ) ) ;
#12869 = ORIENTED_EDGE ( 'NONE', *, *, #13312, .F. ) ;
#12870 = AXIS2_PLACEMENT_3D ( 'NONE', #2744, #24927, #5189 ) ;
#12871 = CARTESIAN_POINT ( 'NONE',  ( -1.323830074806771284, 2.318057800980712457, -46.01435746200690602 ) ) ;
#12872 = CIRCLE ( 'NONE', #1853, 34.60786435723138510 ) ;
#12873 = CARTESIAN_POINT ( 'NONE',  ( -23.79223135445719350, -13.25822371132274924, 30.42557260166825017 ) ) ;
#12874 = CARTESIAN_POINT ( 'NONE',  ( -20.24399999263415140, 27.76448601145554562, 10.36954246768216059 ) ) ;
#12876 = AXIS2_PLACEMENT_3D ( 'NONE', #3340, #21032, #1186 ) ;
#12875 =( BOUNDED_SURFACE ( )  B_SPLINE_SURFACE ( 3, 1, ( 
 ( #3919, #10126 ),
 ( #23511, #10280 ),
 ( #25942, #27947 ),
 ( #23800, #6359 ) ),
 .UNSPECIFIED., .F., .F., .F. ) 
 B_SPLINE_SURFACE_WITH_KNOTS ( ( 4, 4 ),
 ( 2, 2 ),
 ( 0.000000000000000000, 1.000000000000000000 ),
 ( 0.000000000000000000, 1.000000000000000000 ),
 .UNSPECIFIED. ) 
 GEOMETRIC_REPRESENTATION_ITEM ( )  RATIONAL_B_SPLINE_SURFACE ( (
 ( 1.000000000000000000, 1.000000000000000000),
 ( 0.6386103224230316178, 0.9954351624131538845),
 ( 0.6386103224230316178, 0.9954351624131538845),
 ( 1.000000000000000000, 1.000000000000000000) ) ) 
 REPRESENTATION_ITEM ( '' )  SURFACE ( )  );
#12877 = ADVANCED_FACE ( 'NONE', ( #12186 ), #15702, .F. ) ;
#12878 = DIRECTION ( 'NONE',  ( -1.000000000000000000, -0.000000000000000000, -0.000000000000000000 ) ) ;
#12879 = CARTESIAN_POINT ( 'NONE',  ( 25.87036335909425233, -107.2165474610297196, 35.87755773825682581 ) ) ;
#12880 = CARTESIAN_POINT ( 'NONE',  ( -7.078251931573406708, 5.101176922831390570, 51.82710018979469879 ) ) ;
#12881 = LINE ( 'NONE', #17210, #930 ) ;
#12882 = EDGE_CURVE ( 'NONE', #18351, #10615, #28425, .T. ) ;
#12883 = ORIENTED_EDGE ( 'NONE', *, *, #21632, .T. ) ;
#12884 = CARTESIAN_POINT ( 'NONE',  ( 26.11404676487257603, 102.9690087468801352, 47.08215554553553517 ) ) ;
#12885 = CARTESIAN_POINT ( 'NONE',  ( -1.155031165708874097, 45.85732438018715129, -2.068616213631106593 ) ) ;
#12886 = FACE_OUTER_BOUND ( 'NONE', #12858, .T. ) ;
#12887 = EDGE_CURVE ( 'NONE', #27587, #13373, #12336, .T. ) ;
#12888 = VERTEX_POINT ( 'NONE', #6006 ) ;
#12889 = ORIENTED_EDGE ( 'NONE', *, *, #18734, .T. ) ;
#12890 = CARTESIAN_POINT ( 'NONE',  ( 10.93730112725936721, 145.2260730187397542, 42.00474393596321931 ) ) ;
#12891 = CARTESIAN_POINT ( 'NONE',  ( -1.155001620486246994, 25.28075036143276932, 38.31519699443472859 ) ) ;
#12893 = DIRECTION ( 'NONE',  ( 0.5946245182733607137, 0.1700465163848252637, -0.7858154137795714256 ) ) ;
#12892 = CARTESIAN_POINT ( 'NONE',  ( 55.49584447822657296, 58.85239198729187393, 42.42793568432977480 ) ) ;
#12894 = CARTESIAN_POINT ( 'NONE',  ( -10.86508079875782329, 24.22249093393363850, 45.04061326950845512 ) ) ;
#12895 = CARTESIAN_POINT ( 'NONE',  ( 2.430230287190592531, 74.01081053031100510, 125.2872625092164895 ) ) ;
#12896 = CARTESIAN_POINT ( 'NONE',  ( -28.41354790283022069, 12.60397206714832663, -19.47297445639553715 ) ) ;
#12897 = ADVANCED_FACE ( 'NONE', ( #14764 ), #12939, .F. ) ;
#12898 = ORIENTED_EDGE ( 'NONE', *, *, #19204, .F. ) ;
#12899 = CARTESIAN_POINT ( 'NONE',  ( -55.24340739397742794, -0.006539691034608149933, -0.007744344507854676943 ) ) ;
#12900 = CONICAL_SURFACE ( 'NONE', #7412, 53.53553390275978785, 0.7853981625000051592 ) ;
#12901 = CARTESIAN_POINT ( 'NONE',  ( -1.045287976400362417, 25.66401692420069125, 37.92705037016716574 ) ) ;
#12902 = DIRECTION ( 'NONE',  ( 0.000000000000000000, 0.000000000000000000, 1.000000000000000000 ) ) ;
#12903 = CARTESIAN_POINT ( 'NONE',  ( -7.711401346138401891, 35.51061203065580685, 38.61705198405327621 ) ) ;
#12904=STYLED_ITEM('',(#28500),#7750);
#12905 = ORIENTED_EDGE ( 'NONE', *, *, #23940, .T. ) ;
#12906 = CARTESIAN_POINT ( 'NONE',  ( 109.1586059443104944, 0.006856640434643072185, -0.001740416220259429674 ) ) ;
#12907 = VECTOR ( 'NONE', #13914, 999.9999999999998863 ) ;
#12908 = ORIENTED_EDGE ( 'NONE', *, *, #24732, .T. ) ;
#12909 = CARTESIAN_POINT ( 'NONE',  ( 1.894214914920961723, -29.24491455759036995, 142.1734439042097051 ) ) ;
#12910 = B_SPLINE_CURVE_WITH_KNOTS ( 'NONE', 3,
 ( #15767, #26698, #18202, #26978, #13313, #7287 ),
 .UNSPECIFIED., .F., .F.,
 ( 4, 2, 4 ),
 ( 9.875766617722657020E-18, 0.0006311571484586050301, 0.001262314296917200953 ),
 .UNSPECIFIED. ) ;
#12911 = ORIENTED_EDGE ( 'NONE', *, *, #3535, .F. ) ;
#12912 = CARTESIAN_POINT ( 'NONE',  ( 25.69398547355839924, 65.78402800526286853, -91.80679989327076385 ) ) ;
#12913 = DIRECTION ( 'NONE',  ( 0.5914120900931444380, 0.5938529060132621273, 0.5455001977188111972 ) ) ;
#12914 = CARTESIAN_POINT ( 'NONE',  ( 25.64700659047695552, 97.67001118499099732, 56.65258046470288633 ) ) ;
#12915 = CARTESIAN_POINT ( 'NONE',  ( 109.1586900883932856, -0.0001010081143884653671, 0.007137750914552287197 ) ) ;
#12916 = DIRECTION ( 'NONE',  ( 0.000000000000000000, 5.223019709707975211E-21, -1.000000000000000000 ) ) ;
#12917 = CONICAL_SURFACE ( 'NONE', #13850, 117.6351876552689504, 0.9945805576725580410 ) ;
#12918 = B_SPLINE_CURVE_WITH_KNOTS ( 'NONE', 3,
 ( #11431, #15895, #640, #24402 ),
 .UNSPECIFIED., .F., .F.,
 ( 4, 4 ),
 ( 0.000000000000000000, 0.008383560773332715543 ),
 .UNSPECIFIED. ) ;
#12919 = CARTESIAN_POINT ( 'NONE',  ( -1.619063947482194177, -46.30105812165547974, 2.489035965910640247 ) ) ;
#12920 = CARTESIAN_POINT ( 'NONE',  ( -1.031422197589711764, -43.06660437151319343, -15.60268798220621100 ) ) ;
#12921 = DIRECTION ( 'NONE',  ( 1.000000000000000000, -6.938893903907226837E-18, 1.734723475976806709E-18 ) ) ;
#12922 = CARTESIAN_POINT ( 'NONE',  ( -55.25719721206881729, 0.002847566758683125598, -0.01079965405819887508 ) ) ;
#12923 = EDGE_CURVE ( 'NONE', #20744, #18597, #6525, .T. ) ;
#12924 = VECTOR ( 'NONE', #19077, 1000.000000000000000 ) ;
#12925 = B_SPLINE_CURVE_WITH_KNOTS ( 'NONE', 3,
 ( #1812, #19241, #10351, #21266, #10611, #27885 ),
 .UNSPECIFIED., .F., .F.,
 ( 4, 2, 4 ),
 ( 6.952433221959954168E-18, 0.0006311571484586114269, 0.001262314296917216132 ),
 .UNSPECIFIED. ) ;
#12926 = DIRECTION ( 'NONE',  ( 1.000000000000000000, -6.938893903907226837E-18, 1.734723475976806709E-18 ) ) ;
#12927 = CARTESIAN_POINT ( 'NONE',  ( 109.1624594426973118, -0.01438905500501942193, 0.006914244825467924863 ) ) ;
#12928 = CARTESIAN_POINT ( 'NONE',  ( 8.186469829614365423, -71.65198613712890108, -131.0413692472661467 ) ) ;
#12929 = CARTESIAN_POINT ( 'NONE',  ( 32.73300124599739291, -99.90245962373785460, -62.10906484417343165 ) ) ;
#12930 = ORIENTED_EDGE ( 'NONE', *, *, #14999, .F. ) ;
#12931 = CIRCLE ( 'NONE', #23989, 20.00000000000000000 ) ;
#12932 = ADVANCED_FACE ( 'NONE', ( #10985 ), #18841, .F. ) ;
#12933 = ORIENTED_EDGE ( 'NONE', *, *, #8267, .F. ) ;
#12934 = CARTESIAN_POINT ( 'NONE',  ( 25.64681081121879203, 112.2483031020013442, 12.21581276189844800 ) ) ;
#12935 = CARTESIAN_POINT ( 'NONE',  ( -20.20700224038492721, 28.44216453106536946, -8.199606986804427677 ) ) ;
#12936 = DIRECTION ( 'NONE',  ( 0.000000000000000000, 5.223019709708190374E-21, -1.000000000000000000 ) ) ;
#12937 = CARTESIAN_POINT ( 'NONE',  ( 6.224689322667647851, -141.5842213414010473, -43.30635742325521420 ) ) ;
#12938 = FACE_OUTER_BOUND ( 'NONE', #9025, .T. ) ;
#12939 =( BOUNDED_SURFACE ( )  B_SPLINE_SURFACE ( 3, 1, ( 
 ( #8678, #8970 ),
 ( #26095, #2617 ),
 ( #4489, #28377 ),
 ( #11267, #17731 ) ),
 .UNSPECIFIED., .F., .F., .F. ) 
 B_SPLINE_SURFACE_WITH_KNOTS ( ( 4, 4 ),
 ( 2, 2 ),
 ( 0.000000000000000000, 1.000000000000000000 ),
 ( 0.000000000000000000, 1.000000000000000000 ),
 .UNSPECIFIED. ) 
 GEOMETRIC_REPRESENTATION_ITEM ( )  RATIONAL_B_SPLINE_SURFACE ( (
 ( 1.000000000000000000, 1.000000000000000000),
 ( 0.6386103224230316178, 0.9954351624131538845),
 ( 0.6386103224230316178, 0.9954351624131538845),
 ( 1.000000000000000000, 1.000000000000000000) ) ) 
 REPRESENTATION_ITEM ( '' )  SURFACE ( )  );
#12940 = CARTESIAN_POINT ( 'NONE',  ( 32.73300124599735739, -28.19767303745682341, 114.2056417606547285 ) ) ;
#12941 = CARTESIAN_POINT ( 'NONE',  ( 16.75465622695656265, -141.8562168210795278, 10.24707101927994657 ) ) ;
#12942 = VERTEX_POINT ( 'NONE', #22209 ) ;
#12943 = CARTESIAN_POINT ( 'NONE',  ( -6.574463467970655728, 51.07975593197905795, -5.014313797967199449 ) ) ;
#12944 = CARTESIAN_POINT ( 'NONE',  ( 30.59138290137886784, -115.8270707793589906, -9.457588828076334053 ) ) ;
#12945 = DIRECTION ( 'NONE',  ( 0.000000000000000000, 5.223019709708116647E-21, -1.000000000000000000 ) ) ;
#12946 = B_SPLINE_CURVE_WITH_KNOTS ( 'NONE', 3,
 ( #9394, #17995, #7369, #18277, #26922, #448, #3052, #16137 ),
 .UNSPECIFIED., .F., .F.,
 ( 4, 2, 2, 4 ),
 ( 0.000000000000000000, 0.0002429592666046677884, 0.0004859185332093355768, 0.0009718370664186791767 ),
 .UNSPECIFIED. ) ;
#12947 = FACE_OUTER_BOUND ( 'NONE', #28238, .T. ) ;
#12948 = ORIENTED_EDGE ( 'NONE', *, *, #619, .F. ) ;
#12949 = CARTESIAN_POINT ( 'NONE',  ( 1.893872463202028955, 43.94661640106022560, 138.3372034345892416 ) ) ;
#12950 = CARTESIAN_POINT ( 'NONE',  ( 25.64681081121879203, -12.21581276189731469, -112.2483031020014579 ) ) ;
#12951 = ORIENTED_EDGE ( 'NONE', *, *, #6081, .F. ) ;
#12952 = B_SPLINE_CURVE_WITH_KNOTS ( 'NONE', 3,
 ( #26146, #6437, #15768, #4265, #17499, #15335 ),
 .UNSPECIFIED., .F., .F.,
 ( 4, 2, 4 ),
 ( 1.436393986538261525E-17, 0.0006311636237756931139, 0.001262327247551371916 ),
 .UNSPECIFIED. ) ;
#12953 = ORIENTED_EDGE ( 'NONE', *, *, #25489, .T. ) ;
#12954 = ORIENTED_EDGE ( 'NONE', *, *, #5207, .T. ) ;
#12955 = VECTOR ( 'NONE', #27228, 999.9999999999998863 ) ;
#12956 = DIRECTION ( 'NONE',  ( 0.5946245182733607137, 0.2512550613902226337, -0.7637359336799396381 ) ) ;
#12957 = CARTESIAN_POINT ( 'NONE',  ( 0.000000000000000000, 0.000000000000000000, 0.000000000000000000 ) ) ;
#12958 = CARTESIAN_POINT ( 'NONE',  ( -1.056502255334264895, -37.35734037467652513, -26.51074901220491498 ) ) ;
#12959 = EDGE_CURVE ( 'NONE', #1293, #17227, #14012, .T. ) ;
#12960 = CARTESIAN_POINT ( 'NONE',  ( 109.1778270068192853, 0.0003511581237513579715, 0.009307953841270271214 ) ) ;
#12961 = ORIENTED_EDGE ( 'NONE', *, *, #1235, .T. ) ;
#12962 = EDGE_CURVE ( 'NONE', #2563, #6704, #15384, .T. ) ;
#12963 = CIRCLE ( 'NONE', #16657, 151.1787379149930359 ) ;
#12964 = ORIENTED_EDGE ( 'NONE', *, *, #21012, .T. ) ;
#12965 = CARTESIAN_POINT ( 'NONE',  ( -22.23226125620929139, 30.68305173820436593, 7.677408153693709991 ) ) ;
#12966 = CARTESIAN_POINT ( 'NONE',  ( 1.833750490713712322, -44.58740205676232193, -138.0897889879343552 ) ) ;
#12967 = EDGE_CURVE ( 'NONE', #5567, #20545, #17778, .T. ) ;
#12968 = CARTESIAN_POINT ( 'NONE',  ( 2.108393763691216893, -1.280847988472779697, 145.2872457912031905 ) ) ;
#12969 = CARTESIAN_POINT ( 'NONE',  ( -1.045287976400362417, -12.68782741917263657, 44.00138577190661948 ) ) ;
#12970 = VECTOR ( 'NONE', #5106, 999.9999999999998863 ) ;
#12971 = CARTESIAN_POINT ( 'NONE',  ( -1.056502255334265339, 36.75727364034771938, 27.33667001641128991 ) ) ;
#12972 = CARTESIAN_POINT ( 'NONE',  ( -1.259972190295308714, -35.85909728507027694, 28.82609802125297449 ) ) ;
#12973 = CARTESIAN_POINT ( 'NONE',  ( -7.733045908741344121, 10.42750254442610114, 51.44704017882764191 ) ) ;
#12974 = VECTOR ( 'NONE', #17112, 1000.000000000000227 ) ;
#12975 = CARTESIAN_POINT ( 'NONE',  ( -20.57838717382308147, -10.78122205916981358, 27.96569011373096814 ) ) ;
#12976 = CARTESIAN_POINT ( 'NONE',  ( -40.00000000000000000, 0.000000000000000000, 0.000000000000000000 ) ) ;
#12977 = CARTESIAN_POINT ( 'NONE',  ( 32.73300124599732186, 0.000000000000000000, 0.000000000000000000 ) ) ;
#12978 = CARTESIAN_POINT ( 'NONE',  ( 13.36082413113061307, 127.3428651193259640, -84.67697637120282650 ) ) ;
#12979 = EDGE_LOOP ( 'NONE', ( #13831, #7340 ) ) ;
#12980 = ORIENTED_EDGE ( 'NONE', *, *, #11374, .F. ) ;
#12981 = CARTESIAN_POINT ( 'NONE',  ( -28.13707043255157103, -6.342158660426852279, 22.00298671236746273 ) ) ;
#12982 = CARTESIAN_POINT ( 'NONE',  ( 10.93730112725999248, 42.00474393596446987, -145.2260730187398110 ) ) ;
#12983 = B_SPLINE_CURVE_WITH_KNOTS ( 'NONE', 3,
 ( #21528, #25997, #4395, #21821, #10884, #15173, #23994, #4110 ),
 .UNSPECIFIED., .F., .F.,
 ( 4, 2, 2, 4 ),
 ( 1.734723475976807094E-18, 0.0002429588503611240324, 0.0004859177007222463302, 0.0009718354014444961298 ),
 .UNSPECIFIED. ) ;
#12984 = ORIENTED_EDGE ( 'NONE', *, *, #8815, .F. ) ;
#12985 = B_SPLINE_CURVE_WITH_KNOTS ( 'NONE', 3,
 ( #21544, #10481, #23598, #19118, #12344, #25740, #10216, #18977, #21409, #8057 ),
 .UNSPECIFIED., .F., .F.,
 ( 4, 2, 2, 2, 4 ),
 ( 2.847672227753435151E-16, 0.0003346187017559057865, 0.0006692374035115268615, 0.001003856105267147665, 0.001338474807022768795 ),
 .UNSPECIFIED. ) ;
#12986 = B_SPLINE_CURVE_WITH_KNOTS ( 'NONE', 3,
 ( #2486, #6977, #13423, #11279, #26814, #6689, #15727, #7122 ),
 .UNSPECIFIED., .F., .F.,
 ( 4, 2, 2, 4 ),
 ( 0.000000000000000000, 0.002761524886576652380, 0.005523049773153304760, 0.01104609954630660952 ),
 .UNSPECIFIED. ) ;
#12987 = ADVANCED_FACE ( 'NONE', ( #183 ), #19917, .F. ) ;
#12988 = ORIENTED_EDGE ( 'NONE', *, *, #10305, .F. ) ;
#12989 = ORIENTED_EDGE ( 'NONE', *, *, #12388, .T. ) ;
#12990 = AXIS2_PLACEMENT_3D ( 'NONE', #1579, #25635, #5066 ) ;
#12991 = ADVANCED_FACE ( 'NONE', ( #19476 ), #11854, .F. ) ;
#12992 = VECTOR ( 'NONE', #21474, 1000.000000000000114 ) ;
#12993 = CARTESIAN_POINT ( 'NONE',  ( -20.57838717382308502, 25.16001208503106668, -16.28767523336130196 ) ) ;
#12994 = CARTESIAN_POINT ( 'NONE',  ( 1.834118845439484335, 45.01070051384772341, -137.9527673765101099 ) ) ;
#12995 = EDGE_CURVE ( 'NONE', #12174, #7268, #19175, .T. ) ;
#12996 = EDGE_CURVE ( 'NONE', #25305, #24670, #22968, .T. ) ;
#12997 = DIRECTION ( 'NONE',  ( -1.000000000000000000, 6.938893903907226837E-18, -1.734723475976806709E-18 ) ) ;
#12998 = CARTESIAN_POINT ( 'NONE',  ( 2.430230287190581429, 116.8646894862412182, 86.70145658344696926 ) ) ;
#12999 = DIRECTION ( 'NONE',  ( -1.000000000000000000, -0.000000000000000000, -0.000000000000000000 ) ) ;
#13000 = CARTESIAN_POINT ( 'NONE',  ( 25.64670758986459376, 23.96231489925043334, -110.3390515846396056 ) ) ;
#13001 = B_SPLINE_CURVE_WITH_KNOTS ( 'NONE', 3,
 ( #11176, #24425, #13606, #231 ),
 .UNSPECIFIED., .F., .F.,
 ( 4, 4 ),
 ( 1.904170172768910460E-16, 0.001982023823822945917 ),
 .UNSPECIFIED. ) ;
#13002 = CARTESIAN_POINT ( 'NONE',  ( 9.884929003653608603, -141.8132360130354357, -50.49804566712268894 ) ) ;
#13003 = CARTESIAN_POINT ( 'NONE',  ( -1.045287976400351981, 36.12803364096590997, -28.14015102489844011 ) ) ;
#13004 = ORIENTED_EDGE ( 'NONE', *, *, #22614, .F. ) ;
#13005 = EDGE_LOOP ( 'NONE', ( #10650, #17, #26148, #4701 ) ) ;
#13007 = CARTESIAN_POINT ( 'NONE',  ( -12.94347594948482083, -33.69581619287849605, 35.22469990145643948 ) ) ;
#13006 = DIRECTION ( 'NONE',  ( 0.000000000000000000, 0.000000000000000000, 1.000000000000000000 ) ) ;
#13008 = CARTESIAN_POINT ( 'NONE',  ( 25.69398547355841700, 22.75551036952080253, -110.6264597420657765 ) ) ;
#13009 = CARTESIAN_POINT ( 'NONE',  ( 109.1721716018069657, 0.01699510305644695227, 0.001583175916620114046 ) ) ;
#13010 = CARTESIAN_POINT ( 'NONE',  ( -1.044557008772712070, -43.01636061108997922, -15.70482370518800153 ) ) ;
#13011 = CARTESIAN_POINT ( 'NONE',  ( 5.340103556456546663, 146.8647350107031855, -13.12023871800969310 ) ) ;
#13012 = ORIENTED_EDGE ( 'NONE', *, *, #15755, .T. ) ;
#13013 = FACE_OUTER_BOUND ( 'NONE', #4380, .T. ) ;
#13014 = CIRCLE ( 'NONE', #20365, 12.50000000000000000 ) ;
#13015 = CARTESIAN_POINT ( 'NONE',  ( 1.893872463202048495, 117.9862474593107891, -84.54426271294305195 ) ) ;
#13016 = CARTESIAN_POINT ( 'NONE',  ( 26.28373643307402574, -88.40064398364015119, -91.96212244992481999 ) ) ;
#13017 = ORIENTED_EDGE ( 'NONE', *, *, #4573, .F. ) ;
#13018 = EDGE_LOOP ( 'NONE', ( #2033, #11720, #8405, #14309 ) ) ;
#13019 = FACE_OUTER_BOUND ( 'NONE', #1514, .T. ) ;
#13020 = CARTESIAN_POINT ( 'NONE',  ( 25.64681081121879203, 107.2555980796241215, 35.28660243342585545 ) ) ;
#13021 = VERTEX_POINT ( 'NONE', #24810 ) ;
#13022 = CARTESIAN_POINT ( 'NONE',  ( -28.13707043255157103, 22.88591869784691113, 0.7675454997507791255 ) ) ;
#13023 = ADVANCED_FACE ( 'NONE', ( #5356 ), #22716, .F. ) ;
#13024 = AXIS2_PLACEMENT_3D ( 'NONE', #21906, #11250, #6946 ) ;
#13025 = EDGE_CURVE ( 'NONE', #11340, #8983, #25712, .T. ) ;
#13026 = ORIENTED_EDGE ( 'NONE', *, *, #4130, .F. ) ;
#13027 = CARTESIAN_POINT ( 'NONE',  ( -55.24340739397742084, 0.003826481709804142178, -0.009386184976286654491 ) ) ;
#13028 =( REPRESENTATION_RELATIONSHIP ('NONE','NONE', #15430, #22271 ) REPRESENTATION_RELATIONSHIP_WITH_TRANSFORMATION ( #23717 )SHAPE_REPRESENTATION_RELATIONSHIP( ) );
#13029 = CARTESIAN_POINT ( 'NONE',  ( 26.11404676487259024, 76.59696442953192275, 83.38016054979810576 ) ) ;
#13030 = CARTESIAN_POINT ( 'NONE',  ( -8.786685647604887350, 53.04920435127183254, -7.199674155859138835 ) ) ;
#13031 = CARTESIAN_POINT ( 'NONE',  ( 109.1778270068192853, -0.008646067828082863033, -0.003465086990435458942 ) ) ;
#13032 = CARTESIAN_POINT ( 'NONE',  ( -1.045287976400383290, -36.12803364096628655, -28.14015102489793918 ) ) ;
#13033 = B_SPLINE_CURVE_WITH_KNOTS ( 'NONE', 3,
 ( #3170, #26761, #9376, #7218 ),
 .UNSPECIFIED., .F., .F.,
 ( 4, 4 ),
 ( 0.000000000000000000, 0.01077107196513867222 ),
 .UNSPECIFIED. ) ;
#13034 = DIRECTION ( 'NONE',  ( 0.5914120900931443270, 0.4101107478122118510, -0.6942916636548122078 ) ) ;
#13035 = DIRECTION ( 'NONE',  ( 0.000000000000000000, 5.223019709707975211E-21, -1.000000000000000000 ) ) ;
#13036 = CARTESIAN_POINT ( 'NONE',  ( 26.11404676487257603, -110.5078194225159223, -24.64483677384961879 ) ) ;
#13037 = CARTESIAN_POINT ( 'NONE',  ( 25.64681081121879203, -45.54494737132156246, -103.3177883989783936 ) ) ;
#13039 = CARTESIAN_POINT ( 'NONE',  ( -20.20700224038492721, -29.58392382092672790, 0.9908225410481621420 ) ) ;
#13038 = CARTESIAN_POINT ( 'NONE',  ( 55.49584447822657296, -72.55110015779771970, 0.2676470673954122192 ) ) ;
#13040 = EDGE_LOOP ( 'NONE', ( #14612, #20546, #27289, #14582 ) ) ;
#13041 = VERTEX_POINT ( 'NONE', #3200 ) ;
#13042 = CARTESIAN_POINT ( 'NONE',  ( 28.43349137099853152, 119.3601175884732299, 34.52178142065567101 ) ) ;
#13043 = CARTESIAN_POINT ( 'NONE',  ( -1.463510566862821660, 25.15876608740871490, 38.76366072687751796 ) ) ;
#13044 = FACE_OUTER_BOUND ( 'NONE', #22158, .T. ) ;
#13045 = CARTESIAN_POINT ( 'NONE',  ( 119.2224693531408803, 90.00000000000005684, 39.99999999999999289 ) ) ;
#13046 = CARTESIAN_POINT ( 'NONE',  ( -6.588769196390762417, 4.956336548259653974, -51.10255870850470217 ) ) ;
#13047 = CARTESIAN_POINT ( 'NONE',  ( -2.265401668238149036, 17.02144111536879123, -43.82493763960390254 ) ) ;
#13048 = VERTEX_POINT ( 'NONE', #465 ) ;
#13049 = CARTESIAN_POINT ( 'NONE',  ( -1.058197053496171325, 15.81317659443684143, -42.99116279335158453 ) ) ;
#13050 = CARTESIAN_POINT ( 'NONE',  ( -7.733045908741342345, 25.81515396910926086, 45.70676731105690749 ) ) ;
#13051 = FACE_OUTER_BOUND ( 'NONE', #18335, .T. ) ;
#13052 = CARTESIAN_POINT ( 'NONE',  ( -20.57838717382308147, -29.92853265176830746, 1.611677988432673070 ) ) ;
#13053 = B_SPLINE_CURVE_WITH_KNOTS ( 'NONE', 3,
 ( #13289, #205, #483, #8993, #4664, #13431, #25547, #12004, #18475, #21050, #1064, #18911, #27538 ),
 .UNSPECIFIED., .F., .F.,
 ( 4, 3, 3, 3, 4 ),
 ( 8.673617379884035472E-18, 0.0007657099931970570922, 0.001531419946797920890, 0.002296279302920155134, 0.003061450627205761568 ),
 .UNSPECIFIED. ) ;
#13054 = CARTESIAN_POINT ( 'NONE',  ( 10.93730112726003156, 115.5857507957718440, -97.44200844886164248 ) ) ;
#13055 = ORIENTED_EDGE ( 'NONE', *, *, #17942, .F. ) ;
#13056 = FACE_OUTER_BOUND ( 'NONE', #10225, .T. ) ;
#13057 = ADVANCED_FACE ( 'NONE', ( #20751 ), #1913, .F. ) ;
#13058 = CARTESIAN_POINT ( 'NONE',  ( 1.833485406944043827, 14.63699153649552365, -144.3694338680883789 ) ) ;
#13060 = ADVANCED_FACE ( 'NONE', ( #752 ), #25663, .F. ) ;
#13059 = CARTESIAN_POINT ( 'NONE',  ( 2.108985857320904600, -60.26444811757312436, -132.2056553747751195 ) ) ;
#13061 = B_SPLINE_CURVE_WITH_KNOTS ( 'NONE', 3,
 ( #19366, #21389, #23719, #14766 ),
 .UNSPECIFIED., .F., .F.,
 ( 4, 4 ),
 ( 3.324202758929661745E-16, 0.01077107486149808495 ),
 .UNSPECIFIED. ) ;
#13062 = ORIENTED_EDGE ( 'NONE', *, *, #26125, .F. ) ;
#13063 = DIRECTION ( 'NONE',  ( -1.000000000000000000, 0.000000000000000000, 0.000000000000000000 ) ) ;
#13064 = ADVANCED_FACE ( 'NONE', ( #5498 ), #21776, .F. ) ;
#13065 = CARTESIAN_POINT ( 'NONE',  ( 26.11404676487257603, 65.63269960453364149, -92.25884714080342519 ) ) ;
#13066 = CARTESIAN_POINT ( 'NONE',  ( 2.433796855181233454, 144.8571464219889151, 13.76554153471742481 ) ) ;
#13067 = CARTESIAN_POINT ( 'NONE',  ( -1.058473599757806971, -12.47539220917832914, 44.07591602137168252 ) ) ;
#13068 = EDGE_CURVE ( 'NONE', #7628, #23299, #13696, .T. ) ;
#13069 = CARTESIAN_POINT ( 'NONE',  ( -1.058473599757834283, 35.99997772736212198, -28.32531354681296420 ) ) ;
#13070 = CARTESIAN_POINT ( 'NONE',  ( 2.263178607246703056, 132.2496131833837012, -60.41552769843686121 ) ) ;
#13071 = CARTESIAN_POINT ( 'NONE',  ( 1.833485406944057594, -138.1714136985305572, -44.33323125130066700 ) ) ;
#13072 = CARTESIAN_POINT ( 'NONE',  ( -8.259864102781634188, -6.590267880897305197, -52.60025989855206063 ) ) ;
#13073 = CARTESIAN_POINT ( 'NONE',  ( 1.833838850855476155, -132.6005571022083700, 58.94016894581421440 ) ) ;
#13074 = CARTESIAN_POINT ( 'NONE',  ( -20.90916690077964901, -18.74041620980142753, 34.84883504600970383 ) ) ;
#13075 = CARTESIAN_POINT ( 'NONE',  ( -25.21435515916025594, 1.749597353048488237E-16, -4.373993382621220594E-17 ) ) ;
#13076 = CARTESIAN_POINT ( 'NONE',  ( 2.433796855181205476, -71.49415740224986848, -126.7346379669263001 ) ) ;
#13077 = CARTESIAN_POINT ( 'NONE',  ( -18.41936578851709072, 38.22933728004715448, 18.42310649277586876 ) ) ;
#13078 = EDGE_LOOP ( 'NONE', ( #3614, #25834, #23111, #6833 ) ) ;
#13079 = ORIENTED_EDGE ( 'NONE', *, *, #26660, .T. ) ;
#13080 = CARTESIAN_POINT ( 'NONE',  ( -20.47566338032520861, -29.82700953060484395, 1.586617869344197018 ) ) ;
#13081 = CARTESIAN_POINT ( 'NONE',  ( -23.77929240705206837, 32.66578242509746133, -15.74261278740683778 ) ) ;
#13082 = CARTESIAN_POINT ( 'NONE',  ( 1.832998868059858122, 15.69902610990566849, -144.2584710144578821 ) ) ;
#13083 = CARTESIAN_POINT ( 'NONE',  ( 109.1778270068192853, -0.007736698406806062980, 0.005186985107080914308 ) ) ;
#13084 = CARTESIAN_POINT ( 'NONE',  ( 32.73300124599738581, -39.98094346392232268, -110.6325518752277759 ) ) ;
#13085 = CARTESIAN_POINT ( 'NONE',  ( 25.64681081121879203, -91.59071981940525120, -66.03065707439029097 ) ) ;
#13086 = CARTESIAN_POINT ( 'NONE',  ( -23.79223135445719706, -24.83942264280416978, -22.01133905265676916 ) ) ;
#13087 = VERTEX_POINT ( 'NONE', #11546 ) ;
#13088 = CARTESIAN_POINT ( 'NONE',  ( -28.13707043255157103, -22.00298671236735615, 6.342158660427235972 ) ) ;
#13089 = FACE_OUTER_BOUND ( 'NONE', #8949, .T. ) ;
#13090 = FACE_OUTER_BOUND ( 'NONE', #4405, .T. ) ;
#13091 = FACE_OUTER_BOUND ( 'NONE', #8233, .T. ) ;
#13092 = CARTESIAN_POINT ( 'NONE',  ( -1.044556982611267948, -43.01635920718339179, 15.70482750345280820 ) ) ;
#13093 = ADVANCED_FACE ( 'NONE', ( #614, #9405 ), #14981, .T. ) ;
#13094 = ORIENTED_EDGE ( 'NONE', *, *, #21290, .F. ) ;
#13095 = CARTESIAN_POINT ( 'NONE',  ( 1.833691583653537682, -108.0753610255259360, 96.83253123394176498 ) ) ;
#13096 = CARTESIAN_POINT ( 'NONE',  ( -20.20997486282892552, 1.395963739018065216E-16, 29.60348406988233450 ) ) ;
#13097 = VERTEX_POINT ( 'NONE', #14419 ) ;
#13098 = ADVANCED_FACE ( 'NONE', ( #7977 ), #27484, .F. ) ;
#13099 = B_SPLINE_CURVE_WITH_KNOTS ( 'NONE', 3,
 ( #17750, #22072, #4660, #4506, #26666, #24249, #13285 ),
 .UNSPECIFIED., .F., .F.,
 ( 4, 3, 4 ),
 ( 5.935087083004135664E-16, 0.02816610861753244752, 0.04000277880656274987 ),
 .UNSPECIFIED. ) ;
#13100 = ORIENTED_EDGE ( 'NONE', *, *, #5940, .F. ) ;
#13101 = B_SPLINE_CURVE_WITH_KNOTS ( 'NONE', 3,
 ( #12437, #1088, #27415, #23546, #16913, #23128, #2029, #27555, #21227, #3809, #19594, #9876, #8661 ),
 .UNSPECIFIED., .F., .F.,
 ( 4, 3, 3, 3, 4 ),
 ( 9.813077866773594792E-18, 0.0007657099931970698858, 0.001531419946797932816, 0.002296279302920152098, 0.003061450627205747257 ),
 .UNSPECIFIED. ) ;
#13102 = EDGE_LOOP ( 'NONE', ( #7712, #3032, #16416, #10326 ) ) ;
#13103 = ADVANCED_FACE ( 'NONE', ( #16741 ), #17724, .F. ) ;
#13104 = CARTESIAN_POINT ( 'NONE',  ( -1.031422197589716205, 45.78027046666444733, 1.530725436377623927 ) ) ;
#13105 = CARTESIAN_POINT ( 'NONE',  ( 109.1778270068192853, 0.003210287141653799838, 0.008743876326162606724 ) ) ;
#13106 = ORIENTED_EDGE ( 'NONE', *, *, #11709, .F. ) ;
#13107 = CARTESIAN_POINT ( 'NONE',  ( -10.86508079875812705, -45.04061326950857591, 24.22249093393325836 ) ) ;
#13108 =( BOUNDED_SURFACE ( )  B_SPLINE_SURFACE ( 3, 1, ( 
 ( #24211, #19454 ),
 ( #24351, #4467 ),
 ( #26072, #13242 ),
 ( #6504, #28222 ) ),
 .UNSPECIFIED., .F., .F., .F. ) 
 B_SPLINE_SURFACE_WITH_KNOTS ( ( 4, 4 ),
 ( 2, 2 ),
 ( 0.000000000000000000, 1.000000000000000000 ),
 ( 0.000000000000000000, 1.000000000000000000 ),
 .UNSPECIFIED. ) 
 GEOMETRIC_REPRESENTATION_ITEM ( )  RATIONAL_B_SPLINE_SURFACE ( (
 ( 1.000000000000000000, 1.000000000000000000),
 ( 0.9593753223639863714, 0.9995975284513187731),
 ( 0.9593753223639863714, 0.9995975284513187731),
 ( 1.000000000000000000, 1.000000000000000000) ) ) 
 REPRESENTATION_ITEM ( '' )  SURFACE ( )  );
#13109 = CARTESIAN_POINT ( 'NONE',  ( 55.79472521941426777, 59.28412330436359667, -42.17269936297579136 ) ) ;
#13110 = VERTEX_POINT ( 'NONE', #1188 ) ;
#13111 = DIRECTION ( 'NONE',  ( 1.000000000000000000, -6.938893903907226837E-18, 1.734723475976806709E-18 ) ) ;
#13112 = CARTESIAN_POINT ( 'NONE',  ( 10.93730112725932635, 0.000000000000000000, 0.000000000000000000 ) ) ;
#13113 = CARTESIAN_POINT ( 'NONE',  ( -55.24271866751342941, 0.006671293903669565407, -0.006757859501006440936 ) ) ;
#13114 = CARTESIAN_POINT ( 'NONE',  ( -8.259864102781673267, 25.58601832199082793, -46.42816643551579148 ) ) ;
#13115 = DIRECTION ( 'NONE',  ( -0.000000000000000000, -0.000000000000000000, 1.000000000000000000 ) ) ;
#13116 = CARTESIAN_POINT ( 'NONE',  ( -55.24271866751342941, -0.009388511352197387999, -0.001425019990782294558 ) ) ;
#13117 = CARTESIAN_POINT ( 'NONE',  ( -9.156249394959713683, 25.18996226954615736, -48.32878616081018208 ) ) ;
#13118 = CARTESIAN_POINT ( 'NONE',  ( 99.22246935314079508, 69.99999999999998579, -40.00000000000000711 ) ) ;
#13119 = LINE ( 'NONE', #1892, #2426 ) ;
#13120 = CARTESIAN_POINT ( 'NONE',  ( 2.433796855181219243, 142.0211193075560061, -31.67151202412830813 ) ) ;
#13121 = ORIENTED_EDGE ( 'NONE', *, *, #23837, .F. ) ;
#13122 = ORIENTED_EDGE ( 'NONE', *, *, #22436, .T. ) ;
#13123 = CARTESIAN_POINT ( 'NONE',  ( 109.1586900883932856, 0.007137750914550311347, -0.0001010081143976270922 ) ) ;
#13124 = ORIENTED_EDGE ( 'NONE', *, *, #7499, .F. ) ;
#13125 = EDGE_CURVE ( 'NONE', #11630, #2861, #14844, .T. ) ;
#13126 = ORIENTED_EDGE ( 'NONE', *, *, #19306, .F. ) ;
#13127 = VERTEX_POINT ( 'NONE', #14698 ) ;
#13128 = CARTESIAN_POINT ( 'NONE',  ( 109.1586059443104944, 0.003774052605966631002, 0.005983234375914163114 ) ) ;
#13129 = EDGE_CURVE ( 'NONE', #27960, #25020, #2320, .T. ) ;
#13130 = B_SPLINE_CURVE_WITH_KNOTS ( 'NONE', 3,
 ( #767, #16018, #11562, #22813 ),
 .UNSPECIFIED., .F., .F.,
 ( 4, 4 ),
 ( 1.962615573354718958E-17, 0.008383560773332712074 ),
 .UNSPECIFIED. ) ;
#13131 = EDGE_CURVE ( 'NONE', #24385, #28456, #26702, .T. ) ;
#13132 = CARTESIAN_POINT ( 'NONE',  ( -20.20700224038492010, -18.19058640100240254, -23.35150625415651859 ) ) ;
#13133 = CARTESIAN_POINT ( 'NONE',  ( -20.24399999263414429, -16.36687688782875938, -24.70869149526196651 ) ) ;
#13134 = FACE_OUTER_BOUND ( 'NONE', #8256, .T. ) ;
#13135 = FACE_OUTER_BOUND ( 'NONE', #21623, .T. ) ;
#13136 = CARTESIAN_POINT ( 'NONE',  ( -1.048172774974291066, 1.020161070261757841, 45.78636862970791555 ) ) ;
#13137 = CARTESIAN_POINT ( 'NONE',  ( 25.64703792032472052, -110.4127989088531336, 23.62108504469209436 ) ) ;
#13138 = CARTESIAN_POINT ( 'NONE',  ( 2.263178607246671525, 60.41552769843821125, 132.2496131833831328 ) ) ;
#13139 = CARTESIAN_POINT ( 'NONE',  ( 55.49584447822657296, 66.38758986585156663, -29.26468316696706751 ) ) ;
#13140 = CARTESIAN_POINT ( 'NONE',  ( 10.93730112726003156, 108.9902118373755684, -104.7670965581001781 ) ) ;
#13141 = VERTEX_POINT ( 'NONE', #25936 ) ;
#13142 = ORIENTED_EDGE ( 'NONE', *, *, #26660, .F. ) ;
#13144 = FACE_OUTER_BOUND ( 'NONE', #28232, .T. ) ;
#13143 = CARTESIAN_POINT ( 'NONE',  ( -1.019300379054419947, 2.023851374322675589, -45.76814864815091255 ) ) ;
#13145 = PRODUCT_RELATED_PRODUCT_CATEGORY ( 'part', '', ( #15175 ) ) ;
#13146 = CARTESIAN_POINT ( 'NONE',  ( 32.73300124599735739, 75.82012867748483131, 89.94078864464094636 ) ) ;
#13147 = FACE_OUTER_BOUND ( 'NONE', #18642, .T. ) ;
#13148 = CARTESIAN_POINT ( 'NONE',  ( -24.53239521893647890, -29.54733954334097135, 16.68574937151005599 ) ) ;
#13149 = ORIENTED_EDGE ( 'NONE', *, *, #10806, .F. ) ;
#13150 = CARTESIAN_POINT ( 'NONE',  ( -4.473127245936431073, 31.51789735524192793, -37.94261489385728936 ) ) ;
#13151 = CARTESIAN_POINT ( 'NONE',  ( -1.619063947482197729, -25.20140673341345305, 38.92136151114934961 ) ) ;
#13152 = CARTESIAN_POINT ( 'NONE',  ( -25.21435515916025594, 1.749597353048488237E-16, -4.373993382621220594E-17 ) ) ;
#13153 = ORIENTED_EDGE ( 'NONE', *, *, #11122, .F. ) ;
#13154 = ORIENTED_EDGE ( 'NONE', *, *, #24088, .F. ) ;
#13155 = EDGE_CURVE ( 'NONE', #3917, #8101, #22611, .T. ) ;
#13156 = CARTESIAN_POINT ( 'NONE',  ( 109.1586900883932856, -0.001385221016536901904, -0.007002774699553655259 ) ) ;
#13157 = ORIENTED_EDGE ( 'NONE', *, *, #20035, .T. ) ;
#13158 = CARTESIAN_POINT ( 'NONE',  ( 5.340103579038085080, 120.6284720963485029, 84.79482754232307684 ) ) ;
#13159 = VERTEX_POINT ( 'NONE', #19034 ) ;
#13160 = CARTESIAN_POINT ( 'NONE',  ( 1.831572820252008738, -138.3111855986063858, 43.90210991190574674 ) ) ;
#13161 = ORIENTED_EDGE ( 'NONE', *, *, #15688, .F. ) ;
#13162 = CARTESIAN_POINT ( 'NONE',  ( 2.430230287190592531, -118.5711603495675632, -84.35270093935378100 ) ) ;
#13163 = LINE ( 'NONE', #12741, #25352 ) ;
#13164 = CARTESIAN_POINT ( 'NONE',  ( -20.57838717382308147, 27.96569011373101077, 10.78122205916971055 ) ) ;
#13165 = CARTESIAN_POINT ( 'NONE',  ( 109.1586900883932856, -0.002109621908814847055, 0.006819617742893393543 ) ) ;
#13166 = CARTESIAN_POINT ( 'NONE',  ( -55.25297051322618813, 0.01483298743815085648, 0.001818774723749092123 ) ) ;
#13167 = CARTESIAN_POINT ( 'NONE',  ( 32.73300124599738581, -114.2056417606545864, -28.19767303745721065 ) ) ;
#13168 = CARTESIAN_POINT ( 'NONE',  ( -1.031422197589711987, 12.69107518035501414, -44.01264471863851213 ) ) ;
#13169 = CARTESIAN_POINT ( 'NONE',  ( -20.47566262905010248, 25.06314747784837138, -16.24827521404660047 ) ) ;
#13170 = CARTESIAN_POINT ( 'NONE',  ( 94.22246935314088034, -151.1871800109700246, -6.938893903907228378E-15 ) ) ;
#13171 = CARTESIAN_POINT ( 'NONE',  ( 21.16825799904933803, 130.1008673867299876, 37.62905626541736126 ) ) ;
#13172 = CARTESIAN_POINT ( 'NONE',  ( -1.045287976400365970, -25.66401692419961833, 37.92705037016786918 ) ) ;
#13173 = CARTESIAN_POINT ( 'NONE',  ( -1.049817751779876129, -43.71287583013717182, 13.66628317065032583 ) ) ;
#13174 = CARTESIAN_POINT ( 'NONE',  ( 109.1778270068192853, 0.009220257877172552408, 0.001322180554006217911 ) ) ;
#13175 = CARTESIAN_POINT ( 'NONE',  ( 1.833206310202336820, -125.2945016693816598, 73.19872434058744659 ) ) ;
#13176 = EDGE_CURVE ( 'NONE', #28263, #8520, #5136, .T. ) ;
#13177 = ORIENTED_EDGE ( 'NONE', *, *, #22844, .F. ) ;
#13178 = ADVANCED_FACE ( 'NONE', ( #12131 ), #4872, .F. ) ;
#13179 = B_SPLINE_CURVE_WITH_KNOTS ( 'NONE', 3,
 ( #4584, #24183, #2417, #11352, #15508, #26186, #22153, #6905 ),
 .UNSPECIFIED., .F., .F.,
 ( 4, 2, 2, 4 ),
 ( 0.000000000000000000, 0.0002429588503611127567, 0.0004859177007222255135, 0.0009718354014444878898 ),
 .UNSPECIFIED. ) ;
#13180 = CARTESIAN_POINT ( 'NONE',  ( -4.178947244162567465, -37.51424432987625579, 31.41809272265961539 ) ) ;
#13181 = CARTESIAN_POINT ( 'NONE',  ( 25.64681081121879203, -91.59071981940616070, 66.03065707438906884 ) ) ;
#13182 = CARTESIAN_POINT ( 'NONE',  ( 10.93730112725990367, -92.80059208661606363, -119.3442956573281748 ) ) ;
#13184 = ORIENTED_EDGE ( 'NONE', *, *, #19493, .F. ) ;
#13183 = EDGE_CURVE ( 'NONE', #10454, #3000, #19719, .T. ) ;
#13185 = CARTESIAN_POINT ( 'NONE',  ( -1.031422197589711764, -12.69107518035532856, -44.01264471863841266 ) ) ;
#13186 = CARTESIAN_POINT ( 'NONE',  ( 109.1778270068192853, 0.001591747944966651496, -0.009177562596833053685 ) ) ;
#13187 = CARTESIAN_POINT ( 'NONE',  ( 1.833485406944043827, -97.49333871408762775, 107.4794113447406119 ) ) ;
#13188 = ORIENTED_EDGE ( 'NONE', *, *, #7970, .F. ) ;
#13189 = CARTESIAN_POINT ( 'NONE',  ( 10.93730112725994275, -36.23586118136433498, -146.7718404940647190 ) ) ;
#13190 = CARTESIAN_POINT ( 'NONE',  ( 25.64660436782558861, 65.89729635303032751, -91.68669413043076588 ) ) ;
#13191 = EDGE_LOOP ( 'NONE', ( #7701, #28473, #15142, #10843 ) ) ;
#13192 = CARTESIAN_POINT ( 'NONE',  ( 25.64708010899968116, 103.1273237223355750, -45.97512510001799768 ) ) ;
#13193 = CARTESIAN_POINT ( 'NONE',  ( -1.239374126674604337, 44.48112152129363750, 11.92219841463783503 ) ) ;
#13194 = CARTESIAN_POINT ( 'NONE',  ( 14.74894986621300319, 4.490279961725991446E-15, -37.50000000000001421 ) ) ;
#13195 = CARTESIAN_POINT ( 'NONE',  ( -1.058473599757823846, -45.77379534793241334, 1.755404039369906188 ) ) ;
#13196 = LINE ( 'NONE', #4424, #22793 ) ;
#13197 = CARTESIAN_POINT ( 'NONE',  ( 10.93730112725997294, 26.59437931460951177, -148.8212007290660210 ) ) ;
#13198 = CARTESIAN_POINT ( 'NONE',  ( -9.156249394959713683, 48.78605533024740737, -24.29252099376508056 ) ) ;
#13199 = B_SPLINE_CURVE_WITH_KNOTS ( 'NONE', 3,
 ( #19796, #89, #26423, #6722, #15469, #22406, #26845 ),
 .UNSPECIFIED., .F., .F.,
 ( 4, 3, 4 ),
 ( 0.000000000000000000, 0.02398743853561364353, 0.04000277880656225027 ),
 .UNSPECIFIED. ) ;
#13200 = CARTESIAN_POINT ( 'NONE',  ( -25.21435515916044423, -16.39063784838720395, 30.48034229288656505 ) ) ;
#13201 = CARTESIAN_POINT ( 'NONE',  ( 13.36082413113061307, 97.52406103376755198, 117.7941133658641917 ) ) ;
#13202 = CARTESIAN_POINT ( 'NONE',  ( 24.22246935314087324, 70.00000000000004263, 39.99999999999999289 ) ) ;
#13203 = CARTESIAN_POINT ( 'NONE',  ( -25.21435515916043357, 31.17620025257608418, 15.02493970636113474 ) ) ;
#13204 = EDGE_LOOP ( 'NONE', ( #3403, #18664, #12061, #4943 ) ) ;
#13205 = EDGE_CURVE ( 'NONE', #21575, #18167, #9278, .T. ) ;
#13206 = ORIENTED_EDGE ( 'NONE', *, *, #11221, .F. ) ;
#13207 = ORIENTED_EDGE ( 'NONE', *, *, #1801, .T. ) ;
#13208 = CARTESIAN_POINT ( 'NONE',  ( 32.73300124599741423, -92.86301839379967760, -72.21147546950645335 ) ) ;
#13209 = DIRECTION ( 'NONE',  ( 0.5946245182733608248, 0.6487139525627683145, 0.4749651461092318505 ) ) ;
#13210 = CARTESIAN_POINT ( 'NONE',  ( 109.1586900883932856, 0.005236795036860546551, -0.004851151255037378096 ) ) ;
#13211 = CARTESIAN_POINT ( 'NONE',  ( 2.063896406836609909, 60.31174178979808431, 132.1577797566308163 ) ) ;
#13212 = CARTESIAN_POINT ( 'NONE',  ( 1.833750490713643266, 72.78591676344139216, -125.5350013574263244 ) ) ;
#13213 = CARTESIAN_POINT ( 'NONE',  ( 5.340103556456522682, -43.36842540065395468, -140.9275371673311952 ) ) ;
#13214 = ADVANCED_FACE ( 'NONE', ( #10822 ), #6153, .F. ) ;
#13215 = ORIENTED_EDGE ( 'NONE', *, *, #10630, .F. ) ;
#13216 = DIRECTION ( 'NONE',  ( -1.000000000000000000, -0.000000000000000000, -0.000000000000000000 ) ) ;
#13217 = VECTOR ( 'NONE', #5335, 1000.000000000000114 ) ;
#13218 = CARTESIAN_POINT ( 'NONE',  ( -25.21435515916025594, 1.749597353048488237E-16, -4.373993382621220594E-17 ) ) ;
#13219 = CARTESIAN_POINT ( 'NONE',  ( 25.98107933586718943, -113.1286487641200722, -1.091357942391775637 ) ) ;
#13220 = EDGE_CURVE ( 'NONE', #27068, #6724, #19569, .T. ) ;
#13221 = CARTESIAN_POINT ( 'NONE',  ( 1.833838850093517658, 1.769966374633376447E-14, 145.1097630783160923 ) ) ;
#13222 = CARTESIAN_POINT ( 'NONE',  ( 9.884929003653626367, 148.0628878137280537, 27.17402761732395433 ) ) ;
#13223 = ORIENTED_EDGE ( 'NONE', *, *, #26093, .T. ) ;
#13224 = CARTESIAN_POINT ( 'NONE',  ( 1.833838850093465700, -107.8375672471888294, 97.09738632348999943 ) ) ;
#13226 = CARTESIAN_POINT ( 'NONE',  ( 1.833809397773873417, -117.2915757704551396, -85.43729755723271069 ) ) ;
#13225 = B_SPLINE_CURVE_WITH_KNOTS ( 'NONE', 3,
 ( #21845, #11322, #15201, #13059, #8892, #24153 ),
 .UNSPECIFIED., .F., .F.,
 ( 4, 2, 4 ),
 ( 1.389302603484999005E-17, 0.0006311571484586102343, 0.001262314296917207241 ),
 .UNSPECIFIED. ) ;
#13227 = ORIENTED_EDGE ( 'NONE', *, *, #28235, .T. ) ;
#13228 = ORIENTED_EDGE ( 'NONE', *, *, #5717, .T. ) ;
#13229 = VERTEX_POINT ( 'NONE', #10954 ) ;
#13230 = CARTESIAN_POINT ( 'NONE',  ( 2.430230287190572103, 109.1043569252027083, -96.28466919683991421 ) ) ;
#13231 = CARTESIAN_POINT ( 'NONE',  ( 13.36082413113063083, 129.1512766091132676, -81.89226687791952486 ) ) ;
#13232 = CARTESIAN_POINT ( 'NONE',  ( 109.1721716018069657, -0.003350975118864069589, 0.01673651515803013454 ) ) ;
#13233 = B_SPLINE_CURVE_WITH_KNOTS ( 'NONE', 3,
 ( #8740, #15777, #24588, #4848, #11321, #20090 ),
 .UNSPECIFIED., .F., .F.,
 ( 4, 2, 4 ),
 ( 1.734723475976807094E-18, 0.0004335184443140234316, 0.0008670368886280451284 ),
 .UNSPECIFIED. ) ;
#13234 = EDGE_LOOP ( 'NONE', ( #10701, #8379, #16284, #7241 ) ) ;
#13235 = CARTESIAN_POINT ( 'NONE',  ( 1.833838850093465034, 72.55488452980864622, 125.6687394363099628 ) ) ;
#13236 = ORIENTED_EDGE ( 'NONE', *, *, #17373, .T. ) ;
#13237 = EDGE_CURVE ( 'NONE', #17251, #20822, #27474, .T. ) ;
#13238 = DIRECTION ( 'NONE',  ( 0.000000000000000000, 5.223019709708233256E-21, -1.000000000000000000 ) ) ;
#13239 = CARTESIAN_POINT ( 'NONE',  ( 55.49584447822657296, 66.38758986585115451, 29.26468316696795569 ) ) ;
#13240 = ADVANCED_FACE ( 'NONE', ( #17835 ), #23986, .F. ) ;
#13241 = CARTESIAN_POINT ( 'NONE',  ( -1.239374126674604337, -2.406737988131443906, -45.98822239537607715 ) ) ;
#13242 = CARTESIAN_POINT ( 'NONE',  ( -1.056502255334264895, -14.64009593116132457, -43.40574022158768486 ) ) ;
#13243 = CARTESIAN_POINT ( 'NONE',  ( 25.64681081121879203, -75.24277141833549365, 84.18689316040023130 ) ) ;
#13244 = CARTESIAN_POINT ( 'NONE',  ( -55.24728320129491266, 0.003868537197317211632, -0.01402509393918151964 ) ) ;
#13245 = CARTESIAN_POINT ( 'NONE',  ( -21.81686047589426636, -27.83628745321466624, -26.62923599424956933 ) ) ;
#13246 = CARTESIAN_POINT ( 'NONE',  ( -6.588769196390752647, -26.02756986588571309, -44.25609997968896892 ) ) ;
#13247 = EDGE_CURVE ( 'NONE', #12534, #12509, #4604, .T. ) ;
#13248 = CARTESIAN_POINT ( 'NONE',  ( -25.21435515916025594, 1.749597353048488237E-16, -4.373993382621220594E-17 ) ) ;
#13249 = CARTESIAN_POINT ( 'NONE',  ( -20.20612092514785019, -24.59769888281546102, -16.46550332780518033 ) ) ;
#13250 = CARTESIAN_POINT ( 'NONE',  ( -55.24390624410018802, 0.001451500391951047672, 0.01032895241566990016 ) ) ;
#13251 = VECTOR ( 'NONE', #8190, 1000.000000000000114 ) ;
#13252 = LINE ( 'NONE', #304, #18037 ) ;
#13253 = EDGE_CURVE ( 'NONE', #25791, #26744, #23926, .T. ) ;
#13254 = VERTEX_POINT ( 'NONE', #19864 ) ;
#13255 = CLOSED_SHELL ( 'NONE', ( #13734, #24560, #15064, #13610, #5239, #9833, #15513, #3708, #22270, #24950, #10675, #882, #16044, #26327, #26758, #26163, #21169, #20605, #2570, #22238, #21537, #15423, #27465, #5944, #17996, #18522, #11606, #1653, #27949, #20037, #23519, #13064, #2425, #27501, #13486, #27938, #14653, #18598, #6133, #6942, #7643, #14483, #1770, #25159, #18796, #9160, #17725, #28252, #13103, #5903, #20247, #27621, #2998, #27058, #19527, #26317, #18391, #11115, #14186, #1311, #4242, #19715, #10005, #23393, #10095, #8120, #23145, #3612, #13214, #27370, #26067, #19199, #13277, #25792, #18185, #2317, #10568, #16784, #7901, #19061, #19028, #22865, #5968, #19058, #18766, #12987, #8407, #10027, #23593, #20925, #26631, #14881, #5709, #14488, #11217, #21356, #16039, #25299, #16933, #12382, #8918, #22164, #19030, #15004, #2878, #18601, #11807, #17139, #683, #13640, #6861, #9638, #14118, #15438, #164, #2601, #18995, #26835, #11506, #24075, #21030, #6573, #1332, #8504, #4936, #9648, #18303, #980, #17247, #2080, #14832, #20850 ) ) ;
#13256 = VERTEX_POINT ( 'NONE', #15529 ) ;
#13257 = CARTESIAN_POINT ( 'NONE',  ( -28.41354790283022069, -1.249099604787238249, -23.16239616762930353 ) ) ;
#13258 = CARTESIAN_POINT ( 'NONE',  ( -1.031422197589711764, -28.14735071801717226, 36.13727897780157150 ) ) ;
#13259 = ORIENTED_EDGE ( 'NONE', *, *, #10984, .T. ) ;
#13260 = B_SPLINE_CURVE_WITH_KNOTS ( 'NONE', 3,
 ( #26839, #5395, #16626, #21611, #7424, #16331, #23400, #14307, #25420, #1083, #9723, #27550, #1218 ),
 .UNSPECIFIED., .F., .F.,
 ( 4, 3, 3, 3, 4 ),
 ( 6.938893903907227607E-18, 0.0007657099931970527554, 0.001531419946797919806, 0.002296279302920157302, 0.003061450627205762002 ),
 .UNSPECIFIED. ) ;
#13261 = VERTEX_POINT ( 'NONE', #23797 ) ;
#13262 = EDGE_LOOP ( 'NONE', ( #673, #8050, #8106, #1182 ) ) ;
#13263 =( BOUNDED_SURFACE ( )  B_SPLINE_SURFACE ( 3, 1, ( 
 ( #11963, #20739 ),
 ( #9665, #5341 ),
 ( #7521, #23826 ),
 ( #6127, #2052 ) ),
 .UNSPECIFIED., .F., .F., .F. ) 
 B_SPLINE_SURFACE_WITH_KNOTS ( ( 4, 4 ),
 ( 2, 2 ),
 ( 0.000000000000000000, 1.000000000000000000 ),
 ( 0.000000000000000000, 1.000000000000000000 ),
 .UNSPECIFIED. ) 
 GEOMETRIC_REPRESENTATION_ITEM ( )  RATIONAL_B_SPLINE_SURFACE ( (
 ( 1.000000000000000000, 1.000000000000000000),
 ( 0.9956975270656954757, 0.8568959468854893125),
 ( 0.9956975270656954757, 0.8568959468854893125),
 ( 1.000000000000000000, 1.000000000000000000) ) ) 
 REPRESENTATION_ITEM ( '' )  SURFACE ( )  );
#13264 = B_SPLINE_CURVE_WITH_KNOTS ( 'NONE', 3,
 ( #25705, #4087, #17187, #6265, #6395, #27853, #12581 ),
 .UNSPECIFIED., .F., .F.,
 ( 4, 3, 4 ),
 ( 9.299800619644450092E-17, 0.009512539173626386249, 0.02506242213020836232 ),
 .UNSPECIFIED. ) ;
#13265 = CARTESIAN_POINT ( 'NONE',  ( 1.833206310202334155, -145.1075835704899930, 0.7447039688720614725 ) ) ;
#13266 = CARTESIAN_POINT ( 'NONE',  ( 109.1592201516379674, -0.007856029051022764623, 0.0003082430542016628347 ) ) ;
#13267 = CARTESIAN_POINT ( 'NONE',  ( 25.64681081121879203, -107.2555980796238657, -35.28660243342658731 ) ) ;
#13268 = CARTESIAN_POINT ( 'NONE',  ( -1.019300379054419947, 25.26451264419699783, 38.21680004809136477 ) ) ;
#13269 = CARTESIAN_POINT ( 'NONE',  ( 25.64703792032467433, 66.48786612795875328, 91.25955007190242441 ) ) ;
#13270 = B_SPLINE_CURVE_WITH_KNOTS ( 'NONE', 3,
 ( #16649, #21662, #27995, #23570, #18948, #1525, #1792 ),
 .UNSPECIFIED., .F., .F.,
 ( 4, 3, 4 ),
 ( 6.242136742649753700E-16, 0.02816610861753246833, 0.04000277880656282620 ),
 .UNSPECIFIED. ) ;
#13271 = CARTESIAN_POINT ( 'NONE',  ( -1.050230347699841582, 0.2550051351977194458, 45.79907861674081460 ) ) ;
#13272 = EDGE_CURVE ( 'NONE', #3393, #16069, #26261, .T. ) ;
#13273 = CARTESIAN_POINT ( 'NONE',  ( 55.79472521941426777, -54.55111121764116433, 48.13855120843864910 ) ) ;
#13274 = B_SPLINE_CURVE_WITH_KNOTS ( 'NONE', 3,
 ( #9053, #9482, #20257, #24614, #6759, #22440, #404, #13781 ),
 .UNSPECIFIED., .F., .F.,
 ( 4, 2, 2, 4 ),
 ( 0.000000000000000000, 0.0002429588503611127025, 0.0004859177007222254051, 0.0009718354014444663142 ),
 .UNSPECIFIED. ) ;
#13275 = CARTESIAN_POINT ( 'NONE',  ( 25.98552792386800192, -65.62435323276234556, 92.15963349013344441 ) ) ;
#13276 = CARTESIAN_POINT ( 'NONE',  ( -8.786685647604890903, 7.199674155858966529, -53.04920435127184675 ) ) ;
#13278 = ORIENTED_EDGE ( 'NONE', *, *, #13601, .T. ) ;
#13277 = ADVANCED_FACE ( 'NONE', ( #2439 ), #11095, .F. ) ;
#13279 = EDGE_LOOP ( 'NONE', ( #27607, #25107, #14376, #7320 ) ) ;
#13281 = CARTESIAN_POINT ( 'NONE',  ( -55.25719721206881729, 0.01041086141212315547, 0.004044147484874825726 ) ) ;
#13280 = CARTESIAN_POINT ( 'NONE',  ( 2.063896406836605024, 108.8509294491477846, -96.20114399516289438 ) ) ;
#13282 = CARTESIAN_POINT ( 'NONE',  ( -55.24271866751342941, 0.004365563123935787236, 0.008433070970613791573 ) ) ;
#13283 = CARTESIAN_POINT ( 'NONE',  ( 2.433796855181205476, 96.28145139437683042, 109.1007109081229345 ) ) ;
#13284 = CARTESIAN_POINT ( 'NONE',  ( -7.078251931573400491, 38.93060825814280435, 34.59014398252872269 ) ) ;
#13285 = CARTESIAN_POINT ( 'NONE',  ( 32.73300124599735739, -110.6325518752276622, 39.98094346392273479 ) ) ;
#13286 = ORIENTED_EDGE ( 'NONE', *, *, #14850, .T. ) ;
#13287 = CARTESIAN_POINT ( 'NONE',  ( 1.833485406944043827, 145.1085452359073145, 0.5339064996889848480 ) ) ;
#13288 = ORIENTED_EDGE ( 'NONE', *, *, #23880, .F. ) ;
#13289 = CARTESIAN_POINT ( 'NONE',  ( -1.045287976400351981, 43.05558670614237116, -15.59869763335110449 ) ) ;
#13290 = B_SPLINE_CURVE_WITH_KNOTS ( 'NONE', 3,
 ( #12950, #28068, #1457, #10398, #10670, #25657, #5797, #21745, #12531, #10813 ),
 .UNSPECIFIED., .F., .F.,
 ( 4, 3, 3, 4 ),
 ( 8.673617379884035472E-18, 0.0002669560319015772424, 0.0005492286108966412369, 0.0008315040496093445725 ),
 .UNSPECIFIED. ) ;
#13291 = DIRECTION ( 'NONE',  ( -0.7637818620346800147, -0.6451161201712181104, 0.02150485345384613861 ) ) ;
#13292 = ORIENTED_EDGE ( 'NONE', *, *, #12607, .T. ) ;
#13293 = EDGE_LOOP ( 'NONE', ( #20547, #3824, #9829, #26694 ) ) ;
#13294 = CARTESIAN_POINT ( 'NONE',  ( -1.044557008772713402, -15.70482370518787718, 43.01636061109000053 ) ) ;
#13295 = ORIENTED_EDGE ( 'NONE', *, *, #18, .F. ) ;
#13296 = CARTESIAN_POINT ( 'NONE',  ( 109.1587776205901577, -0.004240403845337402736, -0.005978137617714210199 ) ) ;
#13297 = ORIENTED_EDGE ( 'NONE', *, *, #15965, .F. ) ;
#13298 = B_SPLINE_CURVE_WITH_KNOTS ( 'NONE', 3,
 ( #28430, #24279, #24579, #24144 ),
 .UNSPECIFIED., .F., .F.,
 ( 4, 4 ),
 ( 0.0005339083821128836910, 0.001067817517169162081 ),
 .UNSPECIFIED. ) ;
#13299 = CARTESIAN_POINT ( 'NONE',  ( 1.833721034905666736, 97.36162733017710025, 107.5990973104326258 ) ) ;
#13300 =( BOUNDED_SURFACE ( )  B_SPLINE_SURFACE ( 3, 1, ( 
 ( #12278, #18755 ),
 ( #25540, #23380 ),
 ( #14437, #27385 ),
 ( #3358, #3631 ) ),
 .UNSPECIFIED., .F., .F., .F. ) 
 B_SPLINE_SURFACE_WITH_KNOTS ( ( 4, 4 ),
 ( 2, 2 ),
 ( 0.000000000000000000, 1.000000000000000000 ),
 ( 0.000000000000000000, 1.000000000000000000 ),
 .UNSPECIFIED. ) 
 GEOMETRIC_REPRESENTATION_ITEM ( )  RATIONAL_B_SPLINE_SURFACE ( (
 ( 1.000000000000000000, 1.000000000000000000),
 ( 0.6386103224230302855, 0.9954351624131538845),
 ( 0.6386103224230302855, 0.9954351624131538845),
 ( 1.000000000000000000, 1.000000000000000000) ) ) 
 REPRESENTATION_ITEM ( '' )  SURFACE ( )  );
#13301 = CARTESIAN_POINT ( 'NONE',  ( -1.045287976400365970, 1.530335034934747318, 45.76855895860941814 ) ) ;
#13302 = CARTESIAN_POINT ( 'NONE',  ( -28.13707043255157103, -7.802116958608856123, 21.52861750560947129 ) ) ;
#13303 = CARTESIAN_POINT ( 'NONE',  ( -22.23342874802668234, 2.180636882146512079, -31.55488258420089664 ) ) ;
#13304 = CARTESIAN_POINT ( 'NONE',  ( -1.239374126674604337, -25.08410696974269527, -38.61989855450929809 ) ) ;
#13305 = EDGE_CURVE ( 'NONE', #16995, #14040, #24738, .T. ) ;
#13306 = CARTESIAN_POINT ( 'NONE',  ( -24.53239521893647890, -24.99972072650158950, -22.94500969220225883 ) ) ;
#13307 = CARTESIAN_POINT ( 'NONE',  ( -1.239374126674604337, -11.92219841463861130, -44.48112152129341013 ) ) ;
#13308 = EDGE_CURVE ( 'NONE', #7877, #23571, #2361, .T. ) ;
#13309 = ORIENTED_EDGE ( 'NONE', *, *, #26437, .T. ) ;
#13310 = CARTESIAN_POINT ( 'NONE',  ( 30.59138290137891047, -70.47507990428499625, -92.40465044710811071 ) ) ;
#13311 = CARTESIAN_POINT ( 'NONE',  ( -55.24300891470648622, 0.003362556190415182372, -0.009225237711098200136 ) ) ;
#13312 = EDGE_CURVE ( 'NONE', #12584, #13547, #23722, .T. ) ;
#13313 = CARTESIAN_POINT ( 'NONE',  ( 2.263178607246682628, 1.401567185706472207, 145.3892423243864300 ) ) ;
#13314 = CARTESIAN_POINT ( 'NONE',  ( 109.1721716018069515, 0.01567407524361261531, -0.006757465437533811958 ) ) ;
#13315 = CARTESIAN_POINT ( 'NONE',  ( -55.24728320129491266, -0.008013189884950039019, 0.01214321324516758234 ) ) ;
#13316 = CARTESIAN_POINT ( 'NONE',  ( 1.831572820252008738, 58.11906524360477988, 132.9644823688597342 ) ) ;
#13317 = CARTESIAN_POINT ( 'NONE',  ( 1.831572820252009626, 138.3111855986061300, 43.90210991190668466 ) ) ;
#13318 = CARTESIAN_POINT ( 'NONE',  ( -7.733045908741333463, 45.70676731105722723, -25.81515396910878479 ) ) ;
#13319 = CARTESIAN_POINT ( 'NONE',  ( 109.1592201516379674, 0.002913740842103182058, -0.007302213399787563404 ) ) ;
#13320 = ORIENTED_EDGE ( 'NONE', *, *, #14464, .F. ) ;
#13321 = EDGE_CURVE ( 'NONE', #25057, #6789, #12681, .T. ) ;
#13322 = CARTESIAN_POINT ( 'NONE',  ( 109.1586900883932856, -0.002810909342011641554, -0.006561743627143320871 ) ) ;
#13323 = VECTOR ( 'NONE', #3539, 1000.000000000000227 ) ;
#13324 = VECTOR ( 'NONE', #27727, 1000.000000000000000 ) ;
#13325 = ORIENTED_EDGE ( 'NONE', *, *, #15862, .T. ) ;
#13326 = EDGE_CURVE ( 'NONE', #7205, #16763, #13033, .T. ) ;
#13327 =( GEOMETRIC_REPRESENTATION_CONTEXT ( 3 ) GLOBAL_UNCERTAINTY_ASSIGNED_CONTEXT ( ( #5061 ) ) GLOBAL_UNIT_ASSIGNED_CONTEXT ( ( #10377, #1284, #12500 ) ) REPRESENTATION_CONTEXT ( 'NONE', 'WORKASPACE' ) );
#13328 = CARTESIAN_POINT ( 'NONE',  ( 10.93730112725932635, 0.000000000000000000, 0.000000000000000000 ) ) ;
#13329 = ORIENTED_EDGE ( 'NONE', *, *, #17056, .T. ) ;
#13330 = FACE_OUTER_BOUND ( 'NONE', #25466, .T. ) ;
#13331 = EDGE_CURVE ( 'NONE', #19518, #7680, #17817, .T. ) ;
#13332 = FACE_OUTER_BOUND ( 'NONE', #1903, .T. ) ;
#13333 = LINE ( 'NONE', #25902, #12525 ) ;
#13334 = CARTESIAN_POINT ( 'NONE',  ( 1.894214914920954174, -138.3376769255506247, -43.94587946447545335 ) ) ;
#13335 = CARTESIAN_POINT ( 'NONE',  ( 24.01988960052067057, -94.47404045191566979, -90.81495976423880734 ) ) ;
#13336 = CARTESIAN_POINT ( 'NONE',  ( 25.64699802086724745, 110.4930320910560511, 23.24292564406076522 ) ) ;
#13337 = ADVANCED_FACE ( 'NONE', ( #5028 ), #12767, .F. ) ;
#13338 = EDGE_LOOP ( 'NONE', ( #8104, #22677, #10697, #26471 ) ) ;
#13339 = CARTESIAN_POINT ( 'NONE',  ( 1.832998868059858122, 45.34898734666050757, 137.8420662456171897 ) ) ;
#13340 =( BOUNDED_SURFACE ( )  B_SPLINE_SURFACE ( 3, 1, ( 
 ( #16404, #16969 ),
 ( #16703, #18708 ),
 ( #25191, #14666 ),
 ( #7649, #3450 ) ),
 .UNSPECIFIED., .F., .F., .F. ) 
 B_SPLINE_SURFACE_WITH_KNOTS ( ( 4, 4 ),
 ( 2, 2 ),
 ( 0.000000000000000000, 1.000000000000000000 ),
 ( 0.000000000000000000, 1.000000000000000000 ),
 .UNSPECIFIED. ) 
 GEOMETRIC_REPRESENTATION_ITEM ( )  RATIONAL_B_SPLINE_SURFACE ( (
 ( 1.000000000000000000, 1.000000000000000000),
 ( 0.9956975270656954757, 0.8568959468854893125),
 ( 0.9956975270656954757, 0.8568959468854893125),
 ( 1.000000000000000000, 1.000000000000000000) ) ) 
 REPRESENTATION_ITEM ( '' )  SURFACE ( )  );
#13341 = EDGE_CURVE ( 'NONE', #6550, #26453, #14418, .T. ) ;
#13342 = CARTESIAN_POINT ( 'NONE',  ( 109.1778270068192853, 0.008743876326162637949, -0.003210287141653713969 ) ) ;
#13343 = CARTESIAN_POINT ( 'NONE',  ( -20.20898977204109670, 0.6607022527616891461, -29.59696883073212348 ) ) ;
#13344 = ORIENTED_EDGE ( 'NONE', *, *, #21904, .F. ) ;
#13345 = VERTEX_POINT ( 'NONE', #2588 ) ;
#13346 = CARTESIAN_POINT ( 'NONE',  ( -1.050231094221210526, -27.12595454131532691, -36.90262059116457038 ) ) ;
#13347 = CARTESIAN_POINT ( 'NONE',  ( 1.893872463202012524, -43.94661640105923794, -138.3372034345896395 ) ) ;
#13348 = CARTESIAN_POINT ( 'NONE',  ( 25.64699802086724745, 75.72889180797122322, 83.75009658924024336 ) ) ;
#13349 = CIRCLE ( 'NONE', #18412, 151.1787379149930359 ) ;
#13350 = CARTESIAN_POINT ( 'NONE',  ( -28.13707043255157103, -7.802116958609158992, -21.52861750560936471 ) ) ;
#13351 = FACE_OUTER_BOUND ( 'NONE', #17968, .T. ) ;
#13352 = CARTESIAN_POINT ( 'NONE',  ( 25.69398547355838858, 46.61500694509645371, 102.8740393624595413 ) ) ;
#13353 = ORIENTED_EDGE ( 'NONE', *, *, #11971, .T. ) ;
#13354 = LINE ( 'NONE', #13088, #17833 ) ;
#13355 = CARTESIAN_POINT ( 'NONE',  ( 1.831572820252009626, 132.1614873090357207, -59.92262167723306021 ) ) ;
#13356 = DIRECTION ( 'NONE',  ( -0.7563875759206388771, 0.2351350468682910366, 0.6104009704506918599 ) ) ;
#13357 = CARTESIAN_POINT ( 'NONE',  ( 109.1778270068192853, 0.006489198140359531998, 0.006682187084648931116 ) ) ;
#13358 = CARTESIAN_POINT ( 'NONE',  ( 26.11404676487257603, -74.91683232330916553, -84.89295829319569009 ) ) ;
#13359 = FACE_OUTER_BOUND ( 'NONE', #19340, .T. ) ;
#13360 = EDGE_LOOP ( 'NONE', ( #26322, #26895, #23223, #17873 ) ) ;
#13361 = CARTESIAN_POINT ( 'NONE',  ( -18.41936578851706230, 42.05131332928132082, 5.707900577128324215 ) ) ;
#13362 = CARTESIAN_POINT ( 'NONE',  ( 1.833603222531958954, -117.1340888386543782, -85.65285110156258952 ) ) ;
#13363 = ORIENTED_EDGE ( 'NONE', *, *, #22167, .F. ) ;
#13364 = VERTEX_POINT ( 'NONE', #7504 ) ;
#13365 = VERTEX_POINT ( 'NONE', #25064 ) ;
#13366 = AXIS2_PLACEMENT_3D ( 'NONE', #23738, #9306, #6721 ) ;
#13367 = AXIS2_PLACEMENT_3D ( 'NONE', #6572, #17775, #26273 ) ;
#13368 = CARTESIAN_POINT ( 'NONE',  ( -20.57838717382308147, 10.78122205917000365, -27.96569011373090063 ) ) ;
#13369 = EDGE_CURVE ( 'NONE', #14908, #9272, #10316, .T. ) ;
#13370 = CARTESIAN_POINT ( 'NONE',  ( 10.93730112725936188, 148.8212007290658505, 26.59437931460817595 ) ) ;
#13371 = CONICAL_SURFACE ( 'NONE', #19807, 28.92774122539760384, 0.7853981625000054922 ) ;
#13372 = EDGE_CURVE ( 'NONE', #25292, #18738, #27095, .T. ) ;
#13373 = VERTEX_POINT ( 'NONE', #14528 ) ;
#13374 = CARTESIAN_POINT ( 'NONE',  ( -7.078251931573400491, -38.93060825814254144, -34.59014398252902112 ) ) ;
#13375 = CARTESIAN_POINT ( 'NONE',  ( -25.21435515916043713, -34.29329011225952684, 4.655591116594705703 ) ) ;
#13376 = VERTEX_POINT ( 'NONE', #14669 ) ;
#13377 = CARTESIAN_POINT ( 'NONE',  ( 28.37599760073041466, 105.5302221302112713, -45.02094138570479487 ) ) ;
#13378 = ORIENTED_EDGE ( 'NONE', *, *, #20466, .F. ) ;
#13379 = CARTESIAN_POINT ( 'NONE',  ( -55.24728320129491266, 0.005114031043468944375, -0.01362040845703405695 ) ) ;
#13380 = CARTESIAN_POINT ( 'NONE',  ( 32.73300124599734318, 113.0038235389602477, 32.68291970228275289 ) ) ;
#13381 = CARTESIAN_POINT ( 'NONE',  ( -4.178947244162636743, -3.367451375481460563, -48.81675275154075422 ) ) ;
#13382 = B_SPLINE_CURVE_WITH_KNOTS ( 'NONE', 3,
 ( #17517, #15068, #2109, #4141, #21426, #23466 ),
 .UNSPECIFIED., .F., .F.,
 ( 4, 2, 4 ),
 ( 4.055692965608002806E-16, 0.003576372551511211671, 0.007152745103022018283 ),
 .UNSPECIFIED. ) ;
#13383 = CARTESIAN_POINT ( 'NONE',  ( -15.02187109954783040, -20.12219089991063825, 41.75590530176331328 ) ) ;
#13384 = CARTESIAN_POINT ( 'NONE',  ( 2.430230287190589422, -144.8619874886005903, -13.76600171652792248 ) ) ;
#13385 = CARTESIAN_POINT ( 'NONE',  ( 1.831572820252009626, -45.77972211429720062, -137.7011124121622174 ) ) ;
#13386 = CARTESIAN_POINT ( 'NONE',  ( -28.41354790283022069, -12.60397206714846341, -19.47297445639544833 ) ) ;
#13387 = CARTESIAN_POINT ( 'NONE',  ( 94.22246935314088034, -151.1871800109700246, -6.938893903907228378E-15 ) ) ;
#13388 = COLOUR_RGB ( '',0.7921568627450980005, 0.8196078431372548767, 0.9333333333333333481 ) ;
#13389 = FACE_OUTER_BOUND ( 'NONE', #4390, .T. ) ;
#13390 = DIRECTION ( 'NONE',  ( 1.000000000000000000, -6.938893903907226837E-18, 1.734723475976806709E-18 ) ) ;
#13391 = CARTESIAN_POINT ( 'NONE',  ( 1.833485406944057594, -44.33323125130021225, 138.1714136985306993 ) ) ;
#13392 = CARTESIAN_POINT ( 'NONE',  ( 109.1624594426973118, 0.005372302061316064012, 0.01503296564241279366 ) ) ;
#13393 = EDGE_LOOP ( 'NONE', ( #10802, #2673, #21318, #20348 ) ) ;
#13394 = AXIS2_PLACEMENT_3D ( 'NONE', #14106, #16427, #15987 ) ;
#13395 = ORIENTED_EDGE ( 'NONE', *, *, #18214, .T. ) ;
#13396 = CARTESIAN_POINT ( 'NONE',  ( 25.64660436782547137, 24.04259444204660667, 110.3216080362391125 ) ) ;
#13397 = CARTESIAN_POINT ( 'NONE',  ( -55.24300891470648622, 0.0003472257464250210184, -0.009812809446890590967 ) ) ;
#13398 = ORIENTED_EDGE ( 'NONE', *, *, #3939, .F. ) ;
#13399 = B_SPLINE_CURVE_WITH_KNOTS ( 'NONE', 3,
 ( #14443, #10296, #19054, #16170, #24972, #5232 ),
 .UNSPECIFIED., .F., .F.,
 ( 4, 2, 4 ),
 ( 4.906538933386797396E-18, 0.0004335151646191543395, 0.0008670303292383036917 ),
 .UNSPECIFIED. ) ;
#13400 = EDGE_LOOP ( 'NONE', ( #10946, #1040, #7426, #11059 ) ) ;
#13401 = ORIENTED_EDGE ( 'NONE', *, *, #7834, .T. ) ;
#13402 = CARTESIAN_POINT ( 'NONE',  ( -20.20612092514784308, -1.137292630518264680, -29.57813644637189299 ) ) ;
#13403 = CARTESIAN_POINT ( 'NONE',  ( -20.20700224038492721, 29.58392382092673500, -0.9908225410479557516 ) ) ;
#13404 = EDGE_CURVE ( 'NONE', #16492, #27099, #16462, .T. ) ;
#13405 = EDGE_CURVE ( 'NONE', #20253, #16608, #1358, .T. ) ;
#13406 = B_SPLINE_CURVE_WITH_KNOTS ( 'NONE', 3,
 ( #17006, #1327, #3348, #12272 ),
 .UNSPECIFIED., .F., .F.,
 ( 4, 4 ),
 ( 3.805030037801212946E-16, 0.01077107486149793923 ),
 .UNSPECIFIED. ) ;
#13407 = ORIENTED_EDGE ( 'NONE', *, *, #8382, .F. ) ;
#13408 = EDGE_CURVE ( 'NONE', #27092, #12372, #19925, .T. ) ;
#13409 = CARTESIAN_POINT ( 'NONE',  ( 2.063896406836605024, 125.1295119249439125, 73.79559738457795959 ) ) ;
#13410 = CARTESIAN_POINT ( 'NONE',  ( -20.21097721712958872, 29.61001327235739566, 0.3305963429843793433 ) ) ;
#13411 = VECTOR ( 'NONE', #14430, 1000.000000000000227 ) ;
#13412 = EDGE_CURVE ( 'NONE', #12630, #13718, #8931, .T. ) ;
#13413 = VECTOR ( 'NONE', #7400, 1000.000000000000114 ) ;
#13414 = CARTESIAN_POINT ( 'NONE',  ( -55.24300891470650754, -0.003362556190412219030, -0.009225237711101438864 ) ) ;
#13415 = CARTESIAN_POINT ( 'NONE',  ( -25.21435515916025594, 1.749597353048488237E-16, -4.373993382621220594E-17 ) ) ;
#13416 = CARTESIAN_POINT ( 'NONE',  ( -1.049819078601898381, 0.5100232645225435402, 45.79653735114490587 ) ) ;
#13417 = CARTESIAN_POINT ( 'NONE',  ( 25.64699802086726521, -110.3941571196682077, 23.70809581152572676 ) ) ;
#13418 = CARTESIAN_POINT ( 'NONE',  ( -4.178947244162633190, -45.38689110596704523, 18.28784278438497068 ) ) ;
#13419 = CARTESIAN_POINT ( 'NONE',  ( -15.02187109954787303, 21.95370994985631086, 40.82269973458213030 ) ) ;
#13420 = CARTESIAN_POINT ( 'NONE',  ( -25.21435515916025594, 1.749597353048488237E-16, -4.373993382621220594E-17 ) ) ;
#13421 = EDGE_LOOP ( 'NONE', ( #1522, #12227, #2334, #22721 ) ) ;
#13423 = CARTESIAN_POINT ( 'NONE',  ( -7.711401346138398338, -51.42722225669428582, -10.36923727626100522 ) ) ;
#13422 = LINE ( 'NONE', #17745, #24027 ) ;
#13424 = CARTESIAN_POINT ( 'NONE',  ( -1.113548883309550375, 35.91246368318242332, 28.52482525634906096 ) ) ;
#13425 = CARTESIAN_POINT ( 'NONE',  ( 25.64681081121879203, 46.30456157731328659, 102.9795863647030103 ) ) ;
#13426 = CARTESIAN_POINT ( 'NONE',  ( 25.73574536432414206, 0.8061344836384856105, -112.9674920590232858 ) ) ;
#13427 = CARTESIAN_POINT ( 'NONE',  ( 10.93730112726006354, 150.7858122213665126, -10.89264110824830034 ) ) ;
#13428 = ORIENTED_EDGE ( 'NONE', *, *, #13176, .T. ) ;
#13429 = CARTESIAN_POINT ( 'NONE',  ( -7.733045908741331687, -5.980865481987790666, 52.15131830128831325 ) ) ;
#13430 = ORIENTED_EDGE ( 'NONE', *, *, #23080, .T. ) ;
#13431 = CARTESIAN_POINT ( 'NONE',  ( -1.050231094221206973, 43.47885872350356351, -14.39477892760314326 ) ) ;
#13433 = AXIS2_PLACEMENT_3D ( 'NONE', #6990, #15740, #14251 ) ;
#13432 = FACE_OUTER_BOUND ( 'NONE', #1038, .T. ) ;
#13434 = EDGE_LOOP ( 'NONE', ( #3370, #3636, #23920, #9912 ) ) ;
#13435 = EDGE_LOOP ( 'NONE', ( #27774, #11576, #16644, #13149 ) ) ;
#13436 = CARTESIAN_POINT ( 'NONE',  ( -28.13707043255157103, 6.342158660427315020, 22.00298671236732773 ) ) ;
#13438 =( BOUNDED_SURFACE ( )  B_SPLINE_SURFACE ( 3, 1, ( 
 ( #13113, #21899 ),
 ( #17562, #11101 ),
 ( #8952, #19871 ),
 ( #26352, #161 ) ),
 .UNSPECIFIED., .F., .F., .F. ) 
 B_SPLINE_SURFACE_WITH_KNOTS ( ( 4, 4 ),
 ( 2, 2 ),
 ( 0.000000000000000000, 1.000000000000000000 ),
 ( 0.000000000000000000, 1.000000000000000000 ),
 .UNSPECIFIED. ) 
 GEOMETRIC_REPRESENTATION_ITEM ( )  RATIONAL_B_SPLINE_SURFACE ( (
 ( 1.000000000000000000, 1.000000000000000000),
 ( 0.9593753223639863714, 0.9995975284513187731),
 ( 0.9593753223639863714, 0.9995975284513187731),
 ( 1.000000000000000000, 1.000000000000000000) ) ) 
 REPRESENTATION_ITEM ( '' )  SURFACE ( )  );
#13437 = VECTOR ( 'NONE', #22360, 1000.000000000000114 ) ;
#13439 = ORIENTED_EDGE ( 'NONE', *, *, #20477, .T. ) ;
#13440 = CARTESIAN_POINT ( 'NONE',  ( 1.833838848569403046, -97.22964245509687942, -107.7184832843406497 ) ) ;
#13441 = VECTOR ( 'NONE', #4151, 1000.000000000000000 ) ;
#13442 = EDGE_LOOP ( 'NONE', ( #25817, #17182, #3760, #4890 ) ) ;
#13443 = EDGE_CURVE ( 'NONE', #7969, #11307, #339, .T. ) ;
#13444 = B_SPLINE_CURVE_WITH_KNOTS ( 'NONE', 3,
 ( #622, #9412, #18164, #26942, #13138, #24819 ),
 .UNSPECIFIED., .F., .F.,
 ( 4, 2, 4 ),
 ( 0.000000000000000000, 0.0006311571484586015607, 0.001262314296917203121 ),
 .UNSPECIFIED. ) ;
#13445 = B_SPLINE_CURVE_WITH_KNOTS ( 'NONE', 3,
 ( #21508, #14746, #16918, #10447, #17189, #1645, #19347, #17044 ),
 .UNSPECIFIED., .F., .F.,
 ( 4, 2, 2, 4 ),
 ( 3.469446951953614189E-18, 0.0002429588503611212677, 0.0004859177007222390660, 0.0009718354014444785657 ),
 .UNSPECIFIED. ) ;
#13446 = DIRECTION ( 'NONE',  ( -0.7071067818211355105, 9.150583771627656306E-17, -0.7071067805519596350 ) ) ;
#13447 = B_SPLINE_CURVE_WITH_KNOTS ( 'NONE', 3,
 ( #26918, #17263, #21450, #5789, #14962, #21310 ),
 .UNSPECIFIED., .F., .F.,
 ( 4, 2, 4 ),
 ( 0.000000000000000000, 0.0004335151646191513579, 0.0008670303292383027159 ),
 .UNSPECIFIED. ) ;
#13448 = EDGE_CURVE ( 'NONE', #24062, #6049, #7559, .T. ) ;
#13449 = CARTESIAN_POINT ( 'NONE',  ( -12.94347594948481373, -23.08810053288719999, -42.93165645342850212 ) ) ;
#13450 = CARTESIAN_POINT ( 'NONE',  ( 25.64681081121879203, 110.5293738517608375, 23.06870491922360245 ) ) ;
#13451 = CARTESIAN_POINT ( 'NONE',  ( -1.058473599757826511, -38.06357893967446415, -25.48501014712384816 ) ) ;
#13452 = CARTESIAN_POINT ( 'NONE',  ( 24.01988960052044320, 108.4726924928710190, -73.52806416353990926 ) ) ;
#13453 = FACE_OUTER_BOUND ( 'NONE', #8914, .T. ) ;
#13454 = FACE_OUTER_BOUND ( 'NONE', #22705, .T. ) ;
#13455 = B_SPLINE_CURVE_WITH_KNOTS ( 'NONE', 3,
 ( #24101, #2050, #17594, #26100, #10991, #4218, #2479 ),
 .UNSPECIFIED., .F., .F.,
 ( 4, 3, 4 ),
 ( 0.000000000000000000, 0.006568092053401780595, 0.02506242213020846640 ),
 .UNSPECIFIED. ) ;
#13456 = VECTOR ( 'NONE', #14191, 999.9999999999998863 ) ;
#13457 = CARTESIAN_POINT ( 'NONE',  ( 10.93730112725939030, 140.0398180619108075, 56.95489579269806057 ) ) ;
#13458 = CARTESIAN_POINT ( 'NONE',  ( -1.046935749539993799, 27.93995161054695231, -36.28605774377773230 ) ) ;
#13459 = CARTESIAN_POINT ( 'NONE',  ( -8.786685647604890903, 25.35688121747502066, -47.14957014837363403 ) ) ;
#13460 = CIRCLE ( 'NONE', #23138, 117.6351876552689504 ) ;
#13461 = CARTESIAN_POINT ( 'NONE',  ( 1.832998868059890096, -145.1092030902949830, 0.5339089137742853985 ) ) ;
#13462 = CARTESIAN_POINT ( 'NONE',  ( -5.986830583229478364, 19.95149887249920440, 46.64941882410778362 ) ) ;
#13463 = DIRECTION ( 'NONE',  ( -0.5914120900931443270, 0.8027508043202534749, 0.07630783613001089483 ) ) ;
#13464 = CARTESIAN_POINT ( 'NONE',  ( -20.20700224038492721, 10.08426345511588984, -27.82980252387822517 ) ) ;
#13465 = ORIENTED_EDGE ( 'NONE', *, *, #23582, .T. ) ;
#13466 = CARTESIAN_POINT ( 'NONE',  ( 1.833838848569417257, -44.67212175381932582, 138.0625820091623837 ) ) ;
#13467 = CARTESIAN_POINT ( 'NONE',  ( -23.79223135445719350, 16.82181692922858929, 28.60983116549946814 ) ) ;
#13468 = CARTESIAN_POINT ( 'NONE',  ( 21.16825799904930605, 83.13600836828977947, 106.9139171613925470 ) ) ;
#13469 = CARTESIAN_POINT ( 'NONE',  ( 25.64699802086724389, 110.3941571196683924, -23.70809581152500911 ) ) ;
#13470 = EDGE_LOOP ( 'NONE', ( #13122, #8293, #14196, #3138 ) ) ;
#13471 = CARTESIAN_POINT ( 'NONE',  ( 109.1586059443104944, 0.006570129623060872066, -0.002622205828288707002 ) ) ;
#13472 = AXIS2_PLACEMENT_3D ( 'NONE', #21167, #25784, #6077 ) ;
#13473 =( BOUNDED_SURFACE ( )  B_SPLINE_SURFACE ( 3, 1, ( 
 ( #21097, #18806 ),
 ( #21250, #5866 ),
 ( #3690, #19098 ),
 ( #27295, #27871 ) ),
 .UNSPECIFIED., .F., .F., .F. ) 
 B_SPLINE_SURFACE_WITH_KNOTS ( ( 4, 4 ),
 ( 2, 2 ),
 ( 0.000000000000000000, 1.000000000000000000 ),
 ( 0.000000000000000000, 1.000000000000000000 ),
 .UNSPECIFIED. ) 
 GEOMETRIC_REPRESENTATION_ITEM ( )  RATIONAL_B_SPLINE_SURFACE ( (
 ( 1.000000000000000000, 1.000000000000000000),
 ( 0.7789835883360576307, 0.9689951854195403280),
 ( 0.7789835883360576307, 0.9689951854195403280),
 ( 1.000000000000000000, 1.000000000000000000) ) ) 
 REPRESENTATION_ITEM ( '' )  SURFACE ( )  );
#13475 = CARTESIAN_POINT ( 'NONE',  ( 109.1592201516379674, 0.006957642258146918765, -0.003661068210037320397 ) ) ;
#13474 = B_SPLINE_CURVE_WITH_KNOTS ( 'NONE', 3,
 ( #16218, #26999, #22725, #2690, #5138, #9171, #7175 ),
 .UNSPECIFIED., .F., .F.,
 ( 4, 3, 4 ),
 ( 6.702613243490674079E-16, 0.02816610861753246139, 0.04000277880656292334 ),
 .UNSPECIFIED. ) ;
#13476 = CARTESIAN_POINT ( 'NONE',  ( -1.619063947482197729, 46.30105812165548684, 2.489035965910320503 ) ) ;
#13477 = ADVANCED_FACE ( 'NONE', ( #27626 ), #24733, .F. ) ;
#13478 = PRODUCT_DEFINITION_FORMATION_WITH_SPECIFIED_SOURCE ( 'ANY', '', #2083, .NOT_KNOWN. ) ;
#13479 = ORIENTED_EDGE ( 'NONE', *, *, #19499, .F. ) ;
#13480 = CARTESIAN_POINT ( 'NONE',  ( 26.04756280548353686, 112.4366864265129493, -12.93458011762360549 ) ) ;
#13481 = VECTOR ( 'NONE', #24690, 1000.000000000000114 ) ;
#13482 = EDGE_CURVE ( 'NONE', #28480, #4329, #15752, .T. ) ;
#13483 = CARTESIAN_POINT ( 'NONE',  ( -25.21435515916043713, -30.48034229288650820, -16.39063784838731053 ) ) ;
#13484 = DIRECTION ( 'NONE',  ( 0.000000000000000000, 0.000000000000000000, 1.000000000000000000 ) ) ;
#13485 = VERTEX_POINT ( 'NONE', #9951 ) ;
#13486 = ADVANCED_FACE ( 'NONE', ( #16550 ), #2073, .F. ) ;
#13487 = CARTESIAN_POINT ( 'NONE',  ( 24.22246935314087324, 0.000000000000000000, 0.000000000000000000 ) ) ;
#13488 = CARTESIAN_POINT ( 'NONE',  ( 19.66333377628696510, -121.4767361208140812, 64.94841092372145397 ) ) ;
#13489 = LINE ( 'NONE', #22283, #6100 ) ;
#13490 = CARTESIAN_POINT ( 'NONE',  ( -55.24300891470648622, 0.009439835024157980023, -0.002702093572889658051 ) ) ;
#13491 = CARTESIAN_POINT ( 'NONE',  ( 109.1586059443104944, 0.002447596125905588706, -0.006637156007973989483 ) ) ;
#13492 = VERTEX_POINT ( 'NONE', #6462 ) ;
#13493 = CARTESIAN_POINT ( 'NONE',  ( 26.11404676487257603, 57.58742681967449784, 97.48350837663630841 ) ) ;
#13494 = CARTESIAN_POINT ( 'NONE',  ( 10.93730112725990011, -150.7858122213662000, -10.89264110825150489 ) ) ;
#13495 = ORIENTED_EDGE ( 'NONE', *, *, #5176, .T. ) ;
#13496 = VERTEX_POINT ( 'NONE', #15214 ) ;
#13497 = ORIENTED_EDGE ( 'NONE', *, *, #23327, .F. ) ;
#13498 = CARTESIAN_POINT ( 'NONE',  ( 32.73300124599732186, 0.000000000000000000, 0.000000000000000000 ) ) ;
#13499 = CARTESIAN_POINT ( 'NONE',  ( 25.64681081121879203, 102.9795863647028682, 46.30456157731362765 ) ) ;
#13500 = CARTESIAN_POINT ( 'NONE',  ( -7.078251931573406708, -20.86696228105259365, -47.71415099571797924 ) ) ;
#13501 = CARTESIAN_POINT ( 'NONE',  ( -1.031422197589716205, 37.93675465142474224, -25.67058493451456513 ) ) ;
#13502 = CARTESIAN_POINT ( 'NONE',  ( -22.34422965417106965, 37.57019010019570260, -5.100074259622762618 ) ) ;
#13503 = CARTESIAN_POINT ( 'NONE',  ( -20.20700224038492365, -8.199606986804534259, -28.44216453106533748 ) ) ;
#13504 = LINE ( 'NONE', #9056, #21756 ) ;
#13505 = ORIENTED_EDGE ( 'NONE', *, *, #11302, .T. ) ;
#13506 = CARTESIAN_POINT ( 'NONE',  ( 2.433796855181233454, 31.67151202412969724, 142.0211193075556935 ) ) ;
#13507 = CARTESIAN_POINT ( 'NONE',  ( 6.505213034913034000E-17, 4.541450660883840889E-15, -37.50000000000001421 ) ) ;
#13508 = CARTESIAN_POINT ( 'NONE',  ( 109.1586900883932856, -0.007002774699553647453, -0.001385221016527435301 ) ) ;
#13509 = CARTESIAN_POINT ( 'NONE',  ( 109.1721716018069657, 0.003746085893652563534, 0.01665253177026231046 ) ) ;
#13510 = PRODUCT_RELATED_PRODUCT_CATEGORY ( 'part', '', ( #2083 ) ) ;
#13511 = CARTESIAN_POINT ( 'NONE',  ( 109.1721716018069657, 0.01488186354166047033, 0.008358834333183975951 ) ) ;
#13512 = ORIENTED_EDGE ( 'NONE', *, *, #9897, .T. ) ;
#13513 = CARTESIAN_POINT ( 'NONE',  ( 1.832998868059890096, 72.09222286251085166, 125.9352106559986026 ) ) ;
#13514 = EDGE_CURVE ( 'NONE', #18375, #1898, #4788, .T. ) ;
#13515 = ORIENTED_EDGE ( 'NONE', *, *, #7165, .F. ) ;
#13516 = CARTESIAN_POINT ( 'NONE',  ( 109.1586900883932856, -0.003481399864227418834, -0.006231977675082094915 ) ) ;
#13517 = B_SPLINE_CURVE_WITH_KNOTS ( 'NONE', 3,
 ( #8543, #19479, #26098, #21496 ),
 .UNSPECIFIED., .F., .F.,
 ( 4, 4 ),
 ( 3.213376974838984927E-16, 0.01077107486149750729 ),
 .UNSPECIFIED. ) ;
#13518 = CARTESIAN_POINT ( 'NONE',  ( -2.911734481061402757, -12.03743348210748998, 46.11606034418773703 ) ) ;
#13519 = EDGE_LOOP ( 'NONE', ( #22228, #24620, #8822, #15701 ) ) ;
#13520 = EDGE_CURVE ( 'NONE', #7273, #3933, #21212, .T. ) ;
#13521 = ORIENTED_EDGE ( 'NONE', *, *, #2627, .F. ) ;
#13522 = EDGE_LOOP ( 'NONE', ( #25163, #7318, #22994, #9362 ) ) ;
#13523 = DIRECTION ( 'NONE',  ( -0.5914120900931443270, 0.5938529060132731185, -0.5455001977187993178 ) ) ;
#13524 =( BOUNDED_SURFACE ( )  B_SPLINE_SURFACE ( 3, 1, ( 
 ( #24231, #28374 ),
 ( #21781, #4635 ),
 ( #181, #4488 ),
 ( #4210, #11266 ) ),
 .UNSPECIFIED., .F., .F., .F. ) 
 B_SPLINE_SURFACE_WITH_KNOTS ( ( 4, 4 ),
 ( 2, 2 ),
 ( 0.000000000000000000, 1.000000000000000000 ),
 ( 0.000000000000000000, 1.000000000000000000 ),
 .UNSPECIFIED. ) 
 GEOMETRIC_REPRESENTATION_ITEM ( )  RATIONAL_B_SPLINE_SURFACE ( (
 ( 1.000000000000000000, 1.000000000000000000),
 ( 0.9956975270656954757, 0.8568959468854893125),
 ( 0.9956975270656954757, 0.8568959468854893125),
 ( 1.000000000000000000, 1.000000000000000000) ) ) 
 REPRESENTATION_ITEM ( '' )  SURFACE ( )  );
#13525 = CARTESIAN_POINT ( 'NONE',  ( 25.64681081121879203, -23.06870491922242650, -110.5293738517610933 ) ) ;
#13526 = CARTESIAN_POINT ( 'NONE',  ( -20.57838717382308147, -18.89542499756482741, 23.26537097894125594 ) ) ;
#13527 = ORIENTED_EDGE ( 'NONE', *, *, #19555, .T. ) ;
#13528 = CARTESIAN_POINT ( 'NONE',  ( 1.833485406944043827, 141.8265699653867387, 30.69200235378984232 ) ) ;
#13529 = CARTESIAN_POINT ( 'NONE',  ( 1.833206308920067862, -142.0914675761164858, 29.44113170198502161 ) ) ;
#13530 = ORIENTED_EDGE ( 'NONE', *, *, #21056, .F. ) ;
#13531 = ORIENTED_EDGE ( 'NONE', *, *, #9562, .T. ) ;
#13532 = CARTESIAN_POINT ( 'NONE',  ( -25.21435515916043713, -30.48034229288627017, 16.39063784838775462 ) ) ;
#13533 = CARTESIAN_POINT ( 'NONE',  ( 25.64692872815577473, -45.63107645358261522, -103.2799065540888677 ) ) ;
#13534 = CARTESIAN_POINT ( 'NONE',  ( 2.433796855181205476, 96.28145139437683042, 109.1007109081229345 ) ) ;
#13535 = CARTESIAN_POINT ( 'NONE',  ( 2.430230287190572103, 1.451610819319782308, -145.5073573687466535 ) ) ;
#13536 = DIRECTION ( 'NONE',  ( 1.000000000000000000, -6.938893903907226837E-18, 1.734723475976806709E-18 ) ) ;
#13537 = CARTESIAN_POINT ( 'NONE',  ( -19.53423201713129842, 1.355459634611817431E-16, -3.388649086529543578E-17 ) ) ;
#13538 = CARTESIAN_POINT ( 'NONE',  ( -20.47566338032516597, 18.81547714195514232, 23.19796701701855213 ) ) ;
#13539 = DIRECTION ( 'NONE',  ( 0.000000000000000000, 5.223019709707975211E-21, -1.000000000000000000 ) ) ;
#13540 = CARTESIAN_POINT ( 'NONE',  ( -20.90916690077964546, -35.64494649500671386, 17.17795951644694341 ) ) ;
#13541 = CARTESIAN_POINT ( 'NONE',  ( 109.1592201516379674, -0.007748443302134891582, -0.001331853079201365982 ) ) ;
#13542 = CARTESIAN_POINT ( 'NONE',  ( -20.90916690077966322, -5.322316104228261402, -39.20864005633521998 ) ) ;
#13543 = CARTESIAN_POINT ( 'NONE',  ( -1.323439229708135434, 38.58845475799802927, 25.17120723334049970 ) ) ;
#13544 = EDGE_CURVE ( 'NONE', #25020, #3000, #5497, .T. ) ;
#13545 = ORIENTED_EDGE ( 'NONE', *, *, #19740, .F. ) ;
#13546 = EDGE_CURVE ( 'NONE', #1788, #18960, #4077, .T. ) ;
#13547 = VERTEX_POINT ( 'NONE', #8615 ) ;
#13548 = CARTESIAN_POINT ( 'NONE',  ( 28.37599760073042177, -22.09615888373874526, -112.5845136272808134 ) ) ;
#13549 = CARTESIAN_POINT ( 'NONE',  ( -9.156249394959713683, -25.18996226954579498, 48.32878616081037393 ) ) ;
#13550 = ORIENTED_EDGE ( 'NONE', *, *, #19225, .F. ) ;
#13551 = ADVANCED_FACE ( 'NONE', ( #19680 ), #10932, .F. ) ;
#13552 = EDGE_LOOP ( 'NONE', ( #17331, #582, #26056, #5580 ) ) ;
#13553 = VERTEX_POINT ( 'NONE', #114 ) ;
#13554 = CARTESIAN_POINT ( 'NONE',  ( -1.048994561756786625, 37.49601524795411223, -26.29622118251694829 ) ) ;
#13555 = CARTESIAN_POINT ( 'NONE',  ( 1.832998868059858122, -108.1944082009163850, 96.70023740551087599 ) ) ;
#13556 =( BOUNDED_SURFACE ( )  B_SPLINE_SURFACE ( 3, 1, ( 
 ( #23669, #8252 ),
 ( #1330, #25805 ),
 ( #27952, #1748 ),
 ( #16751, #1476 ) ),
 .UNSPECIFIED., .F., .F., .F. ) 
 B_SPLINE_SURFACE_WITH_KNOTS ( ( 4, 4 ),
 ( 2, 2 ),
 ( 0.000000000000000000, 1.000000000000000000 ),
 ( 0.000000000000000000, 1.000000000000000000 ),
 .UNSPECIFIED. ) 
 GEOMETRIC_REPRESENTATION_ITEM ( )  RATIONAL_B_SPLINE_SURFACE ( (
 ( 1.000000000000000000, 1.000000000000000000),
 ( 0.6386103224230316178, 0.9954351624131538845),
 ( 0.6386103224230316178, 0.9954351624131538845),
 ( 1.000000000000000000, 1.000000000000000000) ) ) 
 REPRESENTATION_ITEM ( '' )  SURFACE ( )  );
#13557 = CARTESIAN_POINT ( 'NONE',  ( -20.24419206586952313, -18.44224248888889051, -23.20105925399719382 ) ) ;
#13558 = CARTESIAN_POINT ( 'NONE',  ( 32.73300124599738581, 3.836798148480494497, -117.5726003567928757 ) ) ;
#13559 = DIRECTION ( 'NONE',  ( 0.000000000000000000, 0.000000000000000000, 1.000000000000000000 ) ) ;
#13560 = LINE ( 'NONE', #17737, #13437 ) ;
#13561 = CARTESIAN_POINT ( 'NONE',  ( -23.79223135445719706, 32.40779366744838796, -7.157574570129257907 ) ) ;
#13562 = CARTESIAN_POINT ( 'NONE',  ( 109.1587776205901577, 0.004240403845337359368, 0.005978137617714240556 ) ) ;
#13563 = CARTESIAN_POINT ( 'NONE',  ( 5.340103556456499589, -144.6887562347051244, 28.39990973640018979 ) ) ;
#13564 = CARTESIAN_POINT ( 'NONE',  ( -21.81686047589427702, 18.24499610240089353, 33.92779429964183890 ) ) ;
#13565 = CARTESIAN_POINT ( 'NONE',  ( -55.24271866751342941, -0.008488649505342596782, -0.004256484107795601053 ) ) ;
#13566 = EDGE_CURVE ( 'NONE', #25151, #17323, #28044, .T. ) ;
#13567 = VERTEX_POINT ( 'NONE', #26443 ) ;
#13569 = CARTESIAN_POINT ( 'NONE',  ( 32.73300124599737160, -116.5274707358854158, -16.10546300444944023 ) ) ;
#13568 = CARTESIAN_POINT ( 'NONE',  ( 1.833485406944043827, -142.0485807715647297, 29.64752363041495542 ) ) ;
#13570 = CARTESIAN_POINT ( 'NONE',  ( 25.64681081121879203, -23.06870491922242650, -110.5293738517610933 ) ) ;
#13571 = DIRECTION ( 'NONE',  ( 0.000000000000000000, -5.223019709708190374E-21, 1.000000000000000000 ) ) ;
#13572 = LINE ( 'NONE', #6514, #15215 ) ;
#13573 = CARTESIAN_POINT ( 'NONE',  ( 109.1589550718174877, -0.006669585340466669190, 0.003591809816104974025 ) ) ;
#13574 = CARTESIAN_POINT ( 'NONE',  ( -5.986830583229486358, -33.39046620690942291, -38.20088153919488860 ) ) ;
#13575 = ORIENTED_EDGE ( 'NONE', *, *, #25842, .F. ) ;
#13576 = CARTESIAN_POINT ( 'NONE',  ( 1.833485406944057594, -15.69895494453287021, -144.2578170162064737 ) ) ;
#13577 = EDGE_CURVE ( 'NONE', #17689, #4874, #8263, .T. ) ;
#13578 = ORIENTED_EDGE ( 'NONE', *, *, #6249, .T. ) ;
#13579 = CARTESIAN_POINT ( 'NONE',  ( -20.38016308990358993, -29.73560196176845238, 1.509191766064522655 ) ) ;
#13580 = CARTESIAN_POINT ( 'NONE',  ( 25.98552792386802324, 12.89843290883527693, 112.3992180166319486 ) ) ;
#13581 = ORIENTED_EDGE ( 'NONE', *, *, #8768, .F. ) ;
#13582 = LINE ( 'NONE', #27363, #20799 ) ;
#13583 = EDGE_CURVE ( 'NONE', #8797, #13496, #1725, .T. ) ;
#13584 = ORIENTED_EDGE ( 'NONE', *, *, #3071, .F. ) ;
#13585 = CARTESIAN_POINT ( 'NONE',  ( 109.1586900883932856, 0.005715190711488718836, 0.004277182003220973000 ) ) ;
#13586 = EDGE_LOOP ( 'NONE', ( #14949, #19576, #14496, #11254 ) ) ;
#13587 = CARTESIAN_POINT ( 'NONE',  ( -21.41430102051752016, 16.60879216503635547, -25.94791611261620545 ) ) ;
#13588 = DIRECTION ( 'NONE',  ( -0.5946245182733608248, 0.3994439555666327024, -0.6977579871484492768 ) ) ;
#13589 = CARTESIAN_POINT ( 'NONE',  ( -1.046936909428682894, -15.35929614323696413, -43.14407378092988665 ) ) ;
#13590 = DIRECTION ( 'NONE',  ( 0.000000000000000000, 5.223019709707975211E-21, -1.000000000000000000 ) ) ;
#13591 = CARTESIAN_POINT ( 'NONE',  ( 109.1586059443104944, 0.005067816690886755952, -0.004935564877224700789 ) ) ;
#13592 = CARTESIAN_POINT ( 'NONE',  ( 10.93730112725972425, -65.95960219663204782, 136.0306644680981094 ) ) ;
#13593 = DIRECTION ( 'NONE',  ( 0.000000000000000000, 0.000000000000000000, 1.000000000000000000 ) ) ;
#13594 = CARTESIAN_POINT ( 'NONE',  ( -8.786685647604890903, 52.67761315067286176, -9.545808661480789326 ) ) ;
#13595 = CARTESIAN_POINT ( 'NONE',  ( -1.048171036023513913, 27.73816396939564299, -36.44209502233717046 ) ) ;
#13596 = CARTESIAN_POINT ( 'NONE',  ( 1.832998868059890096, -96.70023740551050651, -108.1944082009167118 ) ) ;
#13597 = EDGE_CURVE ( 'NONE', #6393, #18715, #6876, .T. ) ;
#13598 = ORIENTED_EDGE ( 'NONE', *, *, #16415, .T. ) ;
#13599 = CARTESIAN_POINT ( 'NONE',  ( -25.21435515916043357, 16.39063784838743132, -30.48034229288645136 ) ) ;
#13600 = CARTESIAN_POINT ( 'NONE',  ( 32.73300124599735739, -32.68291970228314369, 113.0038235389601340 ) ) ;
#13601 = EDGE_CURVE ( 'NONE', #12529, #21665, #16074, .T. ) ;
#13603 = CARTESIAN_POINT ( 'NONE',  ( -7.711401346138175406, -45.70592430511711513, -25.75361633141480766 ) ) ;
#13602 = CARTESIAN_POINT ( 'NONE',  ( 1.833485406944057594, -30.69200235378832176, -141.8265699653870513 ) ) ;
#13604 = CARTESIAN_POINT ( 'NONE',  ( 21.16825799904896854, -130.1008673867302150, -37.62905626541836313 ) ) ;
#13605 = B_SPLINE_CURVE_WITH_KNOTS ( 'NONE', 3,
 ( #25744, #1556, #7635, #18836, #3296, #14793, #23602, #27603 ),
 .UNSPECIFIED., .F., .F.,
 ( 4, 2, 2, 4 ),
 ( 0.000000000000000000, 0.0002429588503611224061, 0.0004859177007222448123, 0.0009718354014444896246 ),
 .UNSPECIFIED. ) ;
#13606 = CARTESIAN_POINT ( 'NONE',  ( -20.21097721650787449, -28.05863614620931656, 9.464413208035370673 ) ) ;
#13607 =( BOUNDED_SURFACE ( )  B_SPLINE_SURFACE ( 3, 1, ( 
 ( #23396, #1077 ),
 ( #3650, #19066 ),
 ( #28107, #25961 ),
 ( #19612, #10308 ) ),
 .UNSPECIFIED., .F., .F., .F. ) 
 B_SPLINE_SURFACE_WITH_KNOTS ( ( 4, 4 ),
 ( 2, 2 ),
 ( 0.000000000000000000, 1.000000000000000000 ),
 ( 0.000000000000000000, 1.000000000000000000 ),
 .UNSPECIFIED. ) 
 GEOMETRIC_REPRESENTATION_ITEM ( )  RATIONAL_B_SPLINE_SURFACE ( (
 ( 1.000000000000000000, 1.000000000000000000),
 ( 0.9593753223639863714, 0.9995975284513187731),
 ( 0.9593753223639863714, 0.9995975284513187731),
 ( 1.000000000000000000, 1.000000000000000000) ) ) 
 REPRESENTATION_ITEM ( '' )  SURFACE ( )  );
#13608 = ORIENTED_EDGE ( 'NONE', *, *, #7596, .T. ) ;
#13609 = CARTESIAN_POINT ( 'NONE',  ( -25.21435515916042647, 25.00736669481023355, -23.92354251275945742 ) ) ;
#13610 = ADVANCED_FACE ( 'NONE', ( #26720 ), #10639, .F. ) ;
#13611 = CARTESIAN_POINT ( 'NONE',  ( 1.832998868059858122, -125.4013017422236089, 73.01698022778313657 ) ) ;
#13612 = CARTESIAN_POINT ( 'NONE',  ( 55.49584447822657296, -22.16497542184357883, -69.08290406177603415 ) ) ;
#13613 = ORIENTED_EDGE ( 'NONE', *, *, #17546, .F. ) ;
#13614 = CARTESIAN_POINT ( 'NONE',  ( 25.64681081121879203, 110.5293738517611501, -23.06870491922213873 ) ) ;
#13615 = ORIENTED_EDGE ( 'NONE', *, *, #24034, .F. ) ;
#13616 = CARTESIAN_POINT ( 'NONE',  ( 32.73300124599736449, -116.5274707358856574, 16.10546300444784507 ) ) ;
#13617 = EDGE_CURVE ( 'NONE', #1061, #2385, #22429, .T. ) ;
#13618 = CARTESIAN_POINT ( 'NONE',  ( 1.833691583653519919, 15.52203496789107895, -144.2771263798445602 ) ) ;
#13619 = VERTEX_POINT ( 'NONE', #680 ) ;
#13620 = CARTESIAN_POINT ( 'NONE',  ( 25.69398547355838858, 112.2438548322124490, -12.54367966927931555 ) ) ;
#13621 = ORIENTED_EDGE ( 'NONE', *, *, #10379, .F. ) ;
#13622 = CARTESIAN_POINT ( 'NONE',  ( 109.1586900883932856, -0.006231977675085013588, -0.003481399864218412150 ) ) ;
#13623 = VERTEX_POINT ( 'NONE', #9471 ) ;
#13624 = CARTESIAN_POINT ( 'NONE',  ( 25.64708228042121618, 103.1656011680039171, -45.88917180166176024 ) ) ;
#13625 = B_SPLINE_CURVE_WITH_KNOTS ( 'NONE', 3,
 ( #20081, #26844, #2818, #22701, #9446, #13743, #11593, #7153 ),
 .UNSPECIFIED., .F., .F.,
 ( 4, 2, 2, 4 ),
 ( 0.000000000000000000, 0.0002429588503611188825, 0.0004859177007222377650, 0.0009718354014444807341 ),
 .UNSPECIFIED. ) ;
#13626 = CARTESIAN_POINT ( 'NONE',  ( -55.25297051322618813, -0.01354497706059463319, 0.006313402748432140991 ) ) ;
#13627 = CARTESIAN_POINT ( 'NONE',  ( 8.186469777910962975, 27.65107827750279412, -146.7694294853779695 ) ) ;
#13628 = FACE_OUTER_BOUND ( 'NONE', #9698, .T. ) ;
#13629 = CARTESIAN_POINT ( 'NONE',  ( 32.73300124599741423, -75.82012867748416340, -89.94078864464141532 ) ) ;
#13630 = CARTESIAN_POINT ( 'NONE',  ( 1.833750490713699666, -125.8019536335925324, 72.32354185792516432 ) ) ;
#13631 = ORIENTED_EDGE ( 'NONE', *, *, #10371, .F. ) ;
#13632 = CARTESIAN_POINT ( 'NONE',  ( 109.1778270068192853, 0.006489198140358630809, -0.006682187084639338963 ) ) ;
#13633 = CARTESIAN_POINT ( 'NONE',  ( 2.108985857320905932, -96.26411661813104104, 108.8271972979196818 ) ) ;
#13634 = CARTESIAN_POINT ( 'NONE',  ( -20.57838717382308502, 23.26537097894105699, -18.89542499756508320 ) ) ;
#13635 = ORIENTED_EDGE ( 'NONE', *, *, #9103, .F. ) ;
#13636 = ORIENTED_EDGE ( 'NONE', *, *, #24195, .T. ) ;
#13637 = ORIENTED_EDGE ( 'NONE', *, *, #22683, .F. ) ;
#13638 = CARTESIAN_POINT ( 'NONE',  ( 25.64670758986457955, -91.05338785329392692, -66.76959937251548638 ) ) ;
#13639 = CARTESIAN_POINT ( 'NONE',  ( -20.24399999263415140, -10.36954246768226717, 27.76448601145551009 ) ) ;
#13640 = ADVANCED_FACE ( 'NONE', ( #4859 ), #77, .F. ) ;
#13641 = CARTESIAN_POINT ( 'NONE',  ( -1.463510566862823437, -38.76366072687759612, 25.15876608740857989 ) ) ;
#13642 = DIRECTION ( 'NONE',  ( 1.000000000000000000, -6.938893903907226837E-18, 1.734723475976806709E-18 ) ) ;
#13643 = CARTESIAN_POINT ( 'NONE',  ( 1.833603222531958732, 144.2675221341993961, 15.61050054119080244 ) ) ;
#13644 = CARTESIAN_POINT ( 'NONE',  ( 16.05277956358204605, -48.70400867629005148, -134.7758735858407988 ) ) ;
#13645 = CARTESIAN_POINT ( 'NONE',  ( 109.1592201516379674, -0.006957642258155097119, -0.003661068210032647052 ) ) ;
#13646 = EDGE_LOOP ( 'NONE', ( #19756, #13911, #16321, #24403 ) ) ;
#13647 = CARTESIAN_POINT ( 'NONE',  ( 109.1592201516379674, 0.005631912476305695608, 0.005485778713193766379 ) ) ;
#13648 = CARTESIAN_POINT ( 'NONE',  ( 26.11404676487257603, 90.92995828888199128, 67.46175819463394419 ) ) ;
#13649 =( BOUNDED_SURFACE ( )  B_SPLINE_SURFACE ( 3, 1, ( 
 ( #24114, #28397 ),
 ( #19765, #10865 ),
 ( #26249, #13150 ),
 ( #19627, #12859 ) ),
 .UNSPECIFIED., .F., .F., .F. ) 
 B_SPLINE_SURFACE_WITH_KNOTS ( ( 4, 4 ),
 ( 2, 2 ),
 ( 0.000000000000000000, 1.000000000000000000 ),
 ( 0.000000000000000000, 1.000000000000000000 ),
 .UNSPECIFIED. ) 
 GEOMETRIC_REPRESENTATION_ITEM ( )  RATIONAL_B_SPLINE_SURFACE ( (
 ( 1.000000000000000000, 1.000000000000000000),
 ( 0.7789835883360578528, 0.9689951854195403280),
 ( 0.7789835883360578528, 0.9689951854195403280),
 ( 1.000000000000000000, 1.000000000000000000) ) ) 
 REPRESENTATION_ITEM ( '' )  SURFACE ( )  );
#13650 = CARTESIAN_POINT ( 'NONE',  ( 25.64692872815577473, -0.3216598674791715240, 112.9107203549055498 ) ) ;
#13651 = CARTESIAN_POINT ( 'NONE',  ( -12.94347594948482083, 21.16159467081353540, -43.91326021875521946 ) ) ;
#13652 = EDGE_CURVE ( 'NONE', #10146, #19, #22331, .T. ) ;
#13653 = CARTESIAN_POINT ( 'NONE',  ( -1.045287976400383290, 36.12803364096649972, 28.14015102489766917 ) ) ;
#13654 = EDGE_CURVE ( 'NONE', #378, #19503, #26870, .T. ) ;
#13655 = CARTESIAN_POINT ( 'NONE',  ( 2.263178113027036531, 142.5035404044877509, -28.85718369185572385 ) ) ;
#13656 = CARTESIAN_POINT ( 'NONE',  ( 2.108985857320916146, -142.3791757917250322, -28.95357181520974876 ) ) ;
#13657 = ORIENTED_EDGE ( 'NONE', *, *, #513, .F. ) ;
#13658 = VERTEX_POINT ( 'NONE', #252 ) ;
#13659 = VERTEX_POINT ( 'NONE', #7313 ) ;
#13660 = B_SPLINE_CURVE_WITH_KNOTS ( 'NONE', 3,
 ( #26558, #13175, #365, #2373, #20083, #11312 ),
 .UNSPECIFIED., .F., .F.,
 ( 4, 2, 4 ),
 ( 2.778605206969998010E-17, 0.0006311571484586182574, 0.001262314296917208976 ),
 .UNSPECIFIED. ) ;
#13661 = CARTESIAN_POINT ( 'NONE',  ( -55.24300891470648622, 0.009439835024157980023, -0.002702093572889658051 ) ) ;
#13662 = CARTESIAN_POINT ( 'NONE',  ( -20.21097721650787093, 28.26295598655185515, 8.835581399094868615 ) ) ;
#13663 = CARTESIAN_POINT ( 'NONE',  ( -20.24419206586952313, 16.36655224501367911, -24.70913649113835930 ) ) ;
#13664 = CARTESIAN_POINT ( 'NONE',  ( 14.74894986621300319, -1.023413983156987147E-16, 2.558534957892467869E-17 ) ) ;
#13665 = CARTESIAN_POINT ( 'NONE',  ( 1.833809397773860761, 125.7576368866153729, -72.40070666294458590 ) ) ;
#13666 = CARTESIAN_POINT ( 'NONE',  ( 25.64681081121879203, 66.70335573067988832, -91.10197563707880875 ) ) ;
#13667 = CARTESIAN_POINT ( 'NONE',  ( 25.64704443564079028, -103.2037466592377797, 45.80316013050799029 ) ) ;
#13668 = LINE ( 'NONE', #13109, #8899 ) ;
#13669 = ORIENTED_EDGE ( 'NONE', *, *, #21702, .F. ) ;
#13670 = ORIENTED_EDGE ( 'NONE', *, *, #19181, .T. ) ;
#13671 = CARTESIAN_POINT ( 'NONE',  ( 2.430230287190572103, -118.5711603495687001, 84.35270093935217517 ) ) ;
#13672 = CARTESIAN_POINT ( 'NONE',  ( 21.16825799904894012, 131.4851843440081609, -32.46271504707809896 ) ) ;
#13673 = ADVANCED_FACE ( 'NONE', ( #9041 ), #7843, .F. ) ;
#13674 = CARTESIAN_POINT ( 'NONE',  ( 1.834118845439484335, -144.2964192726481087, -15.34511559672828795 ) ) ;
#13675 = LINE ( 'NONE', #7513, #19316 ) ;
#13676 = CARTESIAN_POINT ( 'NONE',  ( 1.833809397773844774, 58.85883548850593883, 132.6366580004809350 ) ) ;
#13677 = CARTESIAN_POINT ( 'NONE',  ( -1.583189561560253589, 25.21827308671232259, -38.94740041318303270 ) ) ;
#13678 = EDGE_CURVE ( 'NONE', #4666, #23146, #19862, .T. ) ;
#13679 = EDGE_CURVE ( 'NONE', #9661, #14713, #20960, .T. ) ;
#13680 = CARTESIAN_POINT ( 'NONE',  ( -20.20700224038492010, -8.199606986804138131, 28.44216453106544762 ) ) ;
#13681 = CARTESIAN_POINT ( 'NONE',  ( -1.031422197589711764, -15.60268798220608488, 43.06660437151322895 ) ) ;
#13682 = CARTESIAN_POINT ( 'NONE',  ( 109.1586900883932856, -0.005715190711488750061, -0.004277182003220933101 ) ) ;
#13683 = CARTESIAN_POINT ( 'NONE',  ( -8.786685647604890903, 37.00619870957935120, -38.68584556812312059 ) ) ;
#13684 = ORIENTED_EDGE ( 'NONE', *, *, #5267, .F. ) ;
#13685 = CARTESIAN_POINT ( 'NONE',  ( -20.20700224038492010, -10.08426345511570332, 27.82980252387829623 ) ) ;
#13686 = CARTESIAN_POINT ( 'NONE',  ( 109.1586059443104944, 0.005983234375919677800, 0.003774052605959055031 ) ) ;
#13687 = ORIENTED_EDGE ( 'NONE', *, *, #5871, .F. ) ;
#13688 =( BOUNDED_SURFACE ( )  B_SPLINE_SURFACE ( 3, 1, ( 
 ( #21331, #19172 ),
 ( #14304, #25939 ),
 ( #3918, #21470 ),
 ( #1742, #16186 ) ),
 .UNSPECIFIED., .F., .F., .F. ) 
 B_SPLINE_SURFACE_WITH_KNOTS ( ( 4, 4 ),
 ( 2, 2 ),
 ( 0.000000000000000000, 1.000000000000000000 ),
 ( 0.000000000000000000, 1.000000000000000000 ),
 .UNSPECIFIED. ) 
 GEOMETRIC_REPRESENTATION_ITEM ( )  RATIONAL_B_SPLINE_SURFACE ( (
 ( 1.000000000000000000, 1.000000000000000000),
 ( 0.9934239774497838349, 0.8357310067453913582),
 ( 0.9934239774497838349, 0.8357310067453913582),
 ( 1.000000000000000000, 1.000000000000000000) ) ) 
 REPRESENTATION_ITEM ( '' )  SURFACE ( )  );
#13689 = ORIENTED_EDGE ( 'NONE', *, *, #3349, .T. ) ;
#13690 = ORIENTED_EDGE ( 'NONE', *, *, #7857, .F. ) ;
#13691 = DIRECTION ( 'NONE',  ( 5.541455922705463698E-20, -5.223019709708320524E-21, 1.000000000000000000 ) ) ;
#13692 = DIRECTION ( 'NONE',  ( 0.5946245182733608248, 0.7637359336799388609, 0.2512550613902251873 ) ) ;
#13693 = CARTESIAN_POINT ( 'NONE',  ( 32.73300124599735739, 62.10906484417237294, 99.90245962373859356 ) ) ;
#13694 = B_SPLINE_CURVE_WITH_KNOTS ( 'NONE', 3,
 ( #21148, #25349, #1289, #5623, #14388, #12239, #21004, #10088, #18854, #24304 ),
 .UNSPECIFIED., .F., .F.,
 ( 4, 3, 3, 4 ),
 ( 3.925231146709437917E-17, 0.0002669559177086282546, 0.0005339118354151181373, 0.001067817517169144300 ),
 .UNSPECIFIED. ) ;
#13695 = CARTESIAN_POINT ( 'NONE',  ( 10.93730112726002623, 56.95489579269933955, -140.0398180619107507 ) ) ;
#13696 = LINE ( 'NONE', #4928, #5581 ) ;
#13697 = CARTESIAN_POINT ( 'NONE',  ( 1.831572820252009626, -145.1082523917587253, 0.9871191512909551768 ) ) ;
#13698 = EDGE_CURVE ( 'NONE', #22671, #15612, #12195, .T. ) ;
#13699 = CARTESIAN_POINT ( 'NONE',  ( -1.583189561560255143, 25.21827308671289103, 38.94740041318266321 ) ) ;
#13700 = CARTESIAN_POINT ( 'NONE',  ( -8.786685647604890903, -9.545808661480235102, 52.67761315067295413 ) ) ;
#13701 = CARTESIAN_POINT ( 'NONE',  ( 10.93730112725972070, -51.37919228020375328, 142.1801301103782293 ) ) ;
#13702 = CARTESIAN_POINT ( 'NONE',  ( 25.65782528836479770, 34.34372400279251281, 107.5689571161380229 ) ) ;
#13703 = EDGE_CURVE ( 'NONE', #1901, #6478, #15725, .T. ) ;
#13704 = EDGE_CURVE ( 'NONE', #5932, #14392, #21248, .T. ) ;
#13705 = CARTESIAN_POINT ( 'NONE',  ( 1.833485406944057594, -108.1939177044919376, -96.69979900902278303 ) ) ;
#13706 = CARTESIAN_POINT ( 'NONE',  ( 26.28373643307401153, 119.9673604189463703, -43.35364178852652373 ) ) ;
#13707 = VECTOR ( 'NONE', #15956, 1000.000000000000000 ) ;
#13708 = CARTESIAN_POINT ( 'NONE',  ( 1.833750490713655479, -117.5529286802293569, 85.07723081767849749 ) ) ;
#13709 = ORIENTED_EDGE ( 'NONE', *, *, #9725, .T. ) ;
#13710 = CARTESIAN_POINT ( 'NONE',  ( 8.186469829614001270, 134.9918587494112501, 63.89871393833048074 ) ) ;
#13711 = DIRECTION ( 'NONE',  ( 0.000000000000000000, 0.000000000000000000, 1.000000000000000000 ) ) ;
#13712 = CARTESIAN_POINT ( 'NONE',  ( 25.64699802086721903, 46.14225289916308270, 103.0525896353903335 ) ) ;
#13713 = B_SPLINE_CURVE_WITH_KNOTS ( 'NONE', 3,
 ( #15046, #11173, #21684, #24420 ),
 .UNSPECIFIED., .F., .F.,
 ( 4, 4 ),
 ( 3.221104623179000266E-16, 0.01077107486149802423 ),
 .UNSPECIFIED. ) ;
#13714 = CARTESIAN_POINT ( 'NONE',  ( 109.1587776205901577, -0.005978137617714252700, 0.004240403845337341153 ) ) ;
#13715 = DIRECTION ( 'NONE',  ( 0.000000000000000000, 0.000000000000000000, 1.000000000000000000 ) ) ;
#13716 = ORIENTED_EDGE ( 'NONE', *, *, #12696, .T. ) ;
#13717 = DIRECTION ( 'NONE',  ( 0.000000000000000000, 0.000000000000000000, 1.000000000000000000 ) ) ;
#13718 = VERTEX_POINT ( 'NONE', #25298 ) ;
#13719 = CARTESIAN_POINT ( 'NONE',  ( 1.831572820252008738, 84.49389457294135752, 117.9752562883669782 ) ) ;
#13720 = CARTESIAN_POINT ( 'NONE',  ( 10.93730112725932635, 0.000000000000000000, 0.000000000000000000 ) ) ;
#13721 = ORIENTED_EDGE ( 'NONE', *, *, #12357, .T. ) ;
#13722 = FACE_OUTER_BOUND ( 'NONE', #2142, .T. ) ;
#13723 = VERTEX_POINT ( 'NONE', #3692 ) ;
#13724 = CARTESIAN_POINT ( 'NONE',  ( 32.73300124599739291, 92.86301839380121237, -72.21147546950456331 ) ) ;
#13725 =( BOUNDED_SURFACE ( )  B_SPLINE_SURFACE ( 3, 1, ( 
 ( #2160, #10831 ),
 ( #17566, #2599 ),
 ( #11383, #26354 ),
 ( #17712, #20156 ) ),
 .UNSPECIFIED., .F., .F., .F. ) 
 B_SPLINE_SURFACE_WITH_KNOTS ( ( 4, 4 ),
 ( 2, 2 ),
 ( 0.000000000000000000, 1.000000000000000000 ),
 ( 0.000000000000000000, 1.000000000000000000 ),
 .UNSPECIFIED. ) 
 GEOMETRIC_REPRESENTATION_ITEM ( )  RATIONAL_B_SPLINE_SURFACE ( (
 ( 1.000000000000000000, 1.000000000000000000),
 ( 0.7789835883360576307, 0.9689951854195403280),
 ( 0.7789835883360576307, 0.9689951854195403280),
 ( 1.000000000000000000, 1.000000000000000000) ) ) 
 REPRESENTATION_ITEM ( '' )  SURFACE ( )  );
#13726 = EDGE_LOOP ( 'NONE', ( #7814, #26726, #13721, #23126 ) ) ;
#13727 = B_SPLINE_CURVE_WITH_KNOTS ( 'NONE', 3,
 ( #17177, #6255, #19614, #17310, #26099, #6387, #23959 ),
 .UNSPECIFIED., .F., .F.,
 ( 4, 3, 4 ),
 ( 1.734723475976807094E-18, 0.009512539173626382780, 0.02506242213020817150 ),
 .UNSPECIFIED. ) ;
#13728 = CARTESIAN_POINT ( 'NONE',  ( 32.73300124599737870, -117.5726003567929041, -3.836798148480059734 ) ) ;
#13729 = EDGE_CURVE ( 'NONE', #14557, #4557, #9957, .T. ) ;
#13730 = DIRECTION ( 'NONE',  ( 0.000000000000000000, -5.223019709708190374E-21, 1.000000000000000000 ) ) ;
#13731 = EDGE_CURVE ( 'NONE', #21696, #15588, #3409, .T. ) ;
#13732 = CARTESIAN_POINT ( 'NONE',  ( -1.583189561560256253, -25.21827308671203838, 38.94740041318321744 ) ) ;
#13733 = CARTESIAN_POINT ( 'NONE',  ( 25.64708228042121974, -66.39944550735333451, 91.32398912287000314 ) ) ;
#13734 = ADVANCED_FACE ( 'NONE', ( #18529 ), #10341, .T. ) ;
#13735 = CARTESIAN_POINT ( 'NONE',  ( -8.259864102781671491, 9.986657004933631399, -52.06232470801713674 ) ) ;
#13736 = CYLINDRICAL_SURFACE ( 'NONE', #10727, 20.00000000000000000 ) ;
#13737 = CARTESIAN_POINT ( 'NONE',  ( 25.64660436782548203, -34.33930645842076501, 107.5626123667558289 ) ) ;
#13738 = CARTESIAN_POINT ( 'NONE',  ( 24.01988960052056044, -90.81495976423860839, 94.47404045191606770 ) ) ;
#13739 = ORIENTED_EDGE ( 'NONE', *, *, #20573, .T. ) ;
#13740 = CARTESIAN_POINT ( 'NONE',  ( -55.24271866751342941, -0.009369360294295350430, -0.001545935011630812216 ) ) ;
#13742 = CARTESIAN_POINT ( 'NONE',  ( 25.64681081121879203, 45.54494737132223747, 103.3177883989780952 ) ) ;
#13741 = DIRECTION ( 'NONE',  ( -0.5946245182733607137, 0.7992853357633884492, -0.08697490616138101038 ) ) ;
#13743 = CARTESIAN_POINT ( 'NONE',  ( 25.86096068574583029, -84.67961880569343691, 74.90357932134600105 ) ) ;
#13744 = CARTESIAN_POINT ( 'NONE',  ( -6.574463467970635300, 47.03022655117400319, -20.55340846381147202 ) ) ;
#13745 = CARTESIAN_POINT ( 'NONE',  ( -1.619063947482197729, -35.99532424477401094, -29.22875152547743838 ) ) ;
#13746 = ORIENTED_EDGE ( 'NONE', *, *, #17059, .F. ) ;
#13747 = CARTESIAN_POINT ( 'NONE',  ( 26.28373643307438812, 127.4927519498662321, -4.159810388346843801 ) ) ;
#13748 = CARTESIAN_POINT ( 'NONE',  ( -20.57838717382308147, 16.28767523336157552, 25.16001208503087838 ) ) ;
#13749 = CARTESIAN_POINT ( 'NONE',  ( 32.73300124599740002, -81.52272205837138586, -84.80615050150450429 ) ) ;
#13750 = VERTEX_POINT ( 'NONE', #6014 ) ;
#13751 = DIRECTION ( 'NONE',  ( 0.000000000000000000, 0.000000000000000000, 1.000000000000000000 ) ) ;
#13752 = EDGE_LOOP ( 'NONE', ( #24630, #21052, #14600, #15352 ) ) ;
#13753 = CARTESIAN_POINT ( 'NONE',  ( -1.259972190295304939, 2.243354636026407611, 45.95417440459613800 ) ) ;
#13754 = CARTESIAN_POINT ( 'NONE',  ( 2.433796855181219243, 132.3327394885239698, -60.50726454507772445 ) ) ;
#13755 = ORIENTED_EDGE ( 'NONE', *, *, #27256, .T. ) ;
#13756 = CARTESIAN_POINT ( 'NONE',  ( 24.22246935314087324, 2.449293598294706119E-15, 20.00000000000000000 ) ) ;
#13757 = EDGE_CURVE ( 'NONE', #9758, #14288, #8213, .T. ) ;
#13758 = ORIENTED_EDGE ( 'NONE', *, *, #7857, .T. ) ;
#13759 = CARTESIAN_POINT ( 'NONE',  ( -22.23226125620943705, -29.33577758406442726, 11.82389163795241593 ) ) ;
#13760 = ADVANCED_FACE ( 'NONE', ( #27297 ), #20664, .F. ) ;
#13761 = EDGE_LOOP ( 'NONE', ( #7132, #10606, #20455, #1240 ) ) ;
#13762 =( NAMED_UNIT ( * ) SI_UNIT ( $, .STERADIAN. ) SOLID_ANGLE_UNIT ( ) );
#13763 = B_SPLINE_CURVE_WITH_KNOTS ( 'NONE', 3,
 ( #28002, #12604, #8041, #23577, #10598, #8301, #23723 ),
 .UNSPECIFIED., .F., .F.,
 ( 4, 3, 4 ),
 ( 7.571427111245364237E-17, 0.02816610861753245099, 0.04000277880656218782 ),
 .UNSPECIFIED. ) ;
#13764 = CARTESIAN_POINT ( 'NONE',  ( 55.49584447822657296, 7.317474139116590948, -72.18163437663932314 ) ) ;
#13765 = AXIS2_PLACEMENT_3D ( 'NONE', #25603, #25170, #27751 ) ;
#13766 = ADVANCED_FACE ( 'NONE', ( #24132 ), #10773, .F. ) ;
#13767 = CARTESIAN_POINT ( 'NONE',  ( 25.64681081121879203, -35.28660243342623204, 107.2555980796239936 ) ) ;
#13768 = DIRECTION ( 'NONE',  ( -1.000000000000000000, -0.000000000000000000, -0.000000000000000000 ) ) ;
#13769 = ORIENTED_EDGE ( 'NONE', *, *, #25949, .T. ) ;
#13770 =( BOUNDED_SURFACE ( )  B_SPLINE_SURFACE ( 3, 1, ( 
 ( #5487, #7813 ),
 ( #18874, #12527 ),
 ( #27647, #7963 ),
 ( #23357, #12385 ) ),
 .UNSPECIFIED., .F., .F., .F. ) 
 B_SPLINE_SURFACE_WITH_KNOTS ( ( 4, 4 ),
 ( 2, 2 ),
 ( 0.000000000000000000, 1.000000000000000000 ),
 ( 0.000000000000000000, 1.000000000000000000 ),
 .UNSPECIFIED. ) 
 GEOMETRIC_REPRESENTATION_ITEM ( )  RATIONAL_B_SPLINE_SURFACE ( (
 ( 1.000000000000000000, 1.000000000000000000),
 ( 0.9956975270656954757, 0.8568959468854893125),
 ( 0.9956975270656954757, 0.8568959468854893125),
 ( 1.000000000000000000, 1.000000000000000000) ) ) 
 REPRESENTATION_ITEM ( '' )  SURFACE ( )  );
#13771 = EDGE_CURVE ( 'NONE', #8435, #20441, #12983, .T. ) ;
#13772 = CARTESIAN_POINT ( 'NONE',  ( 2.433796855181205476, 74.00833731765735024, -125.2830755159746445 ) ) ;
#13773 = CARTESIAN_POINT ( 'NONE',  ( -1.583189561560255143, -44.83405390829663872, 11.94859433442949381 ) ) ;
#13774 = CARTESIAN_POINT ( 'NONE',  ( 25.64681081121879203, 91.10197563707947666, 66.70335573067896462 ) ) ;
#13775 = ORIENTED_EDGE ( 'NONE', *, *, #21086, .F. ) ;
#13776 = VERTEX_POINT ( 'NONE', #8577 ) ;
#13777 = ORIENTED_EDGE ( 'NONE', *, *, #6348, .F. ) ;
#13778 = CARTESIAN_POINT ( 'NONE',  ( -1.050230346682684113, 37.05182464822020449, 26.92058491724826297 ) ) ;
#13779 = CARTESIAN_POINT ( 'NONE',  ( 1.832998868059858122, -132.7810136645742318, 58.53348008137599834 ) ) ;
#13781 = CARTESIAN_POINT ( 'NONE',  ( 26.11404676487257603, -24.64483677384923865, 110.5078194225160360 ) ) ;
#13780 = CARTESIAN_POINT ( 'NONE',  ( 109.1778270068192853, -0.009220257877172541999, -0.001322180554006281445 ) ) ;
#13782 = CARTESIAN_POINT ( 'NONE',  ( -8.259864102781492079, -38.68084189741939127, 36.24929574824932388 ) ) ;
#13783 = CARTESIAN_POINT ( 'NONE',  ( -55.24271866751342941, 0.006757859501010507128, -0.006671293903668127322 ) ) ;
#13784 = CARTESIAN_POINT ( 'NONE',  ( -16.86833981943425087, -31.95666732167541113, 30.57013526701953054 ) ) ;
#13785 = CARTESIAN_POINT ( 'NONE',  ( -8.786685647604890903, -52.67761315067279781, 9.545808661481174795 ) ) ;
#13786 = ORIENTED_EDGE ( 'NONE', *, *, #6968, .F. ) ;
#13787 = CARTESIAN_POINT ( 'NONE',  ( 24.01988960052067412, -123.2441023955613275, -44.53753990739630098 ) ) ;
#13788 = CARTESIAN_POINT ( 'NONE',  ( 26.11404676487257603, 97.48350837663606683, 57.58742681967482469 ) ) ;
#13789 = CARTESIAN_POINT ( 'NONE',  ( 1.833838848569418367, -145.1097630730648973, 0.1779716374152634506 ) ) ;
#13790 = CARTESIAN_POINT ( 'NONE',  ( 6.224689322667630975, 100.9623537450666788, -108.2965163446063883 ) ) ;
#13791 = CARTESIAN_POINT ( 'NONE',  ( 30.59141879584285917, -49.72305007553517697, 105.0379937202712313 ) ) ;
#13792 = CARTESIAN_POINT ( 'NONE',  ( 1.894214914920944626, 142.1734439042097904, 29.24491455758985481 ) ) ;
#13793 = ORIENTED_EDGE ( 'NONE', *, *, #13131, .T. ) ;
#13794 = CARTESIAN_POINT ( 'NONE',  ( 109.1586900883932856, -0.001582822706024298925, 0.006960773163856026798 ) ) ;
#13795 = EDGE_CURVE ( 'NONE', #1161, #16650, #4251, .T. ) ;
#13796 = ORIENTED_EDGE ( 'NONE', *, *, #25943, .T. ) ;
#13797 = CARTESIAN_POINT ( 'NONE',  ( -21.81686047589426991, 37.90526371014259155, -6.867757412720813193 ) ) ;
#13798 = B_SPLINE_CURVE_WITH_KNOTS ( 'NONE', 3,
 ( #14896, #25285, #10178, #5557, #17617, #17468, #24257, #24400, #8856, #26256 ),
 .UNSPECIFIED., .F., .F.,
 ( 4, 2, 2, 2, 4 ),
 ( 5.898697549827394244E-18, 0.0003346267210630972291, 0.0006692534421261884950, 0.001003880163189279761, 0.001338506884252371135 ),
 .UNSPECIFIED. ) ;
#13799 = CARTESIAN_POINT ( 'NONE',  ( -1.583189561560253589, 44.83405390829688741, 11.94859433442854701 ) ) ;
#13800 = VERTEX_POINT ( 'NONE', #19369 ) ;
#13801 = ORIENTED_EDGE ( 'NONE', *, *, #7169, .T. ) ;
#13802 = ORIENTED_EDGE ( 'NONE', *, *, #20637, .T. ) ;
#13803 = EDGE_CURVE ( 'NONE', #5626, #15445, #1318, .T. ) ;
#13804 = CARTESIAN_POINT ( 'NONE',  ( 25.64660436782549624, 84.29628170537259280, 75.12017330820509642 ) ) ;
#13805 = CARTESIAN_POINT ( 'NONE',  ( -25.21435515916043713, -34.05351380035337883, -6.169479169075319014 ) ) ;
#13806 = EDGE_CURVE ( 'NONE', #431, #8144, #2079, .T. ) ;
#13807 = VECTOR ( 'NONE', #11870, 1000.000000000000114 ) ;
#13808 = DIRECTION ( 'NONE',  ( -0.5946245182733608248, 0.1700465163848199623, 0.7858154137795725358 ) ) ;
#13809 = CARTESIAN_POINT ( 'NONE',  ( 2.433796855181205476, 43.58222566461644476, 138.8296532063089614 ) ) ;
#13810 = ORIENTED_EDGE ( 'NONE', *, *, #22603, .F. ) ;
#13811 = CARTESIAN_POINT ( 'NONE',  ( -8.786685647604890903, 23.24040270374391426, -48.22796981442777309 ) ) ;
#13812 = AXIS2_PLACEMENT_3D ( 'NONE', #5023, #18256, #7346 ) ;
#13813 = CARTESIAN_POINT ( 'NONE',  ( 25.64692232868535626, 35.20209749635309748, 107.2834780834836863 ) ) ;
#13814 = CARTESIAN_POINT ( 'NONE',  ( -28.13707043255157103, -7.802116958608856123, 21.52861750560947129 ) ) ;
#13815 = ORIENTED_EDGE ( 'NONE', *, *, #10833, .F. ) ;
#13817 = AXIS2_PLACEMENT_3D ( 'NONE', #9402, #7683, #18449 ) ;
#13816 =( BOUNDED_SURFACE ( )  B_SPLINE_SURFACE ( 3, 1, ( 
 ( #16417, #22917 ),
 ( #2740, #25202 ),
 ( #5476, #14236 ),
 ( #23058, #11520 ) ),
 .UNSPECIFIED., .F., .F., .F. ) 
 B_SPLINE_SURFACE_WITH_KNOTS ( ( 4, 4 ),
 ( 2, 2 ),
 ( 0.000000000000000000, 1.000000000000000000 ),
 ( 0.000000000000000000, 1.000000000000000000 ),
 .UNSPECIFIED. ) 
 GEOMETRIC_REPRESENTATION_ITEM ( )  RATIONAL_B_SPLINE_SURFACE ( (
 ( 1.000000000000000000, 1.000000000000000000),
 ( 0.7789835883360578528, 0.9689951854195403280),
 ( 0.7789835883360578528, 0.9689951854195403280),
 ( 1.000000000000000000, 1.000000000000000000) ) ) 
 REPRESENTATION_ITEM ( '' )  SURFACE ( )  );
#13818 = EDGE_LOOP ( 'NONE', ( #4670, #7290, #6469, #25188 ) ) ;
#13819 = CARTESIAN_POINT ( 'NONE',  ( -1.619063947482197729, -43.26576862488421682, 16.67502769180607203 ) ) ;
#13820 = CARTESIAN_POINT ( 'NONE',  ( 30.58324630866341920, 117.4177132550300797, -28.99049605145613384 ) ) ;
#13821 = CARTESIAN_POINT ( 'NONE',  ( -7.711401346138398338, -6.030154970217270538, -52.11446537925909439 ) ) ;
#13822 = B_SPLINE_CURVE_WITH_KNOTS ( 'NONE', 3,
 ( #19837, #1851, #4157, #26179, #8214, #12657, #21726 ),
 .UNSPECIFIED., .F., .F.,
 ( 4, 3, 4 ),
 ( 5.212144047491128852E-16, 0.02816610861753249262, 0.04000277880656270824 ),
 .UNSPECIFIED. ) ;
#13823 = FACE_OUTER_BOUND ( 'NONE', #13005, .T. ) ;
#13824 = CARTESIAN_POINT ( 'NONE',  ( -28.41354790283022069, -1.249099604786914286, 23.16239616762932130 ) ) ;
#13825 = ORIENTED_EDGE ( 'NONE', *, *, #9691, .T. ) ;
#13826 = CARTESIAN_POINT ( 'NONE',  ( -1.031422197589716205, 15.60268798220638509, -43.06660437151315080 ) ) ;
#13827 = CARTESIAN_POINT ( 'NONE',  ( 10.93730112725932635, 0.000000000000000000, 0.000000000000000000 ) ) ;
#13828 = CARTESIAN_POINT ( 'NONE',  ( -4.162674018437131807, -37.46098494546610880, -31.44946543094281921 ) ) ;
#13829 = CARTESIAN_POINT ( 'NONE',  ( -20.57838717382308147, -1.611677988432568709, -29.92853265176830746 ) ) ;
#13830 = CARTESIAN_POINT ( 'NONE',  ( 25.64681081121879203, -0.4157506337719985012, -112.9102952884414606 ) ) ;
#13831 = ORIENTED_EDGE ( 'NONE', *, *, #21155, .F. ) ;
#13832 = CARTESIAN_POINT ( 'NONE',  ( 119.2224693531408803, 6.938893903907200768E-15, -19.99999999999997868 ) ) ;
#13833 = CIRCLE ( 'NONE', #4643, 53.53553390275978785 ) ;
#13834 = EDGE_LOOP ( 'NONE', ( #10719, #15666, #27745, #23465 ) ) ;
#13835 = CONICAL_SURFACE ( 'NONE', #19359, 34.60786435723138510, 0.8559913436420825139 ) ;
#13836 = ORIENTED_EDGE ( 'NONE', *, *, #8647, .F. ) ;
#13837 = ORIENTED_EDGE ( 'NONE', *, *, #2413, .F. ) ;
#13838 = VECTOR ( 'NONE', #21668, 999.9999999999998863 ) ;
#13839 = CARTESIAN_POINT ( 'NONE',  ( -1.259920593601972838, -2.243284667987463621, 45.95412615877144447 ) ) ;
#13840 = B_SPLINE_CURVE_WITH_KNOTS ( 'NONE', 3,
 ( #22126, #8897, #27403, #16323, #20096, #13483 ),
 .UNSPECIFIED., .F., .F.,
 ( 4, 2, 4 ),
 ( 1.552747097607904257E-16, 0.003570751334075639161, 0.007141502668151123064 ),
 .UNSPECIFIED. ) ;
#13841 = EDGE_CURVE ( 'NONE', #23252, #3538, #1665, .T. ) ;
#13842 = CARTESIAN_POINT ( 'NONE',  ( -1.031422197589711987, -36.13727897780105991, 28.14735071801782595 ) ) ;
#13843 = DIRECTION ( 'NONE',  ( 0.000000000000000000, 1.000000000000000000, 0.000000000000000000 ) ) ;
#13844 = EDGE_CURVE ( 'NONE', #16927, #4626, #12881, .T. ) ;
#13845 = CARTESIAN_POINT ( 'NONE',  ( 6.224689322667647851, 129.4863684118287495, 71.79702446228348833 ) ) ;
#13846 = EDGE_CURVE ( 'NONE', #16481, #5027, #26045, .T. ) ;
#13847 = LINE ( 'NONE', #20900, #25 ) ;
#13848 = CARTESIAN_POINT ( 'NONE',  ( -1.044556982611280160, 1.643392503293353180, 45.76404732357876526 ) ) ;
#13849 = CARTESIAN_POINT ( 'NONE',  ( 25.64670758986458310, -35.36461833156593570, 107.2298587623394326 ) ) ;
#13850 = AXIS2_PLACEMENT_3D ( 'NONE', #27730, #14333, #27867 ) ;
#13851 = CARTESIAN_POINT ( 'NONE',  ( 26.11404676487259024, 10.71016160607567080, 112.7148551500680753 ) ) ;
#13852 = VECTOR ( 'NONE', #90, 1000.000000000000114 ) ;
#13853 = CARTESIAN_POINT ( 'NONE',  ( 1.833838850855487257, -85.22139087168996241, -117.4485666028826785 ) ) ;
#13854 = CARTESIAN_POINT ( 'NONE',  ( -55.24390624410018802, -0.007503127514281482044, 0.007245494385991411469 ) ) ;
#13855 = DIRECTION ( 'NONE',  ( -0.5914120900931443270, 0.5455001977188052020, 0.5938529060132676785 ) ) ;
#13856 = AXIS2_PLACEMENT_3D ( 'NONE', #1222, #10165, #23404 ) ;
#13857 = CARTESIAN_POINT ( 'NONE',  ( 2.430230287190572103, 142.6294793592101655, -28.83279105684286492 ) ) ;
#13858 = CARTESIAN_POINT ( 'NONE',  ( 5.340103579038071757, 111.1041836885946594, 96.93942141937336032 ) ) ;
#13859 = CARTESIAN_POINT ( 'NONE',  ( 32.73300124599735739, -81.52272205837257957, 84.80615050150346690 ) ) ;
#13860 = CARTESIAN_POINT ( 'NONE',  ( -55.24390624410018802, -0.009374879212970498032, 0.004572280736701721943 ) ) ;
#13861 = CARTESIAN_POINT ( 'NONE',  ( 109.1721716018069657, -0.01392660302850761735, -0.009868622090676126835 ) ) ;
#13862 = CARTESIAN_POINT ( 'NONE',  ( -1.619063947482201282, -11.94059994246191359, -44.80407745103779860 ) ) ;
#13863 =( BOUNDED_SURFACE ( )  B_SPLINE_SURFACE ( 3, 1, ( 
 ( #7276, #19940 ),
 ( #22252, #15757 ),
 ( #9012, #26548 ),
 ( #9295, #790 ) ),
 .UNSPECIFIED., .F., .F., .F. ) 
 B_SPLINE_SURFACE_WITH_KNOTS ( ( 4, 4 ),
 ( 2, 2 ),
 ( 0.000000000000000000, 1.000000000000000000 ),
 ( 0.000000000000000000, 1.000000000000000000 ),
 .UNSPECIFIED. ) 
 GEOMETRIC_REPRESENTATION_ITEM ( )  RATIONAL_B_SPLINE_SURFACE ( (
 ( 1.000000000000000000, 1.000000000000000000),
 ( 0.9960225298536222738, 0.9999952330161893110),
 ( 0.9960225298536222738, 0.9999952330161893110),
 ( 1.000000000000000000, 1.000000000000000000) ) ) 
 REPRESENTATION_ITEM ( '' )  SURFACE ( )  );
#13864 = EDGE_CURVE ( 'NONE', #22236, #24138, #10270, .T. ) ;
#13865 = VERTEX_POINT ( 'NONE', #3841 ) ;
#13866 = CARTESIAN_POINT ( 'NONE',  ( 30.59141879584281654, -14.83090566979504388, 115.2623358717302864 ) ) ;
#13867 = ORIENTED_EDGE ( 'NONE', *, *, #4559, .T. ) ;
#13868 = CARTESIAN_POINT ( 'NONE',  ( 32.73300124599735739, -32.68291970228314369, 113.0038235389601340 ) ) ;
#13869 = CARTESIAN_POINT ( 'NONE',  ( 2.263178113027024541, 1.401567040890216109, -145.3892419963350164 ) ) ;
#13870 = EDGE_LOOP ( 'NONE', ( #19348, #18595, #14042, #17974 ) ) ;
#13871 = ORIENTED_EDGE ( 'NONE', *, *, #1529, .F. ) ;
#13872 = ORIENTED_EDGE ( 'NONE', *, *, #13844, .F. ) ;
#13873 = B_SPLINE_CURVE_WITH_KNOTS ( 'NONE', 3,
 ( #12616, #8053, #14639, #25602 ),
 .UNSPECIFIED., .F., .F.,
 ( 4, 4 ),
 ( 1.892757412642747770E-16, 0.001982023823822945049 ),
 .UNSPECIFIED. ) ;
#13874 = EDGE_CURVE ( 'NONE', #19831, #27159, #27789, .T. ) ;
#13875 = EDGE_CURVE ( 'NONE', #1901, #16572, #17630, .T. ) ;
#13876 = AXIS2_PLACEMENT_3D ( 'NONE', #4217, #12999, #21790 ) ;
#13877 = CARTESIAN_POINT ( 'NONE',  ( 109.1592201516379674, 0.007302213399787552996, 0.002913740842103208079 ) ) ;
#13878 = CARTESIAN_POINT ( 'NONE',  ( 109.1586059443104944, 0.006260042619939234880, -0.003294606663363258692 ) ) ;
#13879 = CARTESIAN_POINT ( 'NONE',  ( -25.21435515916025594, 1.749597353048488237E-16, -4.373993382621220594E-17 ) ) ;
#13880 = CARTESIAN_POINT ( 'NONE',  ( -23.79223135445718995, -32.40779366744830270, 7.157574570129486169 ) ) ;
#13881 = CARTESIAN_POINT ( 'NONE',  ( 2.430230287190581429, 86.70145658344813455, -116.8646894862403514 ) ) ;
#13882 = CARTESIAN_POINT ( 'NONE',  ( 21.16825799904929184, 71.50503315297862628, 115.0183107335388399 ) ) ;
#13883 = LINE ( 'NONE', #7003, #28168 ) ;
#13884 = CARTESIAN_POINT ( 'NONE',  ( 25.64681081121879203, -12.21581276189883170, 112.2483031020013016 ) ) ;
#13885 = CARTESIAN_POINT ( 'NONE',  ( 10.93730112725932635, 0.000000000000000000, 0.000000000000000000 ) ) ;
#13886 = VERTEX_POINT ( 'NONE', #6712 ) ;
#13887 = ORIENTED_EDGE ( 'NONE', *, *, #25109, .F. ) ;
#13888 = CARTESIAN_POINT ( 'NONE',  ( 30.59138290137879679, 14.83088430729549323, 115.2623146671590604 ) ) ;
#13890 = CARTESIAN_POINT ( 'NONE',  ( 25.70243777736190083, 76.12033502296627319, -83.44449745408456920 ) ) ;
#13889 = CARTESIAN_POINT ( 'NONE',  ( 1.833750490713728309, 85.07723081767881013, 117.5529286802290017 ) ) ;
#13891 = LINE ( 'NONE', #20373, #9711 ) ;
#13892 = CARTESIAN_POINT ( 'NONE',  ( 1.833206308920042549, 138.2356393957902583, -44.13245285122123818 ) ) ;
#13893 = CARTESIAN_POINT ( 'NONE',  ( 1.894214914920923087, 144.4515288797483947, 14.22353624692047269 ) ) ;
#13894 = VECTOR ( 'NONE', #21567, 1000.000000000000114 ) ;
#13895 = ORIENTED_EDGE ( 'NONE', *, *, #21484, .F. ) ;
#13896 = CARTESIAN_POINT ( 'NONE',  ( 16.05277956358234448, 143.2298391883437603, -4.672229451528306932 ) ) ;
#13897 = CONICAL_SURFACE ( 'NONE', #18506, 117.6351876552689504, 0.9945805576725580410 ) ;
#13898 = CARTESIAN_POINT ( 'NONE',  ( 25.64670758986457244, 110.5460908981864776, -22.98827151089179210 ) ) ;
#13899 = CARTESIAN_POINT ( 'NONE',  ( 2.430230287190592531, -84.35270093935336888, 118.5711603495678474 ) ) ;
#13900 = VERTEX_POINT ( 'NONE', #21393 ) ;
#13901 = CARTESIAN_POINT ( 'NONE',  ( -55.24390624410018802, -0.009374879212970498032, 0.004572280736701721943 ) ) ;
#13902 = ORIENTED_EDGE ( 'NONE', *, *, #219, .F. ) ;
#13903 = EDGE_CURVE ( 'NONE', #12003, #3421, #20702, .T. ) ;
#13904 = ADVANCED_FACE ( 'NONE', ( #3972 ), #16648, .F. ) ;
#13905 = B_SPLINE_CURVE_WITH_KNOTS ( 'NONE', 3,
 ( #3436, #13010, #18689, #10862, #21799, #19624, #12214, #28394, #17457, #26665 ),
 .UNSPECIFIED., .F., .F.,
 ( 4, 2, 2, 2, 4 ),
 ( 2.845980932296679661E-16, 0.0003346187017559042144, 0.0006692374035115238257, 0.001003856105267143329, 0.001338474807022762940 ),
 .UNSPECIFIED. ) ;
#13906 = ADVANCED_FACE ( 'NONE', ( #6853 ), #23481, .T. ) ;
#13907 = EDGE_LOOP ( 'NONE', ( #26177, #27570, #28237, #3905 ) ) ;
#13908 = DIRECTION ( 'NONE',  ( -0.7637818620346800147, 0.5345501402766299481, 0.3617919495470734992 ) ) ;
#13909 = ORIENTED_EDGE ( 'NONE', *, *, #9752, .F. ) ;
#13910 = CARTESIAN_POINT ( 'NONE',  ( 109.1624594426973118, 0.01263706729759558715, -0.009754804742280831151 ) ) ;
#13911 = ORIENTED_EDGE ( 'NONE', *, *, #10034, .F. ) ;
#13912 = DIRECTION ( 'NONE',  ( 1.000000000000000000, 2.154527146642496163E-16, -2.732661769973308292E-16 ) ) ;
#13913 = VECTOR ( 'NONE', #2048, 1000.000000000000000 ) ;
#13914 = DIRECTION ( 'NONE',  ( -0.7563875759206388771, -0.6531865459554678788, 0.03500244528122777032 ) ) ;
#13915 = CIRCLE ( 'NONE', #14870, 117.6351876552689504 ) ;
#13916 = CYLINDRICAL_SURFACE ( 'NONE', #17103, 20.00000000000000000 ) ;
#13917 = CARTESIAN_POINT ( 'NONE',  ( -1.113548883309557924, 16.03115934825529010, -42.96943836789110094 ) ) ;
#13918 = CARTESIAN_POINT ( 'NONE',  ( 25.64692872815574631, 110.3764733653608516, 23.79008960806638484 ) ) ;
#13919 = ORIENTED_EDGE ( 'NONE', *, *, #24952, .F. ) ;
#13920 = CARTESIAN_POINT ( 'NONE',  ( 25.64707127832796019, 1.378041109049876443E-14, 112.9112343549835487 ) ) ;
#13921 = CARTESIAN_POINT ( 'NONE',  ( 5.340103556456308631, 147.4316330165018769, 2.303180381358696405 ) ) ;
#13922 = CARTESIAN_POINT ( 'NONE',  ( 24.01988960052073807, -17.94039809062707747, 129.8107982898199566 ) ) ;
#13923 = EDGE_LOOP ( 'NONE', ( #1346, #14965, #13309, #23768, #4667, #26570, #18415, #27879, #2235, #27469, #18875, #16045, #15803, #2515, #5131, #1735, #2537, #14900, #17923, #12636, #14507, #8913, #12908, #21049, #7503, #9358, #10585, #15586, #9650, #28396, #2703, #20870, #16589, #9190, #13292, #4732, #11008, #14950, #13236, #24703, #381, #3827, #24635, #8938, #16105, #18618, #7201, #14587, #25546, #22583, #8966, #5347, #21488, #3499, #829, #19427, #14252, #23384, #580, #6213, #23042, #3180, #2938, #12883 ) ) ;
#13924 = ORIENTED_EDGE ( 'NONE', *, *, #27117, .F. ) ;
#13925 = ORIENTED_EDGE ( 'NONE', *, *, #11709, .T. ) ;
#13926 = CARTESIAN_POINT ( 'NONE',  ( -55.25719721206881729, -0.008651607285660899843, 0.007063345920781139223 ) ) ;
#13927 = CARTESIAN_POINT ( 'NONE',  ( 1.833206308920082739, -44.13245285122170003, -138.2356393957900593 ) ) ;
#13929 = CARTESIAN_POINT ( 'NONE',  ( -55.24198130335446422, -0.006527480770973291720, -0.006617369590172134802 ) ) ;
#13928 = CARTESIAN_POINT ( 'NONE',  ( -25.21435515916043713, -34.29329011225952684, 4.655591116594705703 ) ) ;
#13930 = CARTESIAN_POINT ( 'NONE',  ( 0.000000000000000000, 0.000000000000000000, 0.000000000000000000 ) ) ;
#13931 = CARTESIAN_POINT ( 'NONE',  ( -1.058197053496163109, -28.32422455455050425, 36.00048521498983689 ) ) ;
#13932 = VERTEX_POINT ( 'NONE', #24842 ) ;
#13933 = CARTESIAN_POINT ( 'NONE',  ( -22.23226125620943705, -24.24619897613461461, 20.31044300692198945 ) ) ;
#13934 = CARTESIAN_POINT ( 'NONE',  ( -8.786685647604855376, -7.199674155859337787, -53.04920435127184675 ) ) ;
#13935 = CARTESIAN_POINT ( 'NONE',  ( 1.833691583653582535, -145.1092556475513504, -0.3559373310810099444 ) ) ;
#13936 = EDGE_CURVE ( 'NONE', #17335, #20253, #7377, .T. ) ;
#13937 = LINE ( 'NONE', #13118, #8323 ) ;
#13938 = CARTESIAN_POINT ( 'NONE',  ( -23.79223135445719706, 32.40779366744838796, -7.157574570129257907 ) ) ;
#13939 = EDGE_LOOP ( 'NONE', ( #8067, #16577, #27597, #4097 ) ) ;
#13940 = CARTESIAN_POINT ( 'NONE',  ( -1.031422197589711987, -28.14735071801769095, -36.13727897780115939 ) ) ;
#13941 = CONICAL_SURFACE ( 'NONE', #610, 117.6351876552689504, 0.9945805576725580410 ) ;
#13942 = AXIS2_PLACEMENT_3D ( 'NONE', #18385, #7476, #18830 ) ;
#13944 = EDGE_CURVE ( 'NONE', #8900, #26223, #5451, .T. ) ;
#13943 = CARTESIAN_POINT ( 'NONE',  ( -20.20612091757424267, 16.46550228026431384, 24.59769958242370436 ) ) ;
#13945 = CARTESIAN_POINT ( 'NONE',  ( 1.833485406944057594, 132.7804117027888253, 58.53321471326925263 ) ) ;
#13946 = ORIENTED_EDGE ( 'NONE', *, *, #7419, .F. ) ;
#13947 = EDGE_CURVE ( 'NONE', #2039, #17719, #24411, .T. ) ;
#13948 = EDGE_LOOP ( 'NONE', ( #16875, #3830, #1252, #13909 ) ) ;
#13949 = EDGE_LOOP ( 'NONE', ( #16782, #1782, #23342, #13982 ) ) ;
#13950 = CARTESIAN_POINT ( 'NONE',  ( 25.64681081121879203, 84.18689316040048709, 75.24277141833519522 ) ) ;
#13951 = AXIS2_PLACEMENT_3D ( 'NONE', #22635, #25081, #14110 ) ;
#13952 = DIRECTION ( 'NONE',  ( 0.000000000000000000, 0.000000000000000000, 1.000000000000000000 ) ) ;
#13953 = CARTESIAN_POINT ( 'NONE',  ( -20.38016308990357217, 24.94368798801375675, 16.25718651464953624 ) ) ;
#13954 = LINE ( 'NONE', #12097, #26858 ) ;
#13955 = ORIENTED_EDGE ( 'NONE', *, *, #26611, .T. ) ;
#13956 = CARTESIAN_POINT ( 'NONE',  ( 25.65782528836482257, 66.83837989650189115, -91.01210296572875791 ) ) ;
#13957 = CARTESIAN_POINT ( 'NONE',  ( -55.24340739397742794, -0.009386184976284812215, 0.003826481709800012669 ) ) ;
#13958 = LINE ( 'NONE', #25198, #24553 ) ;
#13959 = VERTEX_POINT ( 'NONE', #22394 ) ;
#13960 = B_SPLINE_CURVE_WITH_KNOTS ( 'NONE', 3,
 ( #567, #9364, #15241, #13096 ),
 .UNSPECIFIED., .F., .F.,
 ( 4, 4 ),
 ( 1.906343156168367839E-16, 0.0009910334943225120648 ),
 .UNSPECIFIED. ) ;
#13961 = VERTEX_POINT ( 'NONE', #2660 ) ;
#13962 = CARTESIAN_POINT ( 'NONE',  ( -55.24300891470648622, 0.008142823778062486390, -0.005486913146696510354 ) ) ;
#13963 = CARTESIAN_POINT ( 'NONE',  ( -1.048996300304502194, -36.59642367107725391, 27.53442103413733122 ) ) ;
#13964 = CARTESIAN_POINT ( 'NONE',  ( 1.831572820252009626, -141.7320553118907753, 31.13525033585447233 ) ) ;
#13965 = CARTESIAN_POINT ( 'NONE',  ( 2.108393763691200018, 96.26428731761981794, 108.8265195087752346 ) ) ;
#13966 = CARTESIAN_POINT ( 'NONE',  ( -7.711401346138401891, 6.030154970217631138, 52.11446537925907307 ) ) ;
#13967 = ORIENTED_EDGE ( 'NONE', *, *, #16340, .T. ) ;
#13968 = CARTESIAN_POINT ( 'NONE',  ( -1.019300379054419725, 42.90269154183429379, -16.06793277092006988 ) ) ;
#13969 = DIRECTION ( 'NONE',  ( -1.000000000000000000, -0.000000000000000000, -0.000000000000000000 ) ) ;
#13970 = ADVANCED_FACE ( 'NONE', ( #13454 ), #13863, .F. ) ;
#13971 = EDGE_CURVE ( 'NONE', #17233, #17407, #10592, .T. ) ;
#13972 = B_SPLINE_CURVE_WITH_KNOTS ( 'NONE', 3,
 ( #25840, #20940, #23701, #25569 ),
 .UNSPECIFIED., .F., .F.,
 ( 4, 4 ),
 ( 3.253361034654718625E-16, 0.01077107486149826363 ),
 .UNSPECIFIED. ) ;
#13973 = B_SPLINE_CURVE_WITH_KNOTS ( 'NONE', 3,
 ( #235, #20518, #4840, #15609, #11602, #7438, #9587 ),
 .UNSPECIFIED., .F., .F.,
 ( 4, 3, 4 ),
 ( 0.000000000000000000, 0.02398743853561349088, 0.04000277880656218088 ),
 .UNSPECIFIED. ) ;
#13974 = CARTESIAN_POINT ( 'NONE',  ( -55.24340739397742794, -0.003826481709799693914, -0.009386184976285299672 ) ) ;
#13975 = CARTESIAN_POINT ( 'NONE',  ( 9.884929003653608603, 149.2134106160916076, 19.90991253123297255 ) ) ;
#13976 = CARTESIAN_POINT ( 'NONE',  ( 25.64692232868534560, -107.2834780834837858, 35.20209749635272090 ) ) ;
#13977 = AXIS2_PLACEMENT_3D ( 'NONE', #11891, #22415, #5127 ) ;
#13978 = ORIENTED_EDGE ( 'NONE', *, *, #2868, .T. ) ;
#13980 = ADVANCED_FACE ( 'NONE', ( #16038 ), #26544, .F. ) ;
#13979 = CARTESIAN_POINT ( 'NONE',  ( 25.64681081121879203, -75.24277141833549365, 84.18689316040023130 ) ) ;
#13981 = VERTEX_POINT ( 'NONE', #9144 ) ;
#13982 = ORIENTED_EDGE ( 'NONE', *, *, #3783, .F. ) ;
#13983 = ORIENTED_EDGE ( 'NONE', *, *, #14936, .F. ) ;
#13984 = CARTESIAN_POINT ( 'NONE',  ( 32.73300124599738581, 44.31599526638102304, -108.9684813982483860 ) ) ;
#13985 = CARTESIAN_POINT ( 'NONE',  ( 10.93730112725939030, 136.0306644680981947, 65.95960219663135149 ) ) ;
#13986 = CARTESIAN_POINT ( 'NONE',  ( -55.25297051322618813, 0.002853887643044372355, 0.01466904165775517396 ) ) ;
#13987 = CARTESIAN_POINT ( 'NONE',  ( 109.1721716018069515, 0.009868622090669555702, 0.01392660302850061774 ) ) ;
#13988 = CARTESIAN_POINT ( 'NONE',  ( -20.57838717382308147, -23.26537097894090778, 18.89542499756525729 ) ) ;
#13989 = CARTESIAN_POINT ( 'NONE',  ( -15.02187109954795119, 6.234056423739480657, -45.93032478317444856 ) ) ;
#13990 = CARTESIAN_POINT ( 'NONE',  ( -1.619063947482197729, -16.67502769180532596, 43.26576862488450104 ) ) ;
#13991 = CARTESIAN_POINT ( 'NONE',  ( 25.86096068574579832, 113.0494979885904314, 0.9975172952962499950 ) ) ;
#13992 = CARTESIAN_POINT ( 'NONE',  ( 109.1586900883932856, 0.004851151255037359014, 0.005236795036860563031 ) ) ;
#13993 = CARTESIAN_POINT ( 'NONE',  ( 55.49584447822657296, 42.86099773636619403, -58.53775398922213924 ) ) ;
#13994 = CARTESIAN_POINT ( 'NONE',  ( -23.79223135445719350, 16.82181692922858929, 28.60983116549946814 ) ) ;
#13995 = CARTESIAN_POINT ( 'NONE',  ( -1.155031165708884311, -25.28071330859858534, 38.31525684316168423 ) ) ;
#13996 = CARTESIAN_POINT ( 'NONE',  ( 21.16825799904908223, -23.82367662027909816, 133.3214686481435649 ) ) ;
#13997 = EDGE_CURVE ( 'NONE', #26534, #26705, #25402, .T. ) ;
#13998 = CARTESIAN_POINT ( 'NONE',  ( 25.64681081121879203, 75.86069728268988399, 83.63051021305928145 ) ) ;
#13999 = CARTESIAN_POINT ( 'NONE',  ( 26.11404676487257603, -76.59696442953247697, 83.38016054979757996 ) ) ;
#14000 = B_SPLINE_CURVE_WITH_KNOTS ( 'NONE', 3,
 ( #23378, #18903, #2271, #5954 ),
 .UNSPECIFIED., .F., .F.,
 ( 4, 4 ),
 ( 3.078407974177840223E-16, 0.01077107486149828965 ),
 .UNSPECIFIED. ) ;
#14001 = CARTESIAN_POINT ( 'NONE',  ( 9.884929003653608603, -103.8128997986865159, 109.0134320167729385 ) ) ;
#14002 = CARTESIAN_POINT ( 'NONE',  ( 30.58324630866344407, -117.4177132550299518, 28.99049605145693320 ) ) ;
#14003 = VERTEX_POINT ( 'NONE', #4960 ) ;
#14004 = CARTESIAN_POINT ( 'NONE',  ( -1.239374126674604337, 16.50008610789298302, -42.99367564261284258 ) ) ;
#14005 = ORIENTED_EDGE ( 'NONE', *, *, #3454, .F. ) ;
#14006 = ADVANCED_FACE ( 'NONE', ( #356 ), #4106, .F. ) ;
#14007 = LINE ( 'NONE', #24699, #10693 ) ;
#14008 = ORIENTED_EDGE ( 'NONE', *, *, #4748, .T. ) ;
#14009 = EDGE_CURVE ( 'NONE', #4553, #28186, #15060, .T. ) ;
#14010 = ORIENTED_EDGE ( 'NONE', *, *, #13771, .F. ) ;
#14011 = ORIENTED_EDGE ( 'NONE', *, *, #1806, .T. ) ;
#14012 = B_SPLINE_CURVE_WITH_KNOTS ( 'NONE', 3,
 ( #13132, #15132, #13557, #316, #17589, #26510 ),
 .UNSPECIFIED., .F., .F.,
 ( 4, 2, 4 ),
 ( 0.000000000000000000, 0.0004335184443140231063, 0.0008670368886280462126 ),
 .UNSPECIFIED. ) ;
#14013 = CARTESIAN_POINT ( 'NONE',  ( -55.24271866751342941, -0.006757859501009785483, 0.006671293903667892267 ) ) ;
#14014 = CARTESIAN_POINT ( 'NONE',  ( 2.108393763691210676, 86.43392821214733601, -116.7869873529600540 ) ) ;
#14015 = CARTESIAN_POINT ( 'NONE',  ( 14.74894986621300319, -1.023413983156987147E-16, 2.558534957892467869E-17 ) ) ;
#14016 = B_SPLINE_CURVE_WITH_KNOTS ( 'NONE', 3,
 ( #14679, #23483, #3748, #21305, #1587, #25776, #6068, #10931, #19695, #4581 ),
 .UNSPECIFIED., .F., .F.,
 ( 4, 2, 2, 2, 4 ),
 ( 2.913600445039318278E-16, 0.0003346187017559067080, 0.0006692374035115219826, 0.001003856105267137474, 0.001338474807022752748 ),
 .UNSPECIFIED. ) ;
#14017 = CARTESIAN_POINT ( 'NONE',  ( 32.73300124599732186, 0.000000000000000000, 0.000000000000000000 ) ) ;
#14018 = CARTESIAN_POINT ( 'NONE',  ( 1.833750490713699666, 29.90883416717615262, 141.9939712933756084 ) ) ;
#14019 = CARTESIAN_POINT ( 'NONE',  ( 10.93730112725945425, 115.5857507957700818, 97.44200844886312041 ) ) ;
#14020 = CARTESIAN_POINT ( 'NONE',  ( 1.833691583653535462, -58.69608658929837475, -132.7086741139088133 ) ) ;
#14021 =( BOUNDED_SURFACE ( )  B_SPLINE_SURFACE ( 3, 1, ( 
 ( #5553, #9738 ),
 ( #18792, #16638 ),
 ( #10324, #948 ),
 ( #7735, #18507 ) ),
 .UNSPECIFIED., .F., .F., .F. ) 
 B_SPLINE_SURFACE_WITH_KNOTS ( ( 4, 4 ),
 ( 2, 2 ),
 ( 0.000000000000000000, 1.000000000000000000 ),
 ( 0.000000000000000000, 1.000000000000000000 ),
 .UNSPECIFIED. ) 
 GEOMETRIC_REPRESENTATION_ITEM ( )  RATIONAL_B_SPLINE_SURFACE ( (
 ( 1.000000000000000000, 1.000000000000000000),
 ( 0.9956975270656955868, 0.8568959468854907557),
 ( 0.9956975270656955868, 0.8568959468854907557),
 ( 1.000000000000000000, 1.000000000000000000) ) ) 
 REPRESENTATION_ITEM ( '' )  SURFACE ( )  );
#14022 = CARTESIAN_POINT ( 'NONE',  ( -23.79248802219723302, 33.03370827286732947, -3.207402715357277057 ) ) ;
#14024 = CARTESIAN_POINT ( 'NONE',  ( 2.430230287190581429, -145.5073573687466819, -1.451610819319260726 ) ) ;
#14023 = CARTESIAN_POINT ( 'NONE',  ( -9.156249394959706578, -48.78605533024757079, -24.29252099376471818 ) ) ;
#14025 = CARTESIAN_POINT ( 'NONE',  ( 10.93730112725932635, 0.000000000000000000, 0.000000000000000000 ) ) ;
#14026 = ORIENTED_EDGE ( 'NONE', *, *, #19908, .T. ) ;
#14027 = ORIENTED_EDGE ( 'NONE', *, *, #18156, .F. ) ;
#14028 = CARTESIAN_POINT ( 'NONE',  ( -25.21435515916044423, -16.39063784838720395, 30.48034229288656505 ) ) ;
#14030 = CARTESIAN_POINT ( 'NONE',  ( 109.1589550718174877, -0.004269295012386602368, -0.006257602293694194094 ) ) ;
#14029 = CARTESIAN_POINT ( 'NONE',  ( -55.24271866751342941, 0.009388511352198142604, 0.001425019990782173561 ) ) ;
#14031 = ADVANCED_FACE ( 'NONE', ( #24994 ), #23661, .T. ) ;
#14032 = CARTESIAN_POINT ( 'NONE',  ( 5.340103556456401002, 13.12023871801123498, 146.8647350107029865 ) ) ;
#14033 = B_SPLINE_CURVE_WITH_KNOTS ( 'NONE', 3,
 ( #7659, #18717, #27045, #12103, #16272, #9382, #9811 ),
 .UNSPECIFIED., .F., .F.,
 ( 4, 3, 4 ),
 ( 1.868354362588067661E-17, 0.009512539173626417474, 0.02506242213020845253 ),
 .UNSPECIFIED. ) ;
#14034 = CARTESIAN_POINT ( 'NONE',  ( 30.59138290137886429, -115.2623146671591314, 14.83088430729515217 ) ) ;
#14035 = CARTESIAN_POINT ( 'NONE',  ( -1.058197053496161999, -36.00048521498973031, -28.32422455455065347 ) ) ;
#14036 = ORIENTED_EDGE ( 'NONE', *, *, #7333, .T. ) ;
#14037 = FACE_OUTER_BOUND ( 'NONE', #10322, .T. ) ;
#14038 = CARTESIAN_POINT ( 'NONE',  ( -1.323830074806771506, 46.01435746200691312, 2.318057800980871885 ) ) ;
#14039 = CARTESIAN_POINT ( 'NONE',  ( -1.323830074806762402, -38.58891736138512840, 25.17121255494518550 ) ) ;
#14040 = VERTEX_POINT ( 'NONE', #22832 ) ;
#14041 = CARTESIAN_POINT ( 'NONE',  ( 2.430230287190572103, -142.6294793592099950, 28.83279105684379573 ) ) ;
#14042 = ORIENTED_EDGE ( 'NONE', *, *, #2237, .F. ) ;
#14043 = CARTESIAN_POINT ( 'NONE',  ( 21.16825799904897210, -134.1581724640163600, 18.54093663547782000 ) ) ;
#14044 = CARTESIAN_POINT ( 'NONE',  ( 16.75465622695655910, 10.24707101928041020, 141.8562168210794425 ) ) ;
#14045 = DIRECTION ( 'NONE',  ( -0.5946245182733607137, -0.5955128528260812404, 0.5401723099040858234 ) ) ;
#14046 = EDGE_LOOP ( 'NONE', ( #21349, #16256, #19863, #418 ) ) ;
#14047 = CARTESIAN_POINT ( 'NONE',  ( 6.224689322667647851, -145.3353551538639010, -28.26953958630769037 ) ) ;
#14048 = ORIENTED_EDGE ( 'NONE', *, *, #19086, .T. ) ;
#14049 = CARTESIAN_POINT ( 'NONE',  ( -24.53237795827032741, 29.54731592868594348, 16.68575684089460864 ) ) ;
#14050 = CARTESIAN_POINT ( 'NONE',  ( 16.75465622695653067, -127.9746229614481763, -62.05388459346018948 ) ) ;
#14051 = ORIENTED_EDGE ( 'NONE', *, *, #22603, .T. ) ;
#14052 = SHAPE_DEFINITION_REPRESENTATION ( #19573, #15430 ) ;
#14053 = CARTESIAN_POINT ( 'NONE',  ( -1.323439229708128106, -44.47813215539053999, -12.01475235539429143 ) ) ;
#14054 = CARTESIAN_POINT ( 'NONE',  ( 32.73300124599734318, 113.0038235389602477, 32.68291970228275289 ) ) ;
#14055 = CARTESIAN_POINT ( 'NONE',  ( -9.156249394959713683, 24.29252099376560281, 48.78605533024713026 ) ) ;
#14056 = VERTEX_POINT ( 'NONE', #25123 ) ;
#14057 = ADVANCED_FACE ( 'NONE', ( #16329 ), #2240, .F. ) ;
#14058 = CARTESIAN_POINT ( 'NONE',  ( 26.11404676487257603, 108.0249973236472130, -33.91085499298264239 ) ) ;
#14059 = CARTESIAN_POINT ( 'NONE',  ( 8.186469777910899026, -148.1306754055309511, 19.05650978729151035 ) ) ;
#14060 = CARTESIAN_POINT ( 'NONE',  ( 13.84597867724959208, -124.5889929031784220, -77.45414123936355111 ) ) ;
#14061 = ORIENTED_EDGE ( 'NONE', *, *, #22204, .F. ) ;
#14062 = EDGE_CURVE ( 'NONE', #23391, #22454, #929, .T. ) ;
#14063 = ORIENTED_EDGE ( 'NONE', *, *, #16381, .T. ) ;
#14064 = ORIENTED_EDGE ( 'NONE', *, *, #17194, .T. ) ;
#14065 = DIRECTION ( 'NONE',  ( 1.000000000000000000, -6.938893903907226837E-18, 1.734723475976806709E-18 ) ) ;
#14066 = B_SPLINE_CURVE_WITH_KNOTS ( 'NONE', 3,
 ( #20456, #9528, #18281, #27065, #27649, #5202, #25083, #14113, #25367, #3190 ),
 .UNSPECIFIED., .F., .F.,
 ( 4, 3, 3, 4 ),
 ( 3.404394821604483923E-17, 0.0002669559177086211531, 0.0005339118354151021996, 0.001067817517169162515 ),
 .UNSPECIFIED. ) ;
#14067 = CARTESIAN_POINT ( 'NONE',  ( 109.1586900883932856, 0.007088091345232578992, 0.0008465529156546068058 ) ) ;
#14069 = CARTESIAN_POINT ( 'NONE',  ( 25.64681081121880624, 23.88203588908233499, -110.3564950173079353 ) ) ;
#14068 = LINE ( 'NONE', #24891, #14845 ) ;
#14070 = ADVANCED_FACE ( 'NONE', ( #14158 ), #13688, .F. ) ;
#14071 = CARTESIAN_POINT ( 'NONE',  ( -1.048172774974293064, -43.23017713506512649, 15.11899685083868761 ) ) ;
#14072 = CARTESIAN_POINT ( 'NONE',  ( -20.20612092514784308, -18.30568145913859368, -23.26073121129629939 ) ) ;
#14073 = LINE ( 'NONE', #16680, #15300 ) ;
#14074 = ORIENTED_EDGE ( 'NONE', *, *, #6104, .F. ) ;
#14075 = CARTESIAN_POINT ( 'NONE',  ( 5.340103556456552880, 120.6284720803338217, -84.79482753886428270 ) ) ;
#14076 = CARTESIAN_POINT ( 'NONE',  ( -8.786685647604890903, -37.00619870957905277, 38.68584556812340480 ) ) ;
#14077 = CARTESIAN_POINT ( 'NONE',  ( -1.323439229708132769, 44.47813215539063947, 12.01475235539399300 ) ) ;
#14078 = CARTESIAN_POINT ( 'NONE',  ( 28.37599760073042532, 86.45296943207121387, -75.42809173301522208 ) ) ;
#14079 = CARTESIAN_POINT ( 'NONE',  ( 2.433796855181205476, -1.451562450950653949, 145.5024947199069629 ) ) ;
#14080 = CARTESIAN_POINT ( 'NONE',  ( -7.078251931573400491, 5.101176922830666705, -51.82710018979476274 ) ) ;
#14082 = CARTESIAN_POINT ( 'NONE',  ( 1.832998868059858122, -137.8420662456173034, 45.34898734666001729 ) ) ;
#14081 = B_SPLINE_CURVE_WITH_KNOTS ( 'NONE', 3,
 ( #28327, #17532, #8624, #16373, #11631, #4867, #23017 ),
 .UNSPECIFIED., .F., .F.,
 ( 4, 3, 4 ),
 ( 0.000000000000000000, 0.006568092053401776258, 0.02506242213020846987 ),
 .UNSPECIFIED. ) ;
#14083 = CARTESIAN_POINT ( 'NONE',  ( -20.20700224038492721, 16.58740185276746359, 24.51628800869029234 ) ) ;
#14084 = CARTESIAN_POINT ( 'NONE',  ( 28.43349137099852086, 54.21282462801762847, 111.8014342888385926 ) ) ;
#14085 = VERTEX_POINT ( 'NONE', #10541 ) ;
#14086 = ORIENTED_EDGE ( 'NONE', *, *, #6045, .T. ) ;
#14087 = CARTESIAN_POINT ( 'NONE',  ( -7.733045908741338792, -21.80378472388456501, 47.75066202881817645 ) ) ;
#14088 = CARTESIAN_POINT ( 'NONE',  ( -21.41430102051745266, -29.81033373822133470, -7.777552968935644628 ) ) ;
#14089 = EDGE_CURVE ( 'NONE', #6415, #11326, #4063, .T. ) ;
#14090 = CARTESIAN_POINT ( 'NONE',  ( 55.49584447822657296, 15.34602024131287479, 70.91003759562320852 ) ) ;
#14091 = DIRECTION ( 'NONE',  ( 1.000000000000000000, -6.938893903907226837E-18, 1.734723475976806709E-18 ) ) ;
#14092 = VERTEX_POINT ( 'NONE', #11264 ) ;
#14093 = CARTESIAN_POINT ( 'NONE',  ( -20.57838717382308147, -25.16001208503093522, 16.28767523336148315 ) ) ;
#14094 = CARTESIAN_POINT ( 'NONE',  ( 1.833691583653536128, 45.17974255430996067, -137.8971124741063647 ) ) ;
#14095 = EDGE_CURVE ( 'NONE', #26061, #5381, #9215, .T. ) ;
#14096 = CARTESIAN_POINT ( 'NONE',  ( 2.263178113027037419, -116.7985471375926068, -86.59154384226296486 ) ) ;
#14097 = ORIENTED_EDGE ( 'NONE', *, *, #3094, .T. ) ;
#14098 = EDGE_CURVE ( 'NONE', #17799, #15221, #9249, .T. ) ;
#14099 = ORIENTED_EDGE ( 'NONE', *, *, #21951, .T. ) ;
#14100 = CARTESIAN_POINT ( 'NONE',  ( 2.433796855181219243, -71.49415740225165905, 126.7346379669253622 ) ) ;
#14101 = LINE ( 'NONE', #12106, #26585 ) ;
#14102 = DIRECTION ( 'NONE',  ( -1.000000000000000000, -0.000000000000000000, -0.000000000000000000 ) ) ;
#14103 = CARTESIAN_POINT ( 'NONE',  ( 1.834118845439484335, -107.7186227765460984, 97.22976650547388999 ) ) ;
#14104 = VERTEX_POINT ( 'NONE', #11397 ) ;
#14105 = CARTESIAN_POINT ( 'NONE',  ( -1.113548883309562587, 44.18588492042589166, -12.28732181966532622 ) ) ;
#14106 = CARTESIAN_POINT ( 'NONE',  ( 32.73300124599732186, 0.000000000000000000, 0.000000000000000000 ) ) ;
#14107 = CARTESIAN_POINT ( 'NONE',  ( 109.1589550718174877, 0.007008495014548470070, -0.002874971999843682711 ) ) ;
#14108 = B_SPLINE_CURVE_WITH_KNOTS ( 'NONE', 3,
 ( #7254, #6822, #24683, #15720, #9112, #4934, #22366, #15426 ),
 .UNSPECIFIED., .F., .F.,
 ( 4, 2, 2, 4 ),
 ( 2.194186273941487942E-16, 0.002761568181852859863, 0.005523136363705500283, 0.01104627272741079066 ),
 .UNSPECIFIED. ) ;
#14109 = CARTESIAN_POINT ( 'NONE',  ( -1.056502255334265339, -0.5104472526216820016, 45.80535052436398047 ) ) ;
#14110 = DIRECTION ( 'NONE',  ( 0.000000000000000000, 5.223019709707975211E-21, -1.000000000000000000 ) ) ;
#14111 = CARTESIAN_POINT ( 'NONE',  ( -1.031422197589716205, 43.06660437151330711, 15.60268798220593389 ) ) ;
#14112 = B_SPLINE_CURVE_WITH_KNOTS ( 'NONE', 3,
 ( #25362, #735, #5635, #9523 ),
 .UNSPECIFIED., .F., .F.,
 ( 4, 4 ),
 ( 3.375586461644079052E-16, 0.01077107486149832608 ),
 .UNSPECIFIED. ) ;
#14113 = CARTESIAN_POINT ( 'NONE',  ( 1.833838848569439239, 145.1097630730648120, -0.1779716374162767789 ) ) ;
#14114 = VERTEX_POINT ( 'NONE', #11693 ) ;
#14115 = VERTEX_POINT ( 'NONE', #20173 ) ;
#14116 = EDGE_LOOP ( 'NONE', ( #28476, #8816, #24149, #12948 ) ) ;
#14117 = CARTESIAN_POINT ( 'NONE',  ( 30.59138290137875771, 60.43009393261964135, 99.26509990456028731 ) ) ;
#14118 = ADVANCED_FACE ( 'NONE', ( #7243 ), #3943, .F. ) ;
#14119 = EDGE_CURVE ( 'NONE', #6842, #4463, #609, .T. ) ;
#14120 = CARTESIAN_POINT ( 'NONE',  ( -4.780792508754312387, -18.84172549606840619, 45.80716263181253822 ) ) ;
#14121 = CARTESIAN_POINT ( 'NONE',  ( -1.619063947482197729, -11.94059994246129008, 44.80407745103795492 ) ) ;
#14122 = FACE_OUTER_BOUND ( 'NONE', #27270, .T. ) ;
#14123 = ORIENTED_EDGE ( 'NONE', *, *, #22838, .F. ) ;
#14124 = EDGE_CURVE ( 'NONE', #5185, #195, #20992, .T. ) ;
#14125 = CARTESIAN_POINT ( 'NONE',  ( 25.65782528836481191, 107.5689571161383924, -34.34372400279139725 ) ) ;
#14126 = CARTESIAN_POINT ( 'NONE',  ( 10.93730112725990011, -128.3908183996585990, -79.81734490846054086 ) ) ;
#14127 = LINE ( 'NONE', #27379, #25327 ) ;
#14128 = EDGE_CURVE ( 'NONE', #18960, #27540, #5075, .T. ) ;
#14129 = CARTESIAN_POINT ( 'NONE',  ( -20.24399999263416561, 24.70869149526203401, -16.36687688782867411 ) ) ;
#14130 = CARTESIAN_POINT ( 'NONE',  ( 10.93730112725971004, 51.37919228020272300, 142.1801301103785420 ) ) ;
#14131 = CARTESIAN_POINT ( 'NONE',  ( -1.045287976400365970, -25.66401692419961833, 37.92705037016786918 ) ) ;
#14132 = LINE ( 'NONE', #21196, #17383 ) ;
#14133 = DIRECTION ( 'NONE',  ( -0.7637818620346800147, 0.2198041754873925890, 0.6068965246771022004 ) ) ;
#14134 = CARTESIAN_POINT ( 'NONE',  ( 26.11404676487257603, -112.7148551500681037, 10.71016160607530310 ) ) ;
#14135 = CARTESIAN_POINT ( 'NONE',  ( 1.831572820252009626, 84.49389457294292072, -117.9752562883658555 ) ) ;
#14136 = CARTESIAN_POINT ( 'NONE',  ( 25.64681081121879203, 84.18689316040146764, -75.24277141833410099 ) ) ;
#14137 = ORIENTED_EDGE ( 'NONE', *, *, #26722, .F. ) ;
#14138 = CARTESIAN_POINT ( 'NONE',  ( -55.24300891470648622, 0.002702093572889911754, 0.009439835024157509913 ) ) ;
#14139 = CONICAL_SURFACE ( 'NONE', #353, 117.6351876552689504, 0.9945805576725580410 ) ;
#14140 = ORIENTED_EDGE ( 'NONE', *, *, #15679, .T. ) ;
#14141 = CARTESIAN_POINT ( 'NONE',  ( -55.24271866751342941, -0.001545935011626541761, -0.009369360294294543784 ) ) ;
#14142 = CARTESIAN_POINT ( 'NONE',  ( 119.2224693531408803, -69.99999999999998579, -20.00000000000000355 ) ) ;
#14143 = ORIENTED_EDGE ( 'NONE', *, *, #4713, .T. ) ;
#14144 = ORIENTED_EDGE ( 'NONE', *, *, #19472, .F. ) ;
#14145 = VERTEX_POINT ( 'NONE', #9100 ) ;
#14146 = B_SPLINE_CURVE_WITH_KNOTS ( 'NONE', 3,
 ( #1823, #10075, #23322, #14798, #10491, #16839, #5896 ),
 .UNSPECIFIED., .F., .F.,
 ( 4, 3, 4 ),
 ( 0.000000000000000000, 0.02398743853561349434, 0.04000277880656215312 ),
 .UNSPECIFIED. ) ;
#14147 = ORIENTED_EDGE ( 'NONE', *, *, #7038, .T. ) ;
#14148 = CARTESIAN_POINT ( 'NONE',  ( 109.1778270068192853, 0.007885345421907800564, 0.004958088776550132609 ) ) ;
#14149 = DIRECTION ( 'NONE',  ( 0.5914120900931444380, -0.1754905759872953386, 0.7870418015781028842 ) ) ;
#14150 = EDGE_CURVE ( 'NONE', #8163, #20232, #7860, .T. ) ;
#14151 = CONICAL_SURFACE ( 'NONE', #12782, 117.6351876552689504, 0.9945805576725580410 ) ;
#14152 = CARTESIAN_POINT ( 'NONE',  ( 109.1586900883932856, 0.005236795036868158518, 0.004851151255031872951 ) ) ;
#14153 = CARTESIAN_POINT ( 'NONE',  ( 25.64704443564079739, -66.47548630737917108, 91.26857357624537315 ) ) ;
#14154 = CARTESIAN_POINT ( 'NONE',  ( 28.37644542392842339, -124.2737818798214562, -4.054996728115485283 ) ) ;
#14155 = ADVANCED_FACE ( 'NONE', ( #17861 ), #6901, .F. ) ;
#14156 = CARTESIAN_POINT ( 'NONE',  ( -1.113427685306999759, -1.967672929087495470, -45.82016658690750432 ) ) ;
#14157 = CARTESIAN_POINT ( 'NONE',  ( 1.833485406944057594, -132.7804117027884274, -58.53321471327013370 ) ) ;
#14158 = FACE_OUTER_BOUND ( 'NONE', #6622, .T. ) ;
#14159 = CARTESIAN_POINT ( 'NONE',  ( 1.893872463202043166, -86.08597552418957832, 116.8661275359695679 ) ) ;
#14160 = CARTESIAN_POINT ( 'NONE',  ( 2.108393763691198686, 60.26375949664372200, -132.2055356348356554 ) ) ;
#14161 = FILL_AREA_STYLE_COLOUR ( '', #27164 ) ;
#14162 = VERTEX_POINT ( 'NONE', #23326 ) ;
#14163 = ORIENTED_EDGE ( 'NONE', *, *, #25483, .F. ) ;
#14164 = LINE ( 'NONE', #5544, #16160 ) ;
#14166 = CARTESIAN_POINT ( 'NONE',  ( -1.113548883309539272, 25.34012683631610940, 38.22628252420783213 ) ) ;
#14165 = CARTESIAN_POINT ( 'NONE',  ( -24.53239521893646469, 14.09666242510788337, -30.86654523348667567 ) ) ;
#14167 = CARTESIAN_POINT ( 'NONE',  ( -1.619063947482201282, -16.67502769180592992, -43.26576862488428077 ) ) ;
#14168 = CARTESIAN_POINT ( 'NONE',  ( -5.986830583229461489, 46.64941882410799678, -19.95149887249867859 ) ) ;
#14169 = EDGE_LOOP ( 'NONE', ( #11862, #14757, #19027, #22084, #24175, #17050 ) ) ;
#14170 = ORIENTED_EDGE ( 'NONE', *, *, #1602, .F. ) ;
#14171 = CARTESIAN_POINT ( 'NONE',  ( 1.833603222531969834, 44.41798579679541348, 138.1443021179082677 ) ) ;
#14172 = CARTESIAN_POINT ( 'NONE',  ( -1.045287976400383290, 36.12803364096649972, 28.14015102489766917 ) ) ;
#14173 = CARTESIAN_POINT ( 'NONE',  ( -1.031422197589716205, 25.67058493451498080, 37.93675465142445091 ) ) ;
#14174 = CARTESIAN_POINT ( 'NONE',  ( -25.21435515916043713, -6.169479169075696490, -34.05351380035330777 ) ) ;
#14175 = DIRECTION ( 'NONE',  ( 0.000000000000000000, 0.000000000000000000, 1.000000000000000000 ) ) ;
#14176 = CIRCLE ( 'NONE', #10084, 37.50000000000001421 ) ;
#14177 = CARTESIAN_POINT ( 'NONE',  ( 109.1586900883932856, 0.003481399864227374599, 0.006231977675082119202 ) ) ;
#14178 = VERTEX_POINT ( 'NONE', #21135 ) ;
#14179 = CARTESIAN_POINT ( 'NONE',  ( 26.11404676487257603, -113.2169081140374232, 1.130420376096734847 ) ) ;
#14180 = EDGE_CURVE ( 'NONE', #25022, #22293, #23318, .T. ) ;
#14181 = EDGE_LOOP ( 'NONE', ( #14061, #9156 ) ) ;
#14182 = B_SPLINE_CURVE_WITH_KNOTS ( 'NONE', 3,
 ( #26555, #20216, #6858, #15602 ),
 .UNSPECIFIED., .F., .F.,
 ( 4, 4 ),
 ( 1.906343156168368086E-16, 0.001982023823822943315 ),
 .UNSPECIFIED. ) ;
#14183 =( NAMED_UNIT ( * ) SI_UNIT ( $, .STERADIAN. ) SOLID_ANGLE_UNIT ( ) );
#14184 =( BOUNDED_SURFACE ( )  B_SPLINE_SURFACE ( 3, 1, ( 
 ( #21967, #17641 ),
 ( #8731, #6723 ),
 ( #13315, #21832 ),
 ( #2230, #4694 ) ),
 .UNSPECIFIED., .F., .F., .F. ) 
 B_SPLINE_SURFACE_WITH_KNOTS ( ( 4, 4 ),
 ( 2, 2 ),
 ( 0.000000000000000000, 1.000000000000000000 ),
 ( 0.000000000000000000, 1.000000000000000000 ),
 .UNSPECIFIED. ) 
 GEOMETRIC_REPRESENTATION_ITEM ( )  RATIONAL_B_SPLINE_SURFACE ( (
 ( 1.000000000000000000, 1.000000000000000000),
 ( 0.7789835883360578528, 0.9689951854195403280),
 ( 0.7789835883360578528, 0.9689951854195403280),
 ( 1.000000000000000000, 1.000000000000000000) ) ) 
 REPRESENTATION_ITEM ( '' )  SURFACE ( )  );
#14185 = CARTESIAN_POINT ( 'NONE',  ( -1.058473599757822292, -44.07591602137166831, -12.47539220917846237 ) ) ;
#14186 = ADVANCED_FACE ( 'NONE', ( #6187 ), #3035, .F. ) ;
#14187 = CARTESIAN_POINT ( 'NONE',  ( -1.050231094221219408, 14.39477892760360689, 43.47885872350340009 ) ) ;
#14188 = CARTESIAN_POINT ( 'NONE',  ( 2.430230287190581429, 142.0258656395021717, 31.67257033707551628 ) ) ;
#14189 = EDGE_CURVE ( 'NONE', #1025, #2880, #28409, .T. ) ;
#14190 = ORIENTED_EDGE ( 'NONE', *, *, #25842, .T. ) ;
#14191 = DIRECTION ( 'NONE',  ( -0.7563875759206388771, -0.4122509917856824191, -0.5078650950445610102 ) ) ;
#14193 = CARTESIAN_POINT ( 'NONE',  ( -20.20700224038492721, -27.82980252387826781, -10.08426345511578504 ) ) ;
#14192 = FACE_OUTER_BOUND ( 'NONE', #28465, .T. ) ;
#14194 = CARTESIAN_POINT ( 'NONE',  ( -20.20700224038492721, 23.35150625415659320, -18.19058640100232438 ) ) ;
#14195 = VERTEX_POINT ( 'NONE', #10230 ) ;
#14196 = ORIENTED_EDGE ( 'NONE', *, *, #22872, .T. ) ;
#14197 = ORIENTED_EDGE ( 'NONE', *, *, #2720, .T. ) ;
#14198 = CARTESIAN_POINT ( 'NONE',  ( -1.049819825607596568, 37.34982882986881236, 26.50610175068227292 ) ) ;
#14199 = CARTESIAN_POINT ( 'NONE',  ( 2.433796855181233454, -74.00833731765476386, -125.2830755159761935 ) ) ;
#14200 = DIRECTION ( 'NONE',  ( -0.7071067818211355105, 4.902845705138443504E-18, 0.7071067805519596350 ) ) ;
#14201 = CARTESIAN_POINT ( 'NONE',  ( -1.239374126674604337, -44.48112152129355934, -11.92219841463812280 ) ) ;
#14202 = CARTESIAN_POINT ( 'NONE',  ( 26.11404676487257603, -110.5078194225159223, -24.64483677384961879 ) ) ;
#14203 = CARTESIAN_POINT ( 'NONE',  ( 25.64692232868534560, -83.69035111837253282, 75.79483800045747444 ) ) ;
#14204 = CARTESIAN_POINT ( 'NONE',  ( 10.93730112725932635, 0.000000000000000000, 0.000000000000000000 ) ) ;
#14205 = VERTEX_POINT ( 'NONE', #14932 ) ;
#14206 = CARTESIAN_POINT ( 'NONE',  ( 1.833485406944057594, 145.1085452359073429, -0.5339064996889759662 ) ) ;
#14207 = FACE_OUTER_BOUND ( 'NONE', #19341, .T. ) ;
#14208 = CARTESIAN_POINT ( 'NONE',  ( -1.045287976400365970, 15.59869763335068171, -43.05558670614252037 ) ) ;
#14209 = CARTESIAN_POINT ( 'NONE',  ( 32.73300124599739291, 89.94078864464164269, -75.82012867748392182 ) ) ;
#14210 = CARTESIAN_POINT ( 'NONE',  ( 25.64708010899963853, 107.4019003251856645, 34.83947233573714186 ) ) ;
#14211 = CARTESIAN_POINT ( 'NONE',  ( -20.57838717382308147, -25.16001208503117326, -16.28767523336112433 ) ) ;
#14212 = CARTESIAN_POINT ( 'NONE',  ( 109.1589550718175161, 0.007132058561966984379, -0.002553077953680959675 ) ) ;
#14213 = ORIENTED_EDGE ( 'NONE', *, *, #16759, .T. ) ;
#14214 = CARTESIAN_POINT ( 'NONE',  ( 2.433796855181219243, 28.83182736670734059, -142.6247129145645829 ) ) ;
#14215 = FACE_OUTER_BOUND ( 'NONE', #8944, .T. ) ;
#14216 = CARTESIAN_POINT ( 'NONE',  ( -1.259920593601969729, 12.06711544331625596, 44.39818421957802741 ) ) ;
#14217 = ORIENTED_EDGE ( 'NONE', *, *, #11738, .F. ) ;
#14218 = ADVANCED_FACE ( 'NONE', ( #26025 ), #16961, .T. ) ;
#14219 = ORIENTED_EDGE ( 'NONE', *, *, #23102, .F. ) ;
#14220 = B_SPLINE_CURVE_WITH_KNOTS ( 'NONE', 3,
 ( #28153, #6025, #10210, #27884, #8589, #14780, #16944, #3557 ),
 .UNSPECIFIED., .F., .F.,
 ( 4, 2, 2, 4 ),
 ( 2.225109362706117716E-16, 0.002761568181852862899, 0.005523136363705503753, 0.01104627272741078893 ),
 .UNSPECIFIED. ) ;
#14221 = EDGE_CURVE ( 'NONE', #5798, #18731, #16774, .T. ) ;
#14222 = CARTESIAN_POINT ( 'NONE',  ( -1.049819825607609225, -45.79654196517396514, 0.5097917909113501844 ) ) ;
#14223 = CARTESIAN_POINT ( 'NONE',  ( 109.1586900883932856, 0.002301750759607898694, 0.006757191295056137574 ) ) ;
#14224 = EDGE_LOOP ( 'NONE', ( #9460, #20847, #21350, #16138 ) ) ;
#14225 = CARTESIAN_POINT ( 'NONE',  ( 94.22246935314088034, -90.00000000000005684, -12.50000000000000888 ) ) ;
#14226 =( BOUNDED_SURFACE ( )  B_SPLINE_SURFACE ( 3, 1, ( 
 ( #15462, #23730 ),
 ( #21679, #11168 ),
 ( #4534, #10603 ),
 ( #15176, #10754 ) ),
 .UNSPECIFIED., .F., .F., .F. ) 
 B_SPLINE_SURFACE_WITH_KNOTS ( ( 4, 4 ),
 ( 2, 2 ),
 ( 0.000000000000000000, 1.000000000000000000 ),
 ( 0.000000000000000000, 1.000000000000000000 ),
 .UNSPECIFIED. ) 
 GEOMETRIC_REPRESENTATION_ITEM ( )  RATIONAL_B_SPLINE_SURFACE ( (
 ( 1.000000000000000000, 1.000000000000000000),
 ( 0.9956975270656954757, 0.8568959468854893125),
 ( 0.9956975270656954757, 0.8568959468854893125),
 ( 1.000000000000000000, 1.000000000000000000) ) ) 
 REPRESENTATION_ITEM ( '' )  SURFACE ( )  );
#14227 = CARTESIAN_POINT ( 'NONE',  ( 2.433796855181219243, -116.8607839509062671, 86.69855925933937613 ) ) ;
#14228 = CARTESIAN_POINT ( 'NONE',  ( 26.04756280548354042, 97.45505646068907879, -57.54844730865563918 ) ) ;
#14229 = ORIENTED_EDGE ( 'NONE', *, *, #5270, .T. ) ;
#14230 = CARTESIAN_POINT ( 'NONE',  ( 16.75465622695658041, 102.5353941815402834, 98.56308464785089996 ) ) ;
#14231 = CARTESIAN_POINT ( 'NONE',  ( 26.04756280548352976, 45.01666824410909129, -103.8403168215170922 ) ) ;
#14232 = CARTESIAN_POINT ( 'NONE',  ( 1.833485406944057594, 97.49333871408690300, 107.4794113447412940 ) ) ;
#14233 = CARTESIAN_POINT ( 'NONE',  ( 26.04756280548354752, -45.01666824410835943, 103.8403168215173906 ) ) ;
#14234 = ORIENTED_EDGE ( 'NONE', *, *, #25164, .T. ) ;
#14235 = VERTEX_POINT ( 'NONE', #6315 ) ;
#14236 = CARTESIAN_POINT ( 'NONE',  ( -4.473127245936431073, -18.25038884639838699, 45.82513704981563052 ) ) ;
#14237 = CARTESIAN_POINT ( 'NONE',  ( -55.24300891470650754, 0.008142823778062566187, 0.005486913146700293786 ) ) ;
#14238 = CARTESIAN_POINT ( 'NONE',  ( 1.832998868059890096, 132.7810136645746297, -58.53348008137516700 ) ) ;
#14239 = AXIS2_PLACEMENT_3D ( 'NONE', #19811, #13063, #2242 ) ;
#14240 = CARTESIAN_POINT ( 'NONE',  ( 25.64700659047694487, -83.75695331063684534, -75.72132282458959196 ) ) ;
#14241 = CARTESIAN_POINT ( 'NONE',  ( 180.4657679828686980, 20.00000000000000000, 2.762351802624772237E-15 ) ) ;
#14242 = ORIENTED_EDGE ( 'NONE', *, *, #3882, .F. ) ;
#14243 = CARTESIAN_POINT ( 'NONE',  ( 1.833838848569441016, 59.18404309081362413, 132.4919773286271152 ) ) ;
#14244 = CARTESIAN_POINT ( 'NONE',  ( 1.893872463202054490, 16.11957794552959200, -144.2520230501563958 ) ) ;
#14245 = CARTESIAN_POINT ( 'NONE',  ( 26.11404676487257603, -10.71016160607490875, -112.7148551500681606 ) ) ;
#14246 = B_SPLINE_CURVE_WITH_KNOTS ( 'NONE', 3,
 ( #893, #16149, #3064, #23087, #5357, #20609 ),
 .UNSPECIFIED., .F., .F.,
 ( 4, 2, 4 ),
 ( 1.389302603484999005E-17, 0.0006311571484586006933, 0.001262314296917187509 ),
 .UNSPECIFIED. ) ;
#14247 = B_SPLINE_CURVE_WITH_KNOTS ( 'NONE', 3,
 ( #25266, #9867, #5834, #22830 ),
 .UNSPECIFIED., .F., .F.,
 ( 4, 4 ),
 ( 2.027772282892422897E-16, 0.008383748772659654902 ),
 .UNSPECIFIED. ) ;
#14248 = CARTESIAN_POINT ( 'NONE',  ( 1.831572820252009626, -58.11906524360567516, 132.9644823688593362 ) ) ;
#14249 = ORIENTED_EDGE ( 'NONE', *, *, #28280, .F. ) ;
#14250 = CARTESIAN_POINT ( 'NONE',  ( 25.64700659047697684, -75.72132282458926511, 83.75695331063708693 ) ) ;
#14251 = DIRECTION ( 'NONE',  ( -5.541455922705464902E-20, 5.223019709708320524E-21, -1.000000000000000000 ) ) ;
#14252 = ORIENTED_EDGE ( 'NONE', *, *, #25554, .T. ) ;
#14253 = B_SPLINE_CURVE_WITH_KNOTS ( 'NONE', 3,
 ( #23013, #26875, #18536, #7317, #3279, #9910, #22876 ),
 .UNSPECIFIED., .F., .F.,
 ( 4, 3, 4 ),
 ( 0.000000000000000000, 0.006568092053401830901, 0.02506242213020847681 ),
 .UNSPECIFIED. ) ;
#14254 = ORIENTED_EDGE ( 'NONE', *, *, #21461, .F. ) ;
#14255 = EDGE_CURVE ( 'NONE', #16104, #21261, #18862, .T. ) ;
#14256 = ORIENTED_EDGE ( 'NONE', *, *, #15281, .T. ) ;
#14257 = EDGE_CURVE ( 'NONE', #10864, #7492, #3726, .T. ) ;
#14258 = VECTOR ( 'NONE', #25775, 1000.000000000000114 ) ;
#14259 = VECTOR ( 'NONE', #3447, 1000.000000000000000 ) ;
#14260 = CARTESIAN_POINT ( 'NONE',  ( 55.79472521941428198, -59.28412330436272981, -42.17269936297700639 ) ) ;
#14261 = CARTESIAN_POINT ( 'NONE',  ( 1.832998868059890096, 0.5339089137767937254, -145.1092030902949830 ) ) ;
#14262 = VECTOR ( 'NONE', #2618, 1000.000000000000000 ) ;
#14263 = CARTESIAN_POINT ( 'NONE',  ( -55.24271866751342941, -0.008433070970613520956, -0.004365563123939561994 ) ) ;
#14264 = CARTESIAN_POINT ( 'NONE',  ( -25.21435515916043713, -25.00736669481004526, 23.92354251275963861 ) ) ;
#14265 = CARTESIAN_POINT ( 'NONE',  ( -25.21435515916025594, 1.749597353048488237E-16, -4.373993382621220594E-17 ) ) ;
#14266 = CARTESIAN_POINT ( 'NONE',  ( -1.583189561560256253, 46.33203782964461936, -2.490696082060027017 ) ) ;
#14267 = DIRECTION ( 'NONE',  ( 5.541455922705463698E-20, -5.223019709708320524E-21, 1.000000000000000000 ) ) ;
#14268 = DIRECTION ( 'NONE',  ( 0.7637818620346801257, -0.02150485345383945993, 0.6451161201712183324 ) ) ;
#14269 = CARTESIAN_POINT ( 'NONE',  ( -1.619063947482197729, 38.92136151114943488, 25.20140673341330739 ) ) ;
#14270 = CARTESIAN_POINT ( 'NONE',  ( -22.23342874802668589, 16.78332232459680640, 26.81018246605520972 ) ) ;
#14271 = CARTESIAN_POINT ( 'NONE',  ( 26.11404676487257603, -110.5078194225162918, 24.64483677384812665 ) ) ;
#14272 = CARTESIAN_POINT ( 'NONE',  ( 25.65782528836481191, -55.95807498711414496, -98.07785559018930144 ) ) ;
#14273 = AXIS2_PLACEMENT_3D ( 'NONE', #13832, #22640, #24365 ) ;
#14274 = CARTESIAN_POINT ( 'NONE',  ( -22.23226125620944060, -26.80886670319648246, -16.78323347921907427 ) ) ;
#14275 = CONICAL_SURFACE ( 'NONE', #3718, 117.6351876552689504, 0.9945805576725580410 ) ;
#14276 = CARTESIAN_POINT ( 'NONE',  ( -8.786685647604898008, 38.68584556812353981, 37.00619870957891777 ) ) ;
#14277 = CARTESIAN_POINT ( 'NONE',  ( 30.59141879584286983, -88.14706749784099316, 75.73279557183273880 ) ) ;
#14278 = B_SPLINE_CURVE_WITH_KNOTS ( 'NONE', 3,
 ( #23122, #27412, #3383, #3656, #18331, #7722 ),
 .UNSPECIFIED., .F., .F.,
 ( 4, 2, 4 ),
 ( 8.673617379884035472E-19, 0.0006311636237756757667, 0.001262327247551350666 ),
 .UNSPECIFIED. ) ;
#14279 = LINE ( 'NONE', #7841, #14972 ) ;
#14280 = CARTESIAN_POINT ( 'NONE',  ( 16.05277956358204605, -113.1291064380268665, 87.96830019103622078 ) ) ;
#14281 = CARTESIAN_POINT ( 'NONE',  ( 109.1624594426973260, 0.006914244825461633021, -0.01438905500501229048 ) ) ;
#14282 = ORIENTED_EDGE ( 'NONE', *, *, #24487, .F. ) ;
#14283 = CARTESIAN_POINT ( 'NONE',  ( -28.41354790283022069, 19.47297445639550162, -12.60397206714839413 ) ) ;
#14284 = CONICAL_SURFACE ( 'NONE', #22144, 34.60786435723138510, 0.8559913436420825139 ) ;
#14285 = ADVANCED_FACE ( 'NONE', ( #10369 ), #16099, .T. ) ;
#14286 = ORIENTED_EDGE ( 'NONE', *, *, #23216, .F. ) ;
#14287 = CARTESIAN_POINT ( 'NONE',  ( -1.049819825607599455, 27.33096219556293249, 36.75053263699358297 ) ) ;
#14288 = VERTEX_POINT ( 'NONE', #6047 ) ;
#14289 = EDGE_CURVE ( 'NONE', #3600, #26826, #14802, .T. ) ;
#14290 = ORIENTED_EDGE ( 'NONE', *, *, #6771, .T. ) ;
#14291 = B_SPLINE_CURVE_WITH_KNOTS ( 'NONE', 3,
 ( #22987, #27418, #3248, #20938 ),
 .UNSPECIFIED., .F., .F.,
 ( 4, 4 ),
 ( 1.895855152355442610E-16, 0.001982023823822945917 ),
 .UNSPECIFIED. ) ;
#14292 = ORIENTED_EDGE ( 'NONE', *, *, #13731, .F. ) ;
#14293 = EDGE_CURVE ( 'NONE', #7383, #9793, #22648, .T. ) ;
#14294 = ADVANCED_FACE ( 'NONE', ( #5764 ), #5209, .F. ) ;
#14295 = CARTESIAN_POINT ( 'NONE',  ( 1.834118845439484335, -125.5799175751974985, 72.70910183320523856 ) ) ;
#14296 = VECTOR ( 'NONE', #10679, 1000.000000000000000 ) ;
#14297 = CARTESIAN_POINT ( 'NONE',  ( 25.64681081121880624, -56.81519825470823548, 97.57530875170583329 ) ) ;
#14298 = CARTESIAN_POINT ( 'NONE',  ( -1.019300379054419947, 44.15350047934399669, -12.21833869579480236 ) ) ;
#14299 = AXIS2_PLACEMENT_3D ( 'NONE', #6439, #9586, #2822 ) ;
#14300 = DIRECTION ( 'NONE',  ( 0.5914120900931445490, 0.3206367055789390852, 0.7398809652418038008 ) ) ;
#14301 = CARTESIAN_POINT ( 'NONE',  ( -1.464342487929859660, -2.431462367721655138, -46.14921266389555399 ) ) ;
#14302 = CARTESIAN_POINT ( 'NONE',  ( 25.65782528836480125, 35.44279022896630948, -107.2118488517898101 ) ) ;
#14303 = CARTESIAN_POINT ( 'NONE',  ( 2.433796855181205476, -107.1581411821778858, -98.43889364293970345 ) ) ;
#14304 = CARTESIAN_POINT ( 'NONE',  ( -55.24300891470650754, -0.009812809446892518245, 0.0003472257464213444889 ) ) ;
#14305 = CARTESIAN_POINT ( 'NONE',  ( 109.1586900883932856, 0.0001010081143975987133, 0.007137750914550313082 ) ) ;
#14307 = CARTESIAN_POINT ( 'NONE',  ( -1.050229599974470185, -13.90955673306158147, -43.63650726458059381 ) ) ;
#14306 = CARTESIAN_POINT ( 'NONE',  ( -1.045287976400362417, -44.00138577190658395, -12.68782741917276446 ) ) ;
#14308 = DIRECTION ( 'NONE',  ( 0.000000000000000000, 5.223019709708233256E-21, -1.000000000000000000 ) ) ;
#14309 = ORIENTED_EDGE ( 'NONE', *, *, #7292, .F. ) ;
#14310 = EDGE_LOOP ( 'NONE', ( #28017, #254, #18417, #19932 ) ) ;
#14311 = FACE_OUTER_BOUND ( 'NONE', #17493, .T. ) ;
#14313 = CARTESIAN_POINT ( 'NONE',  ( 2.063896406836609909, 126.4736179849647897, 71.46753739786058190 ) ) ;
#14312 = CARTESIAN_POINT ( 'NONE',  ( -55.24340739397742794, 0.01010924026184123470, -0.0007387096945706978770 ) ) ;
#14314 = CARTESIAN_POINT ( 'NONE',  ( 25.64681081121880624, -23.06870491922396837, 110.5293738517607665 ) ) ;
#14315 = CARTESIAN_POINT ( 'NONE',  ( 25.69398547355842055, 11.06723946918908297, -112.3990349503583985 ) ) ;
#14316 = CARTESIAN_POINT ( 'NONE',  ( -21.41427618760458174, 23.81423075802610967, 19.54551635498102158 ) ) ;
#14317 = EDGE_LOOP ( 'NONE', ( #11113, #27448, #15409, #15520 ) ) ;
#14318 = CARTESIAN_POINT ( 'NONE',  ( 1.832998868059858122, -45.34898734666143838, 137.8420662456168770 ) ) ;
#14319 = EDGE_CURVE ( 'NONE', #12511, #106, #15669, .T. ) ;
#14320 = CARTESIAN_POINT ( 'NONE',  ( 2.430230287190572103, 43.58368230469392302, 138.8342928068221624 ) ) ;
#14321 = CARTESIAN_POINT ( 'NONE',  ( -55.24198130335446422, -0.006617369590168513567, -0.006527480770976002225 ) ) ;
#14322 = VERTEX_POINT ( 'NONE', #13189 ) ;
#14323 = CARTESIAN_POINT ( 'NONE',  ( -55.24728320129491266, 0.008013189884950885564, -0.01214321324516771938 ) ) ;
#14324 = EDGE_CURVE ( 'NONE', #5184, #15977, #26661, .T. ) ;
#14325 = B_SPLINE_CURVE_WITH_KNOTS ( 'NONE', 3,
 ( #2636, #24689, #5078, #26662, #24389, #6690, #2191, #20187, #9119, #22069 ),
 .UNSPECIFIED., .F., .F.,
 ( 4, 3, 3, 4 ),
 ( 3.469446951953614189E-17, 0.0002669559177086212615, 0.0005339118354151003564, 0.001067817517169159696 ),
 .UNSPECIFIED. ) ;
#14326 = CARTESIAN_POINT ( 'NONE',  ( -2.911734481061388990, -46.11606034418772282, -12.03743348210763031 ) ) ;
#14327 = VERTEX_POINT ( 'NONE', #6595 ) ;
#14328 = VECTOR ( 'NONE', #27075, 1000.000000000000114 ) ;
#14329 = EDGE_CURVE ( 'NONE', #19, #21184, #21552, .T. ) ;
#14330 = VERTEX_POINT ( 'NONE', #9164 ) ;
#14331 = CARTESIAN_POINT ( 'NONE',  ( -55.25719721206881729, -0.01115102788682980142, -0.0006290797159206544097 ) ) ;
#14332 = VERTEX_POINT ( 'NONE', #17654 ) ;
#14333 = DIRECTION ( 'NONE',  ( -1.000000000000000000, -0.000000000000000000, -0.000000000000000000 ) ) ;
#14334 = CARTESIAN_POINT ( 'NONE',  ( 2.063896406836609909, 28.88716984836516133, -142.3682421260904789 ) ) ;
#14335 = CARTESIAN_POINT ( 'NONE',  ( 786.9100680686459555, 950.5262624572890218, 1447.888130612201621 ) ) ;
#14336 = CARTESIAN_POINT ( 'NONE',  ( -55.24390624410018802, -0.001451500391950358120, -0.01032895241567008057 ) ) ;
#14338 = AXIS2_PLACEMENT_3D ( 'NONE', #25930, #3903, #21596 ) ;
#14337 = CARTESIAN_POINT ( 'NONE',  ( -25.21435515916043357, -25.00736669481038987, -23.92354251275926558 ) ) ;
#14339 = CARTESIAN_POINT ( 'NONE',  ( -20.20700224038492010, -0.9908225410480588913, -29.58392382092672435 ) ) ;
#14340 = CARTESIAN_POINT ( 'NONE',  ( 109.1589550718174877, 0.001793588804091230705, -0.007359857714023724726 ) ) ;
#14341 = VERTEX_POINT ( 'NONE', #19670 ) ;
#14342 = CIRCLE ( 'NONE', #4237, 53.53553390275978785 ) ;
#14343 = CARTESIAN_POINT ( 'NONE',  ( 2.433796855181205476, -142.0211193075553524, -31.67151202413115385 ) ) ;
#14345 = CARTESIAN_POINT ( 'NONE',  ( 10.93730112725986281, -149.7554878793150408, 20.69552240458288850 ) ) ;
#14344 = CARTESIAN_POINT ( 'NONE',  ( 16.05277956358235159, 109.5668455727257111, 92.36732600443201591 ) ) ;
#14346 = CARTESIAN_POINT ( 'NONE',  ( -1.044557008772713624, 28.22896138707370994, -36.05793264791354602 ) ) ;
#14347 = EDGE_LOOP ( 'NONE', ( #17134, #10028, #27706, #24591 ) ) ;
#14348 = AXIS2_PLACEMENT_3D ( 'NONE', #10297, #20918, #7999 ) ;
#14349 = VERTEX_POINT ( 'NONE', #26434 ) ;
#14350 = ORIENTED_EDGE ( 'NONE', *, *, #9809, .T. ) ;
#14351 = LINE ( 'NONE', #25309, #25432 ) ;
#14353 = CARTESIAN_POINT ( 'NONE',  ( 16.75465622695639212, -131.7467602971413783, 53.58152542127637474 ) ) ;
#14352 = CARTESIAN_POINT ( 'NONE',  ( 1.833838848569429691, 107.7184832843409055, -97.22964245509652415 ) ) ;
#14354 = CARTESIAN_POINT ( 'NONE',  ( -1.045287976400365970, -43.05558670614224326, 15.59869763335140469 ) ) ;
#14355 = CARTESIAN_POINT ( 'NONE',  ( 1.833809397773830785, -132.4918864201824533, -59.18399778167268011 ) ) ;
#14356 = ORIENTED_EDGE ( 'NONE', *, *, #9233, .T. ) ;
#14357 = CARTESIAN_POINT ( 'NONE',  ( -8.786685647604706162, -38.68584556812290032, 37.00619870957955015 ) ) ;
#14358 = CARTESIAN_POINT ( 'NONE',  ( 25.64704443564075476, 46.04703398841431294, -103.0951670221010943 ) ) ;
#14359 = EDGE_LOOP ( 'NONE', ( #11093, #20171, #7994, #8366 ) ) ;
#14360 = CARTESIAN_POINT ( 'NONE',  ( 13.36082413113061307, 142.1654513177095964, -56.35051087434822392 ) ) ;
#14361 = CARTESIAN_POINT ( 'NONE',  ( 25.64681081121880624, -112.2483031020014295, 12.21581276189770904 ) ) ;
#14362 = FACE_OUTER_BOUND ( 'NONE', #13191, .T. ) ;
#14363 = CARTESIAN_POINT ( 'NONE',  ( -1.583189561560252701, 36.01941156322829585, 29.24830400313125978 ) ) ;
#14364 = DIRECTION ( 'NONE',  ( 1.000000000000000000, -6.938893903907226837E-18, 1.734723475976806709E-18 ) ) ;
#14365 = CARTESIAN_POINT ( 'NONE',  ( 25.81918753295379432, -84.61657260023591220, -74.93271318951809690 ) ) ;
#14366 = ADVANCED_FACE ( 'NONE', ( #6737 ), #5976, .F. ) ;
#14367 = ORIENTED_EDGE ( 'NONE', *, *, #17373, .F. ) ;
#14368 = B_SPLINE_CURVE_WITH_KNOTS ( 'NONE', 3,
 ( #554, #19696, #13213, #22004 ),
 .UNSPECIFIED., .F., .F.,
 ( 4, 4 ),
 ( 0.000000000000000000, 0.01077107196513880927 ),
 .UNSPECIFIED. ) ;
#14369 = CARTESIAN_POINT ( 'NONE',  ( -55.24390624410018802, 0.007245494385991918876, 0.007503127514281743120 ) ) ;
#14370 = DIRECTION ( 'NONE',  ( -1.000000000000000000, -0.000000000000000000, -0.000000000000000000 ) ) ;
#14371 = EDGE_CURVE ( 'NONE', #11877, #13127, #26571, .T. ) ;
#14372 = CARTESIAN_POINT ( 'NONE',  ( -55.25297051322618813, 0.006313402748433540913, -0.01354497706059917470 ) ) ;
#14373 = EDGE_CURVE ( 'NONE', #8156, #4782, #5769, .T. ) ;
#14375 =( BOUNDED_SURFACE ( )  B_SPLINE_SURFACE ( 3, 1, ( 
 ( #11208, #13501 ),
 ( #11347, #24615 ),
 ( #11635, #19983 ),
 ( #551, #18102 ) ),
 .UNSPECIFIED., .F., .F., .F. ) 
 B_SPLINE_SURFACE_WITH_KNOTS ( ( 4, 4 ),
 ( 2, 2 ),
 ( 0.000000000000000000, 1.000000000000000000 ),
 ( 0.000000000000000000, 1.000000000000000000 ),
 .UNSPECIFIED. ) 
 GEOMETRIC_REPRESENTATION_ITEM ( )  RATIONAL_B_SPLINE_SURFACE ( (
 ( 1.000000000000000000, 1.000000000000000000),
 ( 0.9593753223639863714, 0.9995975284513187731),
 ( 0.9593753223639863714, 0.9995975284513187731),
 ( 1.000000000000000000, 1.000000000000000000) ) ) 
 REPRESENTATION_ITEM ( '' )  SURFACE ( )  );
#14374 = AXIS2_PLACEMENT_3D ( 'NONE', #4123, #8456, #17353 ) ;
#14376 = ORIENTED_EDGE ( 'NONE', *, *, #5270, .F. ) ;
#14377 = CARTESIAN_POINT ( 'NONE',  ( -1.050230346682696103, 37.05264119692688496, -26.91946103437118509 ) ) ;
#14378 = ORIENTED_EDGE ( 'NONE', *, *, #3783, .T. ) ;
#14379 = VECTOR ( 'NONE', #15610, 1000.000000000000114 ) ;
#14380 = CARTESIAN_POINT ( 'NONE',  ( -1.048994561756806165, -45.79144455904140898, -0.7655149579821828310 ) ) ;
#14381 = CARTESIAN_POINT ( 'NONE',  ( 26.11404676487257603, -57.58742681967381571, -97.48350837663670632 ) ) ;
#14382 = CARTESIAN_POINT ( 'NONE',  ( -21.81686047589431965, -33.92779429964186733, 18.24499610240074432 ) ) ;
#14383 = CARTESIAN_POINT ( 'NONE',  ( -1.045287976400351981, -15.59869763335126436, -43.05558670614231431 ) ) ;
#14384 = CARTESIAN_POINT ( 'NONE',  ( -9.156249394959706578, 48.32878616081010392, -25.18996226954632078 ) ) ;
#14385 = ORIENTED_EDGE ( 'NONE', *, *, #23499, .F. ) ;
#14386 = CARTESIAN_POINT ( 'NONE',  ( 13.84597867724989406, 105.7628030201717877, 101.6650905919613166 ) ) ;
#14387 = B_SPLINE_CURVE_WITH_KNOTS ( 'NONE', 3,
 ( #6761, #28462, #22299, #7051, #15648, #24465, #11483, #2412 ),
 .UNSPECIFIED., .F., .F.,
 ( 4, 2, 2, 4 ),
 ( 2.324173423859648542E-16, 0.002761568181852869404, 0.005523136363705506355, 0.01104627272741079066 ),
 .UNSPECIFIED. ) ;
#14388 = CARTESIAN_POINT ( 'NONE',  ( 1.833809397773857208, -125.5796696653632978, -72.70895493223498818 ) ) ;
#14389 = CARTESIAN_POINT ( 'NONE',  ( 1.894214914920966608, 97.83100278581407849, 107.2270864706593301 ) ) ;
#14390 = CARTESIAN_POINT ( 'NONE',  ( -20.20700224038492721, -18.19058640100206503, 23.35150625415678860 ) ) ;
#14391 = ORIENTED_EDGE ( 'NONE', *, *, #21188, .F. ) ;
#14392 = VERTEX_POINT ( 'NONE', #6452 ) ;
#14393 = CARTESIAN_POINT ( 'NONE',  ( 10.93730112725936188, 148.8212007290658505, 26.59437931460817595 ) ) ;
#14394 = CARTESIAN_POINT ( 'NONE',  ( -4.473127245936431073, -26.34600523034567487, -41.70021447285044047 ) ) ;
#14395 = CARTESIAN_POINT ( 'NONE',  ( 109.1778270068192853, 0.002278716897417739154, 0.009031542838325988531 ) ) ;
#14396 = CARTESIAN_POINT ( 'NONE',  ( -1.259972190295312267, 12.06706380853692551, -44.39825172539698883 ) ) ;
#14397 = CARTESIAN_POINT ( 'NONE',  ( 1.833485406944043827, -84.86072343962486286, -117.7091014914958578 ) ) ;
#14398 = EDGE_CURVE ( 'NONE', #21026, #13718, #24388, .T. ) ;
#14399 = CARTESIAN_POINT ( 'NONE',  ( -1.058197053496163109, 1.754224732379551011, -45.77356582045591438 ) ) ;
#14400 = VERTEX_POINT ( 'NONE', #10908 ) ;
#14401 = CARTESIAN_POINT ( 'NONE',  ( 28.37644542392845537, 95.06674036596312760, -80.14194118792616450 ) ) ;
#14402 = FACE_OUTER_BOUND ( 'NONE', #7155, .T. ) ;
#14403 = AXIS2_PLACEMENT_3D ( 'NONE', #1550, #17748, #14505 ) ;
#14404 = CARTESIAN_POINT ( 'NONE',  ( -20.24399999263414429, -23.20123049637379253, -18.44171895251388094 ) ) ;
#14405 = EDGE_CURVE ( 'NONE', #6724, #14674, #1826, .T. ) ;
#14406 = CARTESIAN_POINT ( 'NONE',  ( 1.832998868059858122, -58.53348008137736258, 132.7810136645736350 ) ) ;
#14407 = LINE ( 'NONE', #10261, #1413 ) ;
#14408 = ORIENTED_EDGE ( 'NONE', *, *, #28081, .T. ) ;
#14409 = DIRECTION ( 'NONE',  ( -1.000000000000000000, -0.000000000000000000, -0.000000000000000000 ) ) ;
#14410 = LINE ( 'NONE', #13436, #24562 ) ;
#14411 = ORIENTED_EDGE ( 'NONE', *, *, #16448, .F. ) ;
#14412 = VERTEX_POINT ( 'NONE', #960 ) ;
#14413 = VECTOR ( 'NONE', #878, 1000.000000000000114 ) ;
#14414 = ORIENTED_EDGE ( 'NONE', *, *, #26157, .T. ) ;
#14415 =( BOUNDED_SURFACE ( )  B_SPLINE_SURFACE ( 3, 1, ( 
 ( #1786, #8853 ),
 ( #17614, #17049 ),
 ( #4512, #10581 ),
 ( #23706, #28221 ) ),
 .UNSPECIFIED., .F., .F., .F. ) 
 B_SPLINE_SURFACE_WITH_KNOTS ( ( 4, 4 ),
 ( 2, 2 ),
 ( 0.000000000000000000, 1.000000000000000000 ),
 ( 0.000000000000000000, 1.000000000000000000 ),
 .UNSPECIFIED. ) 
 GEOMETRIC_REPRESENTATION_ITEM ( )  RATIONAL_B_SPLINE_SURFACE ( (
 ( 1.000000000000000000, 1.000000000000000000),
 ( 0.9934239774497838349, 0.8357310067453913582),
 ( 0.9934239774497838349, 0.8357310067453913582),
 ( 1.000000000000000000, 1.000000000000000000) ) ) 
 REPRESENTATION_ITEM ( '' )  SURFACE ( )  );
#14416 = CARTESIAN_POINT ( 'NONE',  ( 2.433796855181233454, 84.34988187691088513, -118.5671979538048504 ) ) ;
#14417 = CARTESIAN_POINT ( 'NONE',  ( 1.834118845439484335, -0.1779704863060149744, -145.1099497418795750 ) ) ;
#14418 = B_SPLINE_CURVE_WITH_KNOTS ( 'NONE', 3,
 ( #14093, #22470, #4756, #2886, #11663, #7350 ),
 .UNSPECIFIED., .F., .F.,
 ( 4, 2, 4 ),
 ( 0.000000000000000000, 0.0004335151646191496774, 0.0008670303292382993549 ),
 .UNSPECIFIED. ) ;
#14419 = CARTESIAN_POINT ( 'NONE',  ( 99.22246935314079508, -69.99999999999998579, -40.00000000000002132 ) ) ;
#14420 = B_SPLINE_CURVE_WITH_KNOTS ( 'NONE', 3,
 ( #10497, #19265, #19543, #28311, #23890, #28174, #8608, #12914, #12775, #8199 ),
 .UNSPECIFIED., .F., .F.,
 ( 4, 3, 3, 4 ),
 ( 1.387778780781445676E-17, 0.0002669560319015946981, 0.0005492286108966590178, 0.0008315040496093431630 ),
 .UNSPECIFIED. ) ;
#14421 = CARTESIAN_POINT ( 'NONE',  ( -20.21097721650788159, -23.76068422213743503, 17.67178726257384014 ) ) ;
#14422 = EDGE_CURVE ( 'NONE', #15393, #13492, #24866, .T. ) ;
#14423 = CARTESIAN_POINT ( 'NONE',  ( -20.90916690077963835, -38.93431874629077782, -7.054312691028836291 ) ) ;
#14424 = ORIENTED_EDGE ( 'NONE', *, *, #22750, .F. ) ;
#14425 = CARTESIAN_POINT ( 'NONE',  ( 1.833603222531956289, 132.3826570575583048, 59.42758433816011632 ) ) ;
#14426 = CARTESIAN_POINT ( 'NONE',  ( -20.20700224038492010, 16.58740185276710832, -24.51628800869052682 ) ) ;
#14427 = CARTESIAN_POINT ( 'NONE',  ( -20.38016308990357217, 24.94368798801375675, 16.25718651464953624 ) ) ;
#14428 = EDGE_CURVE ( 'NONE', #10456, #1639, #25147, .T. ) ;
#14429 = DIRECTION ( 'NONE',  ( 0.5946245182733608248, -0.4749651461092338489, 0.6487139525627668712 ) ) ;
#14430 = DIRECTION ( 'NONE',  ( -0.5946245182733607137, 0.002950380665384895029, 0.8039981203473693938 ) ) ;
#14431 = CARTESIAN_POINT ( 'NONE',  ( 26.11404676487257603, 110.5078194225161070, 24.64483677384886917 ) ) ;
#14432 = DIRECTION ( 'NONE',  ( -0.5946245182733608248, 0.2456431038754911811, -0.7655593692108981774 ) ) ;
#14433 = EDGE_CURVE ( 'NONE', #17046, #21703, #9891, .T. ) ;
#14434 = DIRECTION ( 'NONE',  ( -0.7563875759206388771, 0.2351350468682910366, 0.6104009704506918599 ) ) ;
#14435 = ADVANCED_FACE ( 'NONE', ( #7304 ), #22897, .F. ) ;
#14436 = LINE ( 'NONE', #16454, #11087 ) ;
#14437 = CARTESIAN_POINT ( 'NONE',  ( 109.1721716018069657, -0.0002019688922674237259, -0.01706748904932341507 ) ) ;
#14438 = FACE_OUTER_BOUND ( 'NONE', #7101, .T. ) ;
#14439 = CARTESIAN_POINT ( 'NONE',  ( 1.833603222531971833, -0.4449221977529563277, 145.1089511853978422 ) ) ;
#14440 = ORIENTED_EDGE ( 'NONE', *, *, #19441, .T. ) ;
#14441 = CARTESIAN_POINT ( 'NONE',  ( -1.619063947482197729, -25.20140673341401438, -38.92136151114898723 ) ) ;
#14442 = ORIENTED_EDGE ( 'NONE', *, *, #18083, .T. ) ;
#14443 = CARTESIAN_POINT ( 'NONE',  ( -20.57838717382308147, 23.26537097894132344, 18.89542499756474569 ) ) ;
#14444 = CARTESIAN_POINT ( 'NONE',  ( 109.1778270068192853, -0.009031542838325997205, 0.002278716897417708363 ) ) ;
#14445 = ORIENTED_EDGE ( 'NONE', *, *, #27521, .F. ) ;
#14446 = ORIENTED_EDGE ( 'NONE', *, *, #24230, .F. ) ;
#14447 = ORIENTED_EDGE ( 'NONE', *, *, #4445, .T. ) ;
#14448 = CARTESIAN_POINT ( 'NONE',  ( 109.1586900883932856, 0.004113747441000919873, 0.005833932871487526248 ) ) ;
#14449 =( BOUNDED_SURFACE ( )  B_SPLINE_SURFACE ( 3, 1, ( 
 ( #8198, #4282 ),
 ( #16964, #17514 ),
 ( #28172, #8340 ),
 ( #17371, #17238 ) ),
 .UNSPECIFIED., .F., .F., .F. ) 
 B_SPLINE_SURFACE_WITH_KNOTS ( ( 4, 4 ),
 ( 2, 2 ),
 ( 0.000000000000000000, 1.000000000000000000 ),
 ( 0.000000000000000000, 1.000000000000000000 ),
 .UNSPECIFIED. ) 
 GEOMETRIC_REPRESENTATION_ITEM ( )  RATIONAL_B_SPLINE_SURFACE ( (
 ( 1.000000000000000000, 1.000000000000000000),
 ( 0.6386103224230302855, 0.9954351624131538845),
 ( 0.6386103224230302855, 0.9954351624131538845),
 ( 1.000000000000000000, 1.000000000000000000) ) ) 
 REPRESENTATION_ITEM ( '' )  SURFACE ( )  );
#14450 = CARTESIAN_POINT ( 'NONE',  ( 1.833485406944043827, -125.9346397303440455, 72.09189602597663793 ) ) ;
#14451 = EDGE_CURVE ( 'NONE', #26705, #26589, #5058, .T. ) ;
#14452 = DIRECTION ( 'NONE',  ( -0.5946245182733608248, -0.2456431038754863239, 0.7655593692108998427 ) ) ;
#14453 = CARTESIAN_POINT ( 'NONE',  ( -1.619063947482197729, 29.22875152547757338, -35.99532424477389725 ) ) ;
#14454 = CARTESIAN_POINT ( 'NONE',  ( 10.93730112725969938, 71.28103789254939215, 133.3192575531800799 ) ) ;
#14455 = LINE ( 'NONE', #25700, #3287 ) ;
#14456 = EDGE_CURVE ( 'NONE', #1896, #7383, #28056, .T. ) ;
#14457 = VERTEX_POINT ( 'NONE', #13756 ) ;
#14458 = ORIENTED_EDGE ( 'NONE', *, *, #15688, .T. ) ;
#14459 = CARTESIAN_POINT ( 'NONE',  ( -1.619063947482197729, -38.92136151114888776, 25.20140673341416360 ) ) ;
#14461 = CARTESIAN_POINT ( 'NONE',  ( 25.98107933586731733, 57.50946808479366723, -97.42660475433878275 ) ) ;
#14460 = LINE ( 'NONE', #21367, #12056 ) ;
#14462 = CARTESIAN_POINT ( 'NONE',  ( 26.11404676487259024, -83.38016054979834735, 76.59696442953165274 ) ) ;
#14463 = CARTESIAN_POINT ( 'NONE',  ( -20.24419206586952313, -16.36655224501349437, 24.70913649113847299 ) ) ;
#14464 = EDGE_CURVE ( 'NONE', #17753, #15393, #17411, .T. ) ;
#14465 = ORIENTED_EDGE ( 'NONE', *, *, #13448, .T. ) ;
#14466 = CARTESIAN_POINT ( 'NONE',  ( 32.73300124599732186, 0.000000000000000000, 0.000000000000000000 ) ) ;
#14467 = LINE ( 'NONE', #19082, #19333 ) ;
#14468 = CARTESIAN_POINT ( 'NONE',  ( -55.24198130335446422, -0.004163123460802295971, -0.008310594958153156783 ) ) ;
#14469 = VERTEX_POINT ( 'NONE', #12047 ) ;
#14470 = CARTESIAN_POINT ( 'NONE',  ( -55.24728320129491266, -0.01453410071985621575, -0.0006547948648749734972 ) ) ;
#14471 = B_SPLINE_CURVE_WITH_KNOTS ( 'NONE', 3,
 ( #12431, #23120, #16776, #25418 ),
 .UNSPECIFIED., .F., .F.,
 ( 4, 4 ),
 ( 0.000000000000000000, 0.01077107196513850396 ),
 .UNSPECIFIED. ) ;
#14472 = DIRECTION ( 'NONE',  ( 0.000000000000000000, 5.223019709707975211E-21, -1.000000000000000000 ) ) ;
#14473 = ORIENTED_EDGE ( 'NONE', *, *, #12468, .T. ) ;
#14474 = EDGE_LOOP ( 'NONE', ( #17116, #19736, #13872, #23500 ) ) ;
#14475 = CARTESIAN_POINT ( 'NONE',  ( -90.83090735639699176, 0.000000000000000000, -37.50000000000001421 ) ) ;
#14476 = EDGE_LOOP ( 'NONE', ( #7703, #15976, #27315, #2985, #12532, #9414 ) ) ;
#14477 = CARTESIAN_POINT ( 'NONE',  ( -1.045287976400362417, -43.05558670614257721, -15.59869763335051651 ) ) ;
#14478 = LINE ( 'NONE', #20821, #6468 ) ;
#14479 = SHAPE_DEFINITION_REPRESENTATION ( #24189, #7571 ) ;
#14480 = LINE ( 'NONE', #6562, #17440 ) ;
#14481 = CARTESIAN_POINT ( 'NONE',  ( -1.045287976400362417, -44.00138577190658395, -12.68782741917276446 ) ) ;
#14482 =( BOUNDED_SURFACE ( )  B_SPLINE_SURFACE ( 3, 1, ( 
 ( #28255, #2059 ),
 ( #26110, #23312 ),
 ( #7921, #3565 ),
 ( #12076, #14360 ) ),
 .UNSPECIFIED., .F., .F., .F. ) 
 B_SPLINE_SURFACE_WITH_KNOTS ( ( 4, 4 ),
 ( 2, 2 ),
 ( 0.000000000000000000, 1.000000000000000000 ),
 ( 0.000000000000000000, 1.000000000000000000 ),
 .UNSPECIFIED. ) 
 GEOMETRIC_REPRESENTATION_ITEM ( )  RATIONAL_B_SPLINE_SURFACE ( (
 ( 1.000000000000000000, 1.000000000000000000),
 ( 0.6386103224230302855, 0.9954351624131538845),
 ( 0.6386103224230302855, 0.9954351624131538845),
 ( 1.000000000000000000, 1.000000000000000000) ) ) 
 REPRESENTATION_ITEM ( '' )  SURFACE ( )  );
#14483 = ADVANCED_FACE ( 'NONE', ( #26994 ), #25819, .F. ) ;
#14484 = CARTESIAN_POINT ( 'NONE',  ( -1.045287976400383290, -44.00138577190632816, 12.68782741917368106 ) ) ;
#14485 = FACE_OUTER_BOUND ( 'NONE', #13522, .T. ) ;
#14486 = CARTESIAN_POINT ( 'NONE',  ( 25.64681081121880624, -46.30456157731397582, 102.9795863647027119 ) ) ;
#14487 = CARTESIAN_POINT ( 'NONE',  ( 2.108985857320889501, -141.8463279126003442, 31.46042399111197696 ) ) ;
#14488 = ADVANCED_FACE ( 'NONE', ( #11760 ), #8923, .F. ) ;
#14489 = VERTEX_POINT ( 'NONE', #20951 ) ;
#14490 = CARTESIAN_POINT ( 'NONE',  ( -25.21435515916025594, 1.749597353048488237E-16, -4.373993382621220594E-17 ) ) ;
#14492 = CARTESIAN_POINT ( 'NONE',  ( -1.050231094221206973, 43.47885872350356351, -14.39477892760314326 ) ) ;
#14491 = CARTESIAN_POINT ( 'NONE',  ( -55.24390624410018802, -0.001451500391952595045, 0.01032895241566660592 ) ) ;
#14493 = CARTESIAN_POINT ( 'NONE',  ( 25.86096068574581608, -102.8701285401538996, -46.89265070732224672 ) ) ;
#14494 = ORIENTED_EDGE ( 'NONE', *, *, #24882, .T. ) ;
#14495 = ADVANCED_FACE ( 'NONE', ( #1239 ), #242, .F. ) ;
#14496 = ORIENTED_EDGE ( 'NONE', *, *, #18888, .T. ) ;
#14497 = EDGE_LOOP ( 'NONE', ( #101, #19587, #27360, #22606 ) ) ;
#14498 = CARTESIAN_POINT ( 'NONE',  ( -1.583189561560256253, 44.83405390829688741, 11.94859433442855412 ) ) ;
#14499 = CARTESIAN_POINT ( 'NONE',  ( 109.1586059443104944, 0.006570129623063769922, 0.002622205828279770140 ) ) ;
#14501 = CARTESIAN_POINT ( 'NONE',  ( -25.21435515916043713, -6.169479169075696490, -34.05351380035330777 ) ) ;
#14500 = CARTESIAN_POINT ( 'NONE',  ( 1.832998868059858122, 144.2584710144582516, -15.69902610990227210 ) ) ;
#14502 = CARTESIAN_POINT ( 'NONE',  ( -55.24390624410018802, 0.004572280736702236288, 0.009374879212970765180 ) ) ;
#14503 = CARTESIAN_POINT ( 'NONE',  ( 55.79472521941426777, 42.17269936297639532, 59.28412330436317745 ) ) ;
#14504 = CARTESIAN_POINT ( 'NONE',  ( 55.79472521941426777, -30.25520714117951471, 66.16469064668288524 ) ) ;
#14506 = EDGE_CURVE ( 'NONE', #28052, #8915, #17062, .T. ) ;
#14505 = DIRECTION ( 'NONE',  ( 0.000000000000000000, 5.223019709707975211E-21, -1.000000000000000000 ) ) ;
#14507 = ORIENTED_EDGE ( 'NONE', *, *, #6034, .T. ) ;
#14508 = CARTESIAN_POINT ( 'NONE',  ( -20.20700224038492721, -29.58392382092674211, -0.9908225410477480288 ) ) ;
#14509 = CARTESIAN_POINT ( 'NONE',  ( -1.239374126674604337, 2.406737988131122830, -45.98822239537607004 ) ) ;
#14510 = CARTESIAN_POINT ( 'NONE',  ( -1.259972190295307382, 44.39825172539712383, 12.06706380853646188 ) ) ;
#14511 = CARTESIAN_POINT ( 'NONE',  ( 10.93730112725972781, -56.95489579269845137, 140.0398180619108359 ) ) ;
#14512 = CARTESIAN_POINT ( 'NONE',  ( 25.64708228042120908, 107.3728320282188662, 34.92896069507321499 ) ) ;
#14513 = CARTESIAN_POINT ( 'NONE',  ( 109.1589550718175161, 0.004269295012381917748, -0.006257602293702372448 ) ) ;
#14514 = CARTESIAN_POINT ( 'NONE',  ( 26.04756280548354042, -84.84709444968852665, -74.90181827458434327 ) ) ;
#14515 = ORIENTED_EDGE ( 'NONE', *, *, #7141, .F. ) ;
#14516 = CARTESIAN_POINT ( 'NONE',  ( -21.81686047589426991, -16.72402253294291796, 34.70276904128906637 ) ) ;
#14517 = CARTESIAN_POINT ( 'NONE',  ( 10.93730112725943471, 125.1380233598475229, 84.82621002473483429 ) ) ;
#14518 = CARTESIAN_POINT ( 'NONE',  ( 109.1778270068192853, 0.0003511581237571051103, -0.009307953841262539552 ) ) ;
#14519 = B_SPLINE_CURVE_WITH_KNOTS ( 'NONE', 3,
 ( #26463, #6766, #411, #4586, #7057, #13650, #700 ),
 .UNSPECIFIED., .F., .F.,
 ( 4, 3, 4 ),
 ( 0.0004157520161273759373, 0.0005492286108966323464, 0.0008315040496093444641 ),
 .UNSPECIFIED. ) ;
#14520 = ORIENTED_EDGE ( 'NONE', *, *, #721, .F. ) ;
#14521 = CARTESIAN_POINT ( 'NONE',  ( -1.113548883309555704, 38.22628252420811634, -25.34012683631568308 ) ) ;
#14522 = ORIENTED_EDGE ( 'NONE', *, *, #26439, .T. ) ;
#14523 = CARTESIAN_POINT ( 'NONE',  ( -1.045287976400365970, -45.76855895860942525, 1.530335034934587002 ) ) ;
#14524 = CARTESIAN_POINT ( 'NONE',  ( 1.831572820252009626, -73.40899645745918178, -125.1738732943817780 ) ) ;
#14525 = CARTESIAN_POINT ( 'NONE',  ( -55.24271866751342941, 0.004365563123939758886, -0.008433070970614048312 ) ) ;
#14526 = CARTESIAN_POINT ( 'NONE',  ( 26.11404676487259024, 107.3263591096435476, -36.06104232266339693 ) ) ;
#14527 = CARTESIAN_POINT ( 'NONE',  ( 1.833809397773815242, -137.9524943416723204, -45.01060836636663254 ) ) ;
#14528 = CARTESIAN_POINT ( 'NONE',  ( 26.11404676487257603, -45.01677474591340911, -103.8885755249573606 ) ) ;
#14529 = ADVANCED_FACE ( 'NONE', ( #14899 ), #3197, .F. ) ;
#14530 = CARTESIAN_POINT ( 'NONE',  ( 1.833721034905629210, -58.69612512971697527, 132.7087680342066278 ) ) ;
#14531 = CARTESIAN_POINT ( 'NONE',  ( -8.786685647604885574, 6.096987947571466530E-17, -1.524246986892866633E-17 ) ) ;
#14532 = DIRECTION ( 'NONE',  ( -0.5946245182733608248, 0.5955128528260846821, -0.5401723099040819376 ) ) ;
#14533 = ORIENTED_EDGE ( 'NONE', *, *, #16210, .F. ) ;
#14534 = EDGE_CURVE ( 'NONE', #6084, #19831, #3354, .T. ) ;
#14535 = ORIENTED_EDGE ( 'NONE', *, *, #24418, .F. ) ;
#14536 =( BOUNDED_SURFACE ( )  B_SPLINE_SURFACE ( 3, 1, ( 
 ( #2091, #21963 ),
 ( #15467, #8881 ),
 ( #17638, #2225 ),
 ( #6433, #10893 ) ),
 .UNSPECIFIED., .F., .F., .F. ) 
 B_SPLINE_SURFACE_WITH_KNOTS ( ( 4, 4 ),
 ( 2, 2 ),
 ( 0.000000000000000000, 1.000000000000000000 ),
 ( 0.000000000000000000, 1.000000000000000000 ),
 .UNSPECIFIED. ) 
 GEOMETRIC_REPRESENTATION_ITEM ( )  RATIONAL_B_SPLINE_SURFACE ( (
 ( 1.000000000000000000, 1.000000000000000000),
 ( 0.9593753223639863714, 0.9995975284513187731),
 ( 0.9593753223639863714, 0.9995975284513187731),
 ( 1.000000000000000000, 1.000000000000000000) ) ) 
 REPRESENTATION_ITEM ( '' )  SURFACE ( )  );
#14537 = VERTEX_POINT ( 'NONE', #21244 ) ;
#14538 = CARTESIAN_POINT ( 'NONE',  ( 25.73574536432414916, -97.42965068311185917, -57.18187897120895968 ) ) ;
#14539 = CARTESIAN_POINT ( 'NONE',  ( -55.24390624410018802, 0.007245494385991918876, 0.007503127514281743120 ) ) ;
#14540 = CARTESIAN_POINT ( 'NONE',  ( -1.619063947482197729, 16.67502769180622835, 43.26576862488415287 ) ) ;
#14541 = CARTESIAN_POINT ( 'NONE',  ( 26.11404676487259024, 24.64483677385001315, -110.5078194225158654 ) ) ;
#14542 = CARTESIAN_POINT ( 'NONE',  ( -20.20700224038492721, -24.51628800869059432, -16.58740185276701951 ) ) ;
#14543 = CARTESIAN_POINT ( 'NONE',  ( -55.24728320129491266, 0.005114031043468944375, -0.01362040845703405695 ) ) ;
#14544 = CARTESIAN_POINT ( 'NONE',  ( 10.93730112726003156, 84.82621002473607064, -125.1380233598471960 ) ) ;
#14545 = VERTEX_POINT ( 'NONE', #14761 ) ;
#14546 = CARTESIAN_POINT ( 'NONE',  ( -20.20700224038492010, 24.51628800869071867, 16.58740185276683832 ) ) ;
#14547 = CARTESIAN_POINT ( 'NONE',  ( 6.224689322667647851, 144.2687111683199817, -33.28770499679192341 ) ) ;
#14548 = CARTESIAN_POINT ( 'NONE',  ( 8.186469777910767576, 90.56875928602713088, 118.7566730872903804 ) ) ;
#14549 = B_SPLINE_CURVE_WITH_KNOTS ( 'NONE', 3,
 ( #684, #9045, #9474, #17801, #16077, #26723 ),
 .UNSPECIFIED., .F., .F.,
 ( 4, 2, 4 ),
 ( 0.000000000000000000, 0.003570751334075638293, 0.007141502668151276587 ),
 .UNSPECIFIED. ) ;
#14550 = CARTESIAN_POINT ( 'NONE',  ( -20.20612092514785019, -24.59769888281546102, -16.46550332780518033 ) ) ;
#14551 =( BOUNDED_SURFACE ( )  B_SPLINE_SURFACE ( 3, 1, ( 
 ( #26636, #14111 ),
 ( #11829, #4775 ),
 ( #20597, #22930 ),
 ( #18435, #20307 ) ),
 .UNSPECIFIED., .F., .F., .F. ) 
 B_SPLINE_SURFACE_WITH_KNOTS ( ( 4, 4 ),
 ( 2, 2 ),
 ( 0.000000000000000000, 1.000000000000000000 ),
 ( 0.000000000000000000, 1.000000000000000000 ),
 .UNSPECIFIED. ) 
 GEOMETRIC_REPRESENTATION_ITEM ( )  RATIONAL_B_SPLINE_SURFACE ( (
 ( 1.000000000000000000, 1.000000000000000000),
 ( 0.9593753223639863714, 0.9995975284513187731),
 ( 0.9593753223639863714, 0.9995975284513187731),
 ( 1.000000000000000000, 1.000000000000000000) ) ) 
 REPRESENTATION_ITEM ( '' )  SURFACE ( )  );
#14552 = CARTESIAN_POINT ( 'NONE',  ( 28.37644542392846247, -122.4011828058665827, 21.87158679436156206 ) ) ;
#14553 = VERTEX_POINT ( 'NONE', #12868 ) ;
#14554 = CARTESIAN_POINT ( 'NONE',  ( 109.1586059443104944, 0.006260042619943050404, 0.003294606663354673979 ) ) ;
#14555 = CARTESIAN_POINT ( 'NONE',  ( 55.49584447822657296, 69.08290406177610521, -22.16497542184333369 ) ) ;
#14556 = ORIENTED_EDGE ( 'NONE', *, *, #27256, .F. ) ;
#14557 = VERTEX_POINT ( 'NONE', #10037 ) ;
#14558 = ORIENTED_EDGE ( 'NONE', *, *, #15988, .T. ) ;
#14559 = CARTESIAN_POINT ( 'NONE',  ( 30.58324630866345117, -28.99049605145642516, -117.4177132550299945 ) ) ;
#14560 = CARTESIAN_POINT ( 'NONE',  ( 2.430230287190589422, -132.3371620660954875, 60.50928654924707217 ) ) ;
#14561 = B_SPLINE_CURVE_WITH_KNOTS ( 'NONE', 3,
 ( #10009, #21355, #15001, #10430, #14589, #23819, #6117 ),
 .UNSPECIFIED., .F., .F.,
 ( 4, 3, 4 ),
 ( 0.000000000000000000, 0.02398743853561351169, 0.04000277880656213925 ),
 .UNSPECIFIED. ) ;
#14562 = CARTESIAN_POINT ( 'NONE',  ( 109.1587776205901861, 0.004965871434398043752, 0.005390665547495595948 ) ) ;
#14563 = EDGE_CURVE ( 'NONE', #27099, #27156, #13270, .T. ) ;
#14564 = B_SPLINE_CURVE_WITH_KNOTS ( 'NONE', 3,
 ( #21040, #10130, #3207, #14572 ),
 .UNSPECIFIED., .F., .F.,
 ( 4, 4 ),
 ( 0.000000000000000000, 0.008383560773332715543 ),
 .UNSPECIFIED. ) ;
#14565 = CARTESIAN_POINT ( 'NONE',  ( 2.430230287190572103, 116.8646894862412182, 86.70145658344696926 ) ) ;
#14566 = EDGE_CURVE ( 'NONE', #23015, #20282, #2310, .T. ) ;
#14567 = DIRECTION ( 'NONE',  ( 0.000000000000000000, 0.000000000000000000, 1.000000000000000000 ) ) ;
#14568 = CARTESIAN_POINT ( 'NONE',  ( -1.113427685306993542, 45.82016658690751854, -1.967672929087340261 ) ) ;
#14569 = B_SPLINE_CURVE_WITH_KNOTS ( 'NONE', 3,
 ( #24573, #12023, #9574, #11876 ),
 .UNSPECIFIED., .F., .F.,
 ( 4, 4 ),
 ( 3.736708725176135323E-17, 0.008383748772659748577 ),
 .UNSPECIFIED. ) ;
#14570 = EDGE_CURVE ( 'NONE', #16169, #23901, #603, .T. ) ;
#14571 = CARTESIAN_POINT ( 'NONE',  ( -1.049819825607581691, 45.79654196517400777, -0.5097917909110309953 ) ) ;
#14572 = CARTESIAN_POINT ( 'NONE',  ( 32.73300124599738581, -32.68291970228155918, -113.0038235389605461 ) ) ;
#14573 = CARTESIAN_POINT ( 'NONE',  ( 25.64704443564076541, -11.93517308299214541, 112.2786464378873035 ) ) ;
#14574 = B_SPLINE_CURVE_WITH_KNOTS ( 'NONE', 3,
 ( #20415, #22890, #14075, #5010 ),
 .UNSPECIFIED., .F., .F.,
 ( 4, 4 ),
 ( 0.000000000000000000, 0.01077107196513892723 ),
 .UNSPECIFIED. ) ;
#14575 = CARTESIAN_POINT ( 'NONE',  ( 55.49584447822657296, -62.96491934285969450, -36.04376091928610037 ) ) ;
#14576 = CARTESIAN_POINT ( 'NONE',  ( -1.155001620486255209, -44.25209926692301110, 12.20337535396725492 ) ) ;
#14577 = CARTESIAN_POINT ( 'NONE',  ( 2.063896406836609909, 133.2511741302120640, 57.85593781835461158 ) ) ;
#14578 = CARTESIAN_POINT ( 'NONE',  ( -23.79248802219730052, 30.42578156345387086, -13.25839849636368584 ) ) ;
#14579 = DIRECTION ( 'NONE',  ( -0.5946245182733607137, 0.8039981203473692828, -0.002950380665387701811 ) ) ;
#14580 = ORIENTED_EDGE ( 'NONE', *, *, #23574, .T. ) ;
#14581 =( BOUNDED_SURFACE ( )  B_SPLINE_SURFACE ( 3, 1, ( 
 ( #12295, #16473 ),
 ( #25267, #24993 ),
 ( #22690, #18328 ),
 ( #27110, #16185 ) ),
 .UNSPECIFIED., .F., .F., .F. ) 
 B_SPLINE_SURFACE_WITH_KNOTS ( ( 4, 4 ),
 ( 2, 2 ),
 ( 0.000000000000000000, 1.000000000000000000 ),
 ( 0.000000000000000000, 1.000000000000000000 ),
 .UNSPECIFIED. ) 
 GEOMETRIC_REPRESENTATION_ITEM ( )  RATIONAL_B_SPLINE_SURFACE ( (
 ( 1.000000000000000000, 1.000000000000000000),
 ( 0.9934239774497837239, 0.8357310067453919133),
 ( 0.9934239774497837239, 0.8357310067453919133),
 ( 1.000000000000000000, 1.000000000000000000) ) ) 
 REPRESENTATION_ITEM ( '' )  SURFACE ( )  );
#14582 = ORIENTED_EDGE ( 'NONE', *, *, #3759, .F. ) ;
#14583 = CARTESIAN_POINT ( 'NONE',  ( 109.1589550718174877, -0.007359857714023708246, -0.001793588804091302696 ) ) ;
#14584 = CARTESIAN_POINT ( 'NONE',  ( 32.73300124599734318, 108.9684813982489118, 44.31599526637995012 ) ) ;
#14585 = VERTEX_POINT ( 'NONE', #10332 ) ;
#14586 = ORIENTED_EDGE ( 'NONE', *, *, #13803, .T. ) ;
#14587 = ORIENTED_EDGE ( 'NONE', *, *, #15674, .T. ) ;
#14588 = EDGE_CURVE ( 'NONE', #25953, #20961, #17057, .T. ) ;
#14589 = CARTESIAN_POINT ( 'NONE',  ( 16.75465622695661594, 91.67104679059893613, 108.7410129416637830 ) ) ;
#14590 = CARTESIAN_POINT ( 'NONE',  ( -20.57838717382308147, 7.715628353033680220, -28.96176188950220975 ) ) ;
#14591 = EDGE_CURVE ( 'NONE', #28326, #437, #7889, .T. ) ;
#14592 = FACE_OUTER_BOUND ( 'NONE', #13293, .T. ) ;
#14593 = DIRECTION ( 'NONE',  ( 0.000000000000000000, -1.000000000000000000, 0.000000000000000000 ) ) ;
#14594 = FACE_OUTER_BOUND ( 'NONE', #26767, .T. ) ;
#14595 = CARTESIAN_POINT ( 'NONE',  ( -20.20700224038492365, 23.35150625415685255, 18.19058640100197977 ) ) ;
#14596 = CARTESIAN_POINT ( 'NONE',  ( -24.53237795827004319, 33.71192251888839309, -3.868415699415555853 ) ) ;
#14597 = CARTESIAN_POINT ( 'NONE',  ( 25.64692232868533139, 56.73833653200244242, 97.62014907493897908 ) ) ;
#14598 = CARTESIAN_POINT ( 'NONE',  ( 1.833809397773915828, 132.6366580004814750, -58.85883548850453906 ) ) ;
#14599 = ORIENTED_EDGE ( 'NONE', *, *, #13597, .F. ) ;
#14600 = ORIENTED_EDGE ( 'NONE', *, *, #14979, .T. ) ;
#14601 = CARTESIAN_POINT ( 'NONE',  ( 109.1589550718175161, 0.003284595046935036983, 0.006826119083824142356 ) ) ;
#14603 = FACE_OUTER_BOUND ( 'NONE', #5285, .T. ) ;
#14602 = CARTESIAN_POINT ( 'NONE',  ( 25.64700659047696618, 112.9110011064639139, 0.2275682798790891748 ) ) ;
#14604 = DIRECTION ( 'NONE',  ( 0.000000000000000000, 5.223019709707975211E-21, -1.000000000000000000 ) ) ;
#14605 = CARTESIAN_POINT ( 'NONE',  ( 109.1589550718175161, 0.007453082872782197839, 0.001354998915253799886 ) ) ;
#14606 = DIRECTION ( 'NONE',  ( -1.000000000000000000, 6.938893903907226837E-18, -1.734723475976806709E-18 ) ) ;
#14607 = ORIENTED_EDGE ( 'NONE', *, *, #15154, .T. ) ;
#14608 = DIRECTION ( 'NONE',  ( -1.000000000000000000, 6.938893903907226837E-18, -1.734723475976806709E-18 ) ) ;
#14609 = FACE_OUTER_BOUND ( 'NONE', #20780, .T. ) ;
#14610 = CARTESIAN_POINT ( 'NONE',  ( 10.93730112725978110, -119.3442956573278479, 92.80059208661636205 ) ) ;
#14611 = ORIENTED_EDGE ( 'NONE', *, *, #18432, .T. ) ;
#14612 = ORIENTED_EDGE ( 'NONE', *, *, #8785, .F. ) ;
#14613 = B_SPLINE_CURVE_WITH_KNOTS ( 'NONE', 3,
 ( #18925, #11872, #27701, #5247 ),
 .UNSPECIFIED., .F., .F.,
 ( 4, 4 ),
 ( 3.344554059698260450E-16, 0.01077107486149801382 ),
 .UNSPECIFIED. ) ;
#14614 = LINE ( 'NONE', #23144, #8462 ) ;
#14615 = ORIENTED_EDGE ( 'NONE', *, *, #20471, .F. ) ;
#14616 = ORIENTED_EDGE ( 'NONE', *, *, #9804, .F. ) ;
#14617 = B_SPLINE_CURVE_WITH_KNOTS ( 'NONE', 3,
 ( #21721, #1992, #21862, #10924 ),
 .UNSPECIFIED., .F., .F.,
 ( 4, 4 ),
 ( 1.636534854170084423E-17, 0.008383748772659484899 ),
 .UNSPECIFIED. ) ;
#14618 =( BOUNDED_SURFACE ( )  B_SPLINE_SURFACE ( 3, 1, ( 
 ( #11659, #15968 ),
 ( #24639, #22763 ),
 ( #4892, #427 ),
 ( #27034, #9368 ) ),
 .UNSPECIFIED., .F., .F., .F. ) 
 B_SPLINE_SURFACE_WITH_KNOTS ( ( 4, 4 ),
 ( 2, 2 ),
 ( 0.000000000000000000, 1.000000000000000000 ),
 ( 0.000000000000000000, 1.000000000000000000 ),
 .UNSPECIFIED. ) 
 GEOMETRIC_REPRESENTATION_ITEM ( )  RATIONAL_B_SPLINE_SURFACE ( (
 ( 1.000000000000000000, 1.000000000000000000),
 ( 0.6386103224230302855, 0.9954351624131538845),
 ( 0.6386103224230302855, 0.9954351624131538845),
 ( 1.000000000000000000, 1.000000000000000000) ) ) 
 REPRESENTATION_ITEM ( '' )  SURFACE ( )  );
#14619 = CARTESIAN_POINT ( 'NONE',  ( 1.833838848569415925, 97.22964245509760417, 107.7184832843399533 ) ) ;
#14620 = EDGE_CURVE ( 'NONE', #12568, #11237, #19165, .T. ) ;
#14621 = EDGE_CURVE ( 'NONE', #6991, #25151, #6779, .T. ) ;
#14622 = VERTEX_POINT ( 'NONE', #6846 ) ;
#14623 = CARTESIAN_POINT ( 'NONE',  ( -16.86833981943426508, 38.94907963570754106, 20.94590537750566028 ) ) ;
#14624 = CONTEXT_DEPENDENT_SHAPE_REPRESENTATION ( #10116, #7204 ) ;
#14625 = CARTESIAN_POINT ( 'NONE',  ( 109.1592201516379674, -0.006536841731953435194, 0.004368284148528988643 ) ) ;
#14626 = CARTESIAN_POINT ( 'NONE',  ( 2.263178607246657315, -118.4461883615809654, -84.32376080825676468 ) ) ;
#14627 = CARTESIAN_POINT ( 'NONE',  ( 25.64692872815575342, 83.69378511050568648, 75.79105864157416761 ) ) ;
#14628 = CARTESIAN_POINT ( 'NONE',  ( 1.833721034905647862, -108.0754384393928120, -96.83259691102610134 ) ) ;
#14629 = ORIENTED_EDGE ( 'NONE', *, *, #18728, .F. ) ;
#14630 = B_SPLINE_CURVE_WITH_KNOTS ( 'NONE', 3,
 ( #11315, #16057, #26561, #9313, #20378, #4698, #5121 ),
 .UNSPECIFIED., .F., .F.,
 ( 4, 3, 4 ),
 ( 9.269414991073849107E-17, 0.009512539173626381045, 0.02506242213020854620 ),
 .UNSPECIFIED. ) ;
#14631 = CARTESIAN_POINT ( 'NONE',  ( -55.24390624410018802, -0.004572280736702649152, 0.009374879212966917563 ) ) ;
#14633 = CARTESIAN_POINT ( 'NONE',  ( 9.884929003653608603, 19.90991253123445404, -149.2134106160914087 ) ) ;
#14632 = CARTESIAN_POINT ( 'NONE',  ( 25.64692232868534560, -97.94691534265392363, -56.17236075412048990 ) ) ;
#14634 = CARTESIAN_POINT ( 'NONE',  ( -20.24419206586951603, -1.282847120831435594, -29.61012937815439372 ) ) ;
#14635 = ORIENTED_EDGE ( 'NONE', *, *, #8143, .F. ) ;
#14636 = ORIENTED_EDGE ( 'NONE', *, *, #19981, .F. ) ;
#14637 = CARTESIAN_POINT ( 'NONE',  ( 25.64681081121879203, 56.09509703373481670, -97.99105938547863559 ) ) ;
#14638 = CARTESIAN_POINT ( 'NONE',  ( -20.20898968516257810, -0.6607166829021660082, -29.59696826051172280 ) ) ;
#14639 = CARTESIAN_POINT ( 'NONE',  ( -20.21097721650787093, 28.26295598655185515, 8.835581399094868615 ) ) ;
#14640 = FACE_OUTER_BOUND ( 'NONE', #24859, .T. ) ;
#14641 = DIRECTION ( 'NONE',  ( 1.000000000000000000, -6.938893903907226837E-18, 1.734723475976806709E-18 ) ) ;
#14642 = VERTEX_POINT ( 'NONE', #24123 ) ;
#14643 = CARTESIAN_POINT ( 'NONE',  ( 2.108393763691158718, 71.53437599919816137, 126.4628696952921416 ) ) ;
#14644 = CARTESIAN_POINT ( 'NONE',  ( -1.155001620486257208, -28.62773628245643209, 35.88346938217584636 ) ) ;
#14645 = ORIENTED_EDGE ( 'NONE', *, *, #26608, .T. ) ;
#14646 = CARTESIAN_POINT ( 'NONE',  ( 25.64703792032472052, -112.2770217641848660, 11.95040607427947776 ) ) ;
#14647 = AXIS2_PLACEMENT_3D ( 'NONE', #1296, #5330, #27637 ) ;
#14648 = CARTESIAN_POINT ( 'NONE',  ( -1.464342487929851222, 44.64187261869797396, 11.94843286121871273 ) ) ;
#14649 = CARTESIAN_POINT ( 'NONE',  ( -22.23226125620943705, 20.31044300692207472, 24.24619897613454000 ) ) ;
#14650 = CARTESIAN_POINT ( 'NONE',  ( -1.619063947482194177, 29.22875152547808852, 35.99532424477347092 ) ) ;
#14651 = ORIENTED_EDGE ( 'NONE', *, *, #18054, .T. ) ;
#14652 = CARTESIAN_POINT ( 'NONE',  ( 9.884929003653626367, 11.54837932063230888, -150.0922431698403727 ) ) ;
#14653 = ADVANCED_FACE ( 'NONE', ( #22244 ), #9077, .F. ) ;
#14654 = CARTESIAN_POINT ( 'NONE',  ( 10.93730112726005999, 136.0306644680993600, -65.95960219662998725 ) ) ;
#14655 = EDGE_CURVE ( 'NONE', #13865, #6991, #24316, .T. ) ;
#14656 = ORIENTED_EDGE ( 'NONE', *, *, #7800, .F. ) ;
#14657 = CARTESIAN_POINT ( 'NONE',  ( 2.433796855181205476, 116.8607839509056561, 86.69855925934011509 ) ) ;
#14658 = B_SPLINE_CURVE_WITH_KNOTS ( 'NONE', 3,
 ( #10169, #27559, #18646, #21076, #7584, #7730, #9879, #1225, #9732, #12030 ),
 .UNSPECIFIED., .F., .F.,
 ( 4, 3, 3, 4 ),
 ( 3.103167691559091397E-17, 0.0002669559177086257068, 0.0005339118354151221489, 0.001067817517169156877 ),
 .UNSPECIFIED. ) ;
#14659 = VERTEX_POINT ( 'NONE', #8569 ) ;
#14660 =( BOUNDED_SURFACE ( )  B_SPLINE_SURFACE ( 3, 1, ( 
 ( #5820, #1481 ),
 ( #17161, #17292 ),
 ( #19312, #23672 ),
 ( #25683, #19598 ) ),
 .UNSPECIFIED., .F., .F., .F. ) 
 B_SPLINE_SURFACE_WITH_KNOTS ( ( 4, 4 ),
 ( 2, 2 ),
 ( 0.000000000000000000, 1.000000000000000000 ),
 ( 0.000000000000000000, 1.000000000000000000 ),
 .UNSPECIFIED. ) 
 GEOMETRIC_REPRESENTATION_ITEM ( )  RATIONAL_B_SPLINE_SURFACE ( (
 ( 1.000000000000000000, 1.000000000000000000),
 ( 0.6386103224230316178, 0.9954351624131538845),
 ( 0.6386103224230316178, 0.9954351624131538845),
 ( 1.000000000000000000, 1.000000000000000000) ) ) 
 REPRESENTATION_ITEM ( '' )  SURFACE ( )  );
#14661 = EDGE_CURVE ( 'NONE', #1690, #15158, #8862, .T. ) ;
#14662 = ORIENTED_EDGE ( 'NONE', *, *, #19741, .F. ) ;
#14663 = CARTESIAN_POINT ( 'NONE',  ( -20.47566262905010603, -7.708089517695397852, -28.85746289809576126 ) ) ;
#14664 = CARTESIAN_POINT ( 'NONE',  ( 2.063896406836609909, -73.79559738457666640, -125.1295119249446941 ) ) ;
#14665 = ADVANCED_FACE ( 'NONE', ( #11158 ), #12019, .F. ) ;
#14666 = CARTESIAN_POINT ( 'NONE',  ( 1.831572820252009626, 108.4969585352555015, 96.36280042115966182 ) ) ;
#14667 = CARTESIAN_POINT ( 'NONE',  ( 25.64692872815579250, -23.79008960806674722, 110.3764733653607237 ) ) ;
#14668 = CARTESIAN_POINT ( 'NONE',  ( 1.834118845439484335, 30.34413640949697921, 141.9019470378988501 ) ) ;
#14669 = CARTESIAN_POINT ( 'NONE',  ( 25.64681081121879203, -0.4157506337735756285, 112.9102952884414464 ) ) ;
#14670 = CARTESIAN_POINT ( 'NONE',  ( -4.473127245936434626, 49.22197550883368677, -3.196405119333975087 ) ) ;
#14671 = CARTESIAN_POINT ( 'NONE',  ( 26.04756280548352976, -74.90181827458404484, 84.84709444968881087 ) ) ;
#14672 = CARTESIAN_POINT ( 'NONE',  ( -1.045287976400365970, 28.14015102489882736, 36.12803364096558312 ) ) ;
#14673 = VERTEX_POINT ( 'NONE', #17763 ) ;
#14674 = VERTEX_POINT ( 'NONE', #26543 ) ;
#14675 = CARTESIAN_POINT ( 'NONE',  ( 109.1778270068192853, -0.004349865064712347094, -0.008236503545664854500 ) ) ;
#14676 = CARTESIAN_POINT ( 'NONE',  ( 21.16825799904903604, -75.99073816868381925, 112.1052598354962271 ) ) ;
#14677 = DIRECTION ( 'NONE',  ( 1.000000000000000000, -6.938893903907226837E-18, 1.734723475976806709E-18 ) ) ;
#14678 = CARTESIAN_POINT ( 'NONE',  ( 2.108393763691175149, 144.3574619851892464, 16.46048390411847606 ) ) ;
#14679 = CARTESIAN_POINT ( 'NONE',  ( -1.045287976400362417, 43.05558670614268379, 15.59869763335023229 ) ) ;
#14680 = CARTESIAN_POINT ( 'NONE',  ( -20.21097721712959228, 23.76068428613707439, 17.67178718142832494 ) ) ;
#14681 = CARTESIAN_POINT ( 'NONE',  ( -1.049817751779888342, 27.33161971822197955, -36.75003908324300994 ) ) ;
#14682 = ORIENTED_EDGE ( 'NONE', *, *, #15033, .F. ) ;
#14683 = CARTESIAN_POINT ( 'NONE',  ( 10.93730112725943471, 119.3442956573271516, 92.80059208661684522 ) ) ;
#14684 = CARTESIAN_POINT ( 'NONE',  ( -1.045287976400362417, -1.530335034933495653, 45.76855895860946788 ) ) ;
#14685 = CARTESIAN_POINT ( 'NONE',  ( 32.73300124599732186, 0.000000000000000000, 0.000000000000000000 ) ) ;
#14686 = CARTESIAN_POINT ( 'NONE',  ( 25.87036335909428075, 0.9898498320587705290, 113.0557711752706922 ) ) ;
#14687 = CARTESIAN_POINT ( 'NONE',  ( 25.64707127832796019, 6.059145946834079367E-17, -112.9112343549835487 ) ) ;
#14688 = VERTEX_POINT ( 'NONE', #21949 ) ;
#14689 = CARTESIAN_POINT ( 'NONE',  ( 1.834118845439484335, 45.01070051384593995, 137.9527673765107068 ) ) ;
#14690 = CARTESIAN_POINT ( 'NONE',  ( 32.73300124599732186, 0.000000000000000000, 0.000000000000000000 ) ) ;
#14691 = ORIENTED_EDGE ( 'NONE', *, *, #19125, .T. ) ;
#14692 = EDGE_CURVE ( 'NONE', #12683, #18593, #23619, .T. ) ;
#14693 = ORIENTED_EDGE ( 'NONE', *, *, #5701, .T. ) ;
#14694 = ORIENTED_EDGE ( 'NONE', *, *, #25789, .T. ) ;
#14695 = EDGE_CURVE ( 'NONE', #27686, #13623, #23958, .T. ) ;
#14696 = CARTESIAN_POINT ( 'NONE',  ( -4.473127245936431073, -26.34600523034567487, -41.70021447285044047 ) ) ;
#14697 = CARTESIAN_POINT ( 'NONE',  ( -55.24728320129491266, -0.01214321324516726489, -0.008013189884950557701 ) ) ;
#14698 = CARTESIAN_POINT ( 'NONE',  ( -20.57838717382308147, 28.96176188950229502, 7.715628353033378239 ) ) ;
#14699 = CARTESIAN_POINT ( 'NONE',  ( -25.21435515916043002, 23.92354251275938992, -25.00736669481030106 ) ) ;
#14700 = ORIENTED_EDGE ( 'NONE', *, *, #24872, .T. ) ;
#14701 = CARTESIAN_POINT ( 'NONE',  ( 1.833485406944043827, 117.7091014914961420, -84.86072343962446496 ) ) ;
#14702 = CARTESIAN_POINT ( 'NONE',  ( 109.1586059443104944, -0.006637156007973997289, -0.002447596125905566588 ) ) ;
#14703 =( BOUNDED_SURFACE ( )  B_SPLINE_SURFACE ( 3, 1, ( 
 ( #3603, #12252 ),
 ( #14107, #5337 ),
 ( #21020, #7811 ),
 ( #3183, #7669 ) ),
 .UNSPECIFIED., .F., .F., .F. ) 
 B_SPLINE_SURFACE_WITH_KNOTS ( ( 4, 4 ),
 ( 2, 2 ),
 ( 0.000000000000000000, 1.000000000000000000 ),
 ( 0.000000000000000000, 1.000000000000000000 ),
 .UNSPECIFIED. ) 
 GEOMETRIC_REPRESENTATION_ITEM ( )  RATIONAL_B_SPLINE_SURFACE ( (
 ( 1.000000000000000000, 1.000000000000000000),
 ( 0.9956975270656954757, 0.8568959468854893125),
 ( 0.9956975270656954757, 0.8568959468854893125),
 ( 1.000000000000000000, 1.000000000000000000) ) ) 
 REPRESENTATION_ITEM ( '' )  SURFACE ( )  );
#14704 = CARTESIAN_POINT ( 'NONE',  ( -1.045287976400362417, -44.00138577190658395, -12.68782741917276446 ) ) ;
#14705 = CARTESIAN_POINT ( 'NONE',  ( 1.832998868059890096, 144.3700883710216942, 14.63705790014057406 ) ) ;
#14706 = CARTESIAN_POINT ( 'NONE',  ( -20.20997486282892552, 1.395963739018065216E-16, 29.60348406988233450 ) ) ;
#14707 = CARTESIAN_POINT ( 'NONE',  ( 1.831572820252008738, 73.40899645746179658, -125.1738732943802290 ) ) ;
#14708 = CARTESIAN_POINT ( 'NONE',  ( 30.59141879584272061, 109.6600586137414126, 38.47120193631498353 ) ) ;
#14709 = CARTESIAN_POINT ( 'NONE',  ( 1.832998868059858122, 132.7810136645738055, 58.53348008137690783 ) ) ;
#14710 = CARTESIAN_POINT ( 'NONE',  ( 109.1587776205901577, -0.001442274045003953805, -0.007186028091163427188 ) ) ;
#14711 = CARTESIAN_POINT ( 'NONE',  ( 26.11404676487257603, 12.95861723607603544, -112.4785329405480780 ) ) ;
#14712 = EDGE_LOOP ( 'NONE', ( #12578, #18404, #18847, #13515 ) ) ;
#14713 = VERTEX_POINT ( 'NONE', #1936 ) ;
#14714 = CARTESIAN_POINT ( 'NONE',  ( 25.64660436782568098, -24.04259444204576113, -110.3216080362390699 ) ) ;
#14715 = CIRCLE ( 'NONE', #2286, 117.6351876552689504 ) ;
#14716 = CARTESIAN_POINT ( 'NONE',  ( 109.1592201516379674, -0.001127733110588171120, -0.007780772729122754396 ) ) ;
#14717 = VERTEX_POINT ( 'NONE', #10742 ) ;
#14718 = EDGE_CURVE ( 'NONE', #12310, #5017, #18396, .T. ) ;
#14719 = VECTOR ( 'NONE', #9534, 1000.000000000000000 ) ;
#14720 = ORIENTED_EDGE ( 'NONE', *, *, #23794, .T. ) ;
#14721 = ORIENTED_EDGE ( 'NONE', *, *, #14534, .F. ) ;
#14722 = EDGE_CURVE ( 'NONE', #3497, #20356, #26406, .T. ) ;
#14723 = ADVANCED_FACE ( 'NONE', ( #19636 ), #14957, .F. ) ;
#14724 = FACE_OUTER_BOUND ( 'NONE', #13393, .T. ) ;
#14725 = B_SPLINE_CURVE_WITH_KNOTS ( 'NONE', 3,
 ( #19294, #6219, #4173, #12949, #21744, #8229 ),
 .UNSPECIFIED., .F., .F.,
 ( 4, 2, 4 ),
 ( 7.372574772901430151E-18, 0.0006311636237756882350, 0.001262327247551369314 ),
 .UNSPECIFIED. ) ;
#14726 = CARTESIAN_POINT ( 'NONE',  ( 1.832998868059890096, -59.50898020732424243, -132.3466930259799881 ) ) ;
#14727 = CARTESIAN_POINT ( 'NONE',  ( -8.786685647604885574, 6.096987947571466530E-17, -1.524246986892866633E-17 ) ) ;
#14728 = CARTESIAN_POINT ( 'NONE',  ( 2.063896406836605024, 116.7302989755737741, 86.47093297169037385 ) ) ;
#14729 = VECTOR ( 'NONE', #10915, 1000.000000000000000 ) ;
#14730 = CARTESIAN_POINT ( 'NONE',  ( -8.786685647604855376, -7.199674155859337787, -53.04920435127184675 ) ) ;
#14731 = CONICAL_SURFACE ( 'NONE', #13812, 117.6351876552689504, 0.9945805576725580410 ) ;
#14732 = B_SPLINE_CURVE_WITH_KNOTS ( 'NONE', 3,
 ( #1809, #8453, #24004, #10759 ),
 .UNSPECIFIED., .F., .F.,
 ( 4, 4 ),
 ( 3.805030037801212946E-16, 0.01077107486149815434 ),
 .UNSPECIFIED. ) ;
#14733 = EDGE_CURVE ( 'NONE', #14040, #18219, #12628, .T. ) ;
#14734 = CARTESIAN_POINT ( 'NONE',  ( 1.832998868059890096, -72.09222286250997058, -125.9352106559991142 ) ) ;
#14735 = CARTESIAN_POINT ( 'NONE',  ( 1.893872463202056045, 59.90695624048866819, -132.2106029832896752 ) ) ;
#14736 = CARTESIAN_POINT ( 'NONE',  ( -20.57838717382308147, -16.28767523336102130, 25.16001208503123365 ) ) ;
#14738 = CIRCLE ( 'NONE', #12434, 80.00000000000000000 ) ;
#14737 =( BOUNDED_SURFACE ( )  B_SPLINE_SURFACE ( 3, 1, ( 
 ( #21903, #13677 ),
 ( #19876, #24081 ),
 ( #24502, #4339 ),
 ( #165, #13117 ) ),
 .UNSPECIFIED., .F., .F., .F. ) 
 B_SPLINE_SURFACE_WITH_KNOTS ( ( 4, 4 ),
 ( 2, 2 ),
 ( 0.000000000000000000, 1.000000000000000000 ),
 ( 0.000000000000000000, 1.000000000000000000 ),
 .UNSPECIFIED. ) 
 GEOMETRIC_REPRESENTATION_ITEM ( )  RATIONAL_B_SPLINE_SURFACE ( (
 ( 1.000000000000000000, 1.000000000000000000),
 ( 0.7789835883360576307, 0.9689951854195403280),
 ( 0.7789835883360576307, 0.9689951854195403280),
 ( 1.000000000000000000, 1.000000000000000000) ) ) 
 REPRESENTATION_ITEM ( '' )  SURFACE ( )  );
#14739 = ORIENTED_EDGE ( 'NONE', *, *, #23080, .F. ) ;
#14740 = VERTEX_POINT ( 'NONE', #22386 ) ;
#14741 = CARTESIAN_POINT ( 'NONE',  ( 25.64692232868534560, -107.4854307433084841, -34.58055111992153741 ) ) ;
#14743 = CARTESIAN_POINT ( 'NONE',  ( 13.36082413113063083, -129.1512766091127276, 81.89226687792040593 ) ) ;
#14742 = CARTESIAN_POINT ( 'NONE',  ( -1.045287976400365970, 28.14015102489882736, 36.12803364096558312 ) ) ;
#14744 = CARTESIAN_POINT ( 'NONE',  ( 0.000000000000000000, 0.000000000000000000, -143.8872038478949946 ) ) ;
#14745 = CARTESIAN_POINT ( 'NONE',  ( 109.1587776205901861, 0.006995903587863974010, 0.002185517590237709071 ) ) ;
#14746 = CARTESIAN_POINT ( 'NONE',  ( 25.64670758986457599, 112.3434365398309893, -11.30712635241874153 ) ) ;
#14747 = ADVANCED_FACE ( 'NONE', ( #20204 ), #17880, .F. ) ;
#14748 = VERTEX_POINT ( 'NONE', #24835 ) ;
#14749 = CARTESIAN_POINT ( 'NONE',  ( 180.4657679828686980, -1.252232817320263489E-15, 3.130582043300658722E-16 ) ) ;
#14750 = CARTESIAN_POINT ( 'NONE',  ( 109.1721716018069657, -0.01550977894512761864, 0.007126480965770868800 ) ) ;
#14751 = CARTESIAN_POINT ( 'NONE',  ( 8.186469777910820866, -84.95702201436492373, 122.8338388711457441 ) ) ;
#14752 = ORIENTED_EDGE ( 'NONE', *, *, #3131, .F. ) ;
#14753 = VERTEX_POINT ( 'NONE', #7409 ) ;
#14754 = EDGE_CURVE ( 'NONE', #15797, #26004, #6008, .T. ) ;
#14756 = CYLINDRICAL_SURFACE ( 'NONE', #6191, 37.50000000000001421 ) ;
#14755 = B_SPLINE_CURVE_WITH_KNOTS ( 'NONE', 3,
 ( #9219, #17976, #578, #18131, #14812, #23472 ),
 .UNSPECIFIED., .F., .F.,
 ( 4, 2, 4 ),
 ( 1.447636874611986795E-16, 0.003570751334075636125, 0.007141502668151127400 ),
 .UNSPECIFIED. ) ;
#14757 = ORIENTED_EDGE ( 'NONE', *, *, #13068, .T. ) ;
#14758 = ORIENTED_EDGE ( 'NONE', *, *, #4041, .F. ) ;
#14759 = AXIS2_PLACEMENT_3D ( 'NONE', #23407, #11882, #3664 ) ;
#14760 = CONICAL_SURFACE ( 'NONE', #12011, 117.6351876552689504, 0.9945805576725580410 ) ;
#14761 = CARTESIAN_POINT ( 'NONE',  ( 26.11404676487257603, 98.61392875273440950, -55.62948129436141897 ) ) ;
#14762 = VECTOR ( 'NONE', #5728, 1000.000000000000227 ) ;
#14763 = VERTEX_POINT ( 'NONE', #3088 ) ;
#14764 = FACE_OUTER_BOUND ( 'NONE', #1640, .T. ) ;
#14765 = CARTESIAN_POINT ( 'NONE',  ( 32.73300124599737160, -117.5726003567929610, 3.836798148478423265 ) ) ;
#14766 = CARTESIAN_POINT ( 'NONE',  ( 10.93730112725977932, -128.3908183996597074, 79.81734490845860819 ) ) ;
#14767 = CARTESIAN_POINT ( 'NONE',  ( -1.045287976400365970, 15.59869763335156101, 43.05558670614217931 ) ) ;
#14768 = CARTESIAN_POINT ( 'NONE',  ( 13.36082413113063083, -119.8836995922732882, 94.94363694444014357 ) ) ;
#14769 = CARTESIAN_POINT ( 'NONE',  ( 1.833206310202320610, -141.7818020564280630, 30.89799345102914074 ) ) ;
#14770 = B_SPLINE_CURVE_WITH_KNOTS ( 'NONE', 3,
 ( #18463, #12273, #18899, #27231 ),
 .UNSPECIFIED., .F., .F.,
 ( 4, 4 ),
 ( 5.049803577358454571E-16, 0.008383748772659955009 ),
 .UNSPECIFIED. ) ;
#14771 = B_SPLINE_CURVE_WITH_KNOTS ( 'NONE', 3,
 ( #9152, #24145, #21692, #19529, #24428, #19953, #15190, #13466, #10899, #21970 ),
 .UNSPECIFIED., .F., .F.,
 ( 4, 3, 3, 4 ),
 ( 3.469446951953614189E-17, 0.0002669559177086352477, 0.0005339118354151166194, 0.001067817517169169887 ),
 .UNSPECIFIED. ) ;
#14772 = CARTESIAN_POINT ( 'NONE',  ( 10.93730112725932635, 0.000000000000000000, 0.000000000000000000 ) ) ;
#14774 = CARTESIAN_POINT ( 'NONE',  ( 25.87036335909423812, -10.83311869338149869, 112.5399073133628320 ) ) ;
#14773 = CARTESIAN_POINT ( 'NONE',  ( 25.64708228042119487, -97.76433875577606614, -56.48974615489026974 ) ) ;
#14775 = CARTESIAN_POINT ( 'NONE',  ( 55.79472521941426777, -8.328398066092255192, 72.27573336313948005 ) ) ;
#14776 = VERTEX_POINT ( 'NONE', #26964 ) ;
#14777 = VERTEX_POINT ( 'NONE', #11865 ) ;
#14778 = CARTESIAN_POINT ( 'NONE',  ( -12.82751273423881599, 8.715310691360238948, -48.09651489336683738 ) ) ;
#14779 = CARTESIAN_POINT ( 'NONE',  ( 2.433796855181233454, 118.5671979538056888, 84.34988187690970562 ) ) ;
#14780 = CARTESIAN_POINT ( 'NONE',  ( -6.588769196390765970, -50.13301368233292976, 11.07780292579747083 ) ) ;
#14781 = AXIS2_PLACEMENT_3D ( 'NONE', #18203, #3665, #6135 ) ;
#14782 = CARTESIAN_POINT ( 'NONE',  ( -25.21435515916025594, 1.749597353048488237E-16, -4.373993382621220594E-17 ) ) ;
#14783 = DIRECTION ( 'NONE',  ( 0.5946245182733607137, 0.6948076064830630560, 0.4045541647807504582 ) ) ;
#14784 = ORIENTED_EDGE ( 'NONE', *, *, #7280, .T. ) ;
#14785 = CARTESIAN_POINT ( 'NONE',  ( 55.79472521941428198, -0.7279028900788538925, -72.75035398477137960 ) ) ;
#14786 = CARTESIAN_POINT ( 'NONE',  ( 109.1586059443104944, -0.006344953511164451443, -0.003127959656212844081 ) ) ;
#14787 = ADVANCED_FACE ( 'NONE', ( #15900 ), #20861, .F. ) ;
#14788 = ORIENTED_EDGE ( 'NONE', *, *, #22131, .T. ) ;
#14789 = CARTESIAN_POINT ( 'NONE',  ( -1.056502255334264895, 14.64009593116162478, 43.40574022158757828 ) ) ;
#14790 = CIRCLE ( 'NONE', #14299, 151.1787379149930359 ) ;
#14791 = FACE_OUTER_BOUND ( 'NONE', #21811, .T. ) ;
#14792 = ADVANCED_FACE ( 'NONE', ( #5382 ), #23814, .F. ) ;
#14793 = CARTESIAN_POINT ( 'NONE',  ( 25.86096068574579121, 74.90357932134628527, 84.67961880569320954 ) ) ;
#14794 = CARTESIAN_POINT ( 'NONE',  ( -7.078251931573400491, -38.93060825814254144, -34.59014398252902112 ) ) ;
#14795 = CARTESIAN_POINT ( 'NONE',  ( 25.69398547355839568, -55.82723250638839119, 98.18017599249827754 ) ) ;
#14797 = ORIENTED_EDGE ( 'NONE', *, *, #7729, .F. ) ;
#14796 = EDGE_CURVE ( 'NONE', #3608, #7265, #9858, .T. ) ;
#14798 = CARTESIAN_POINT ( 'NONE',  ( 19.66333377628708945, -33.01772659807196675, 133.7337774474998469 ) ) ;
#14799 =( BOUNDED_SURFACE ( )  B_SPLINE_SURFACE ( 3, 1, ( 
 ( #8025, #14320 ),
 ( #8154, #3528 ),
 ( #14750, #5409 ),
 ( #7590, #7880 ) ),
 .UNSPECIFIED., .F., .F., .F. ) 
 B_SPLINE_SURFACE_WITH_KNOTS ( ( 4, 4 ),
 ( 2, 2 ),
 ( 0.000000000000000000, 1.000000000000000000 ),
 ( 0.000000000000000000, 1.000000000000000000 ),
 .UNSPECIFIED. ) 
 GEOMETRIC_REPRESENTATION_ITEM ( )  RATIONAL_B_SPLINE_SURFACE ( (
 ( 1.000000000000000000, 1.000000000000000000),
 ( 0.6386103224230302855, 0.9954351624131538845),
 ( 0.6386103224230302855, 0.9954351624131538845),
 ( 1.000000000000000000, 1.000000000000000000) ) ) 
 REPRESENTATION_ITEM ( '' )  SURFACE ( )  );
#14800 = DIRECTION ( 'NONE',  ( -0.7563875759206388771, -0.6104009704506927481, 0.2351350468682887607 ) ) ;
#14801 = EDGE_LOOP ( 'NONE', ( #22308, #7526, #27535, #4302 ) ) ;
#14802 = LINE ( 'NONE', #21701, #7850 ) ;
#14803 = CARTESIAN_POINT ( 'NONE',  ( -10.86508079875780552, -6.877801422380434460, 50.67624451685642839 ) ) ;
#14804 = CARTESIAN_POINT ( 'NONE',  ( -28.41354790283022069, -18.00456980371910376, -14.62505768302794529 ) ) ;
#14805 = AXIS2_PLACEMENT_3D ( 'NONE', #2816, #12170, #5112 ) ;
#14806 = CARTESIAN_POINT ( 'NONE',  ( 1.832998868059890096, 29.64765804470269472, -142.0492247521719946 ) ) ;
#14807 = CARTESIAN_POINT ( 'NONE',  ( -1.050229599974468409, -14.39582765040431944, 43.47850826583067629 ) ) ;
#14808 = AXIS2_PLACEMENT_3D ( 'NONE', #10412, #7982, #14567 ) ;
#14809 = CARTESIAN_POINT ( 'NONE',  ( -20.20612091757425688, 18.30568244821375501, -23.26073043121635919 ) ) ;
#14810 = CARTESIAN_POINT ( 'NONE',  ( 1.833838850855473712, 138.0350826608193699, -44.75675607098784781 ) ) ;
#14811 = CARTESIAN_POINT ( 'NONE',  ( 109.1587776205901861, -0.006944419901758113779, 0.002343968083398812255 ) ) ;
#14812 = CARTESIAN_POINT ( 'NONE',  ( -24.53237795827032031, 14.09663893005633284, 30.86653739599985968 ) ) ;
#14813 = DIRECTION ( 'NONE',  ( 0.000000000000000000, -1.000000000000000000, 0.000000000000000000 ) ) ;
#14814 = CARTESIAN_POINT ( 'NONE',  ( 25.64700659047694131, 35.10784848926805779, -107.3144208978481515 ) ) ;
#14815 = ORIENTED_EDGE ( 'NONE', *, *, #17158, .T. ) ;
#14816 = EDGE_CURVE ( 'NONE', #14114, #6438, #956, .T. ) ;
#14817 = ORIENTED_EDGE ( 'NONE', *, *, #22531, .F. ) ;
#14818 = CARTESIAN_POINT ( 'NONE',  ( -1.619063947482194177, 29.22875152547808852, 35.99532424477347092 ) ) ;
#14819 = CARTESIAN_POINT ( 'NONE',  ( -1.155031165708876317, 16.13806347973058664, 42.97366960678581194 ) ) ;
#14820 = CARTESIAN_POINT ( 'NONE',  ( -8.786685647604890903, 38.68584556812300690, -37.00619870957947910 ) ) ;
#14821 = CARTESIAN_POINT ( 'NONE',  ( 25.64692232868534560, -84.12764974007976093, -75.30916867847187746 ) ) ;
#14822 = CARTESIAN_POINT ( 'NONE',  ( 32.73300124599740002, 116.5274707358857142, -16.10546300444702794 ) ) ;
#14823 = CARTESIAN_POINT ( 'NONE',  ( 1.834118845439484335, -141.9019470378985659, -30.34413640949841096 ) ) ;
#14824 = CARTESIAN_POINT ( 'NONE',  ( -1.046936909428678675, 25.87632113675161349, -37.78538189376516954 ) ) ;
#14825 = ORIENTED_EDGE ( 'NONE', *, *, #18431, .T. ) ;
#14826 = CARTESIAN_POINT ( 'NONE',  ( 1.833750490713730752, -144.3424379351781397, 14.90257883162705532 ) ) ;
#14827 = CYLINDRICAL_SURFACE ( 'NONE', #26708, 20.00000000000000000 ) ;
#14828 = EDGE_CURVE ( 'NONE', #26408, #15445, #9198, .T. ) ;
#14829 = CARTESIAN_POINT ( 'NONE',  ( 1.834118845439484335, 15.34511559672683489, 144.2964192726482793 ) ) ;
#14830 = CIRCLE ( 'NONE', #17132, 151.1787379149930359 ) ;
#14831 = CARTESIAN_POINT ( 'NONE',  ( 25.64670758986459731, 65.96397693491162784, 91.63870681572846877 ) ) ;
#14832 = ADVANCED_FACE ( 'NONE', ( #11577 ), #643, .T. ) ;
#14833 = VECTOR ( 'NONE', #6899, 1000.000000000000227 ) ;
#14834 = ORIENTED_EDGE ( 'NONE', *, *, #23282, .T. ) ;
#14835 = CARTESIAN_POINT ( 'NONE',  ( 25.64708228042118776, -45.96113332231410453, 103.1335618347710295 ) ) ;
#14836 = CARTESIAN_POINT ( 'NONE',  ( -8.786685647604890903, -9.545808661480235102, 52.67761315067295413 ) ) ;
#14837 = ORIENTED_EDGE ( 'NONE', *, *, #9501, .F. ) ;
#14838 = ORIENTED_EDGE ( 'NONE', *, *, #20722, .F. ) ;
#14839 = ORIENTED_EDGE ( 'NONE', *, *, #23556, .T. ) ;
#14840 = CARTESIAN_POINT ( 'NONE',  ( 1.893872463202069145, 29.24569695044243645, 142.1730500379299826 ) ) ;
#14841 = CIRCLE ( 'NONE', #26339, 151.1787379149930359 ) ;
#14842 = CARTESIAN_POINT ( 'NONE',  ( 109.1589550718174877, 0.007571935245604908930, 0.0002241941239240737905 ) ) ;
#14843 = AXIS2_PLACEMENT_3D ( 'NONE', #8465, #21548, #4268 ) ;
#14844 = LINE ( 'NONE', #3621, #516 ) ;
#14845 = VECTOR ( 'NONE', #14200, 1000.000000000000114 ) ;
#14846 = CIRCLE ( 'NONE', #9820, 20.00000000000000000 ) ;
#14847 = CARTESIAN_POINT ( 'NONE',  ( 10.93730112725972425, -42.00474393596362432, 145.2260730187398678 ) ) ;
#14848 = ORIENTED_EDGE ( 'NONE', *, *, #17573, .T. ) ;
#14849 = CARTESIAN_POINT ( 'NONE',  ( 109.1592201516379674, 0.006044422199831473233, 0.005027640251764405217 ) ) ;
#14850 = EDGE_CURVE ( 'NONE', #3600, #19910, #21195, .T. ) ;
#14851 = B_SPLINE_CURVE_WITH_KNOTS ( 'NONE', 3,
 ( #1740, #10539, #23928, #21183, #6356, #10408, #21329 ),
 .UNSPECIFIED., .F., .F.,
 ( 4, 3, 4 ),
 ( 0.000000000000000000, 0.02398743853561430966, 0.04000277880656213925 ),
 .UNSPECIFIED. ) ;
#14852 = CARTESIAN_POINT ( 'NONE',  ( 1.833838848569426805, 58.85887272891370259, -132.6367525013571367 ) ) ;
#14853 = CARTESIAN_POINT ( 'NONE',  ( 6.224689322667630975, -108.2965163446067152, -100.9623537450662809 ) ) ;
#14854 = EDGE_CURVE ( 'NONE', #21976, #21463, #20210, .T. ) ;
#14855 = CARTESIAN_POINT ( 'NONE',  ( 2.433796855181205476, -138.8296532063090751, 43.58222566461595449 ) ) ;
#14856 = CARTESIAN_POINT ( 'NONE',  ( 1.833750490713697223, 97.29556423840286072, -107.6587173638736630 ) ) ;
#14857 = CARTESIAN_POINT ( 'NONE',  ( 30.59138290137919469, 99.26509990456105470, -60.43009393261889528 ) ) ;
#14858 = ADVANCED_FACE ( 'NONE', ( #11542 ), #26710, .F. ) ;
#14859 = CARTESIAN_POINT ( 'NONE',  ( -1.463510566862838091, -44.64091840826481672, 11.94877850058549029 ) ) ;
#14860 = DIRECTION ( 'NONE',  ( -0.5946245182733607137, -0.2512550613902121976, -0.7637359336799429688 ) ) ;
#14861 = CARTESIAN_POINT ( 'NONE',  ( -25.21435515916043357, -16.39063784838764093, -30.48034229288631991 ) ) ;
#14862 = CARTESIAN_POINT ( 'NONE',  ( -4.178947244162637631, -25.96944194166761832, 41.47292084251660782 ) ) ;
#14863 = ORIENTED_EDGE ( 'NONE', *, *, #522, .T. ) ;
#14864 = ORIENTED_EDGE ( 'NONE', *, *, #14938, .F. ) ;
#14865 = CARTESIAN_POINT ( 'NONE',  ( 1.832998868059890096, -141.8272129421610828, 30.69214149073967590 ) ) ;
#14866 = CARTESIAN_POINT ( 'NONE',  ( 21.16825799904901828, 37.62905626541876103, -130.1008673867301297 ) ) ;
#14867 = VERTEX_POINT ( 'NONE', #13985 ) ;
#14868 = CONICAL_SURFACE ( 'NONE', #5680, 34.60786435723138510, 0.8559913436420825139 ) ;
#14869 = ORIENTED_EDGE ( 'NONE', *, *, #2728, .T. ) ;
#14870 = AXIS2_PLACEMENT_3D ( 'NONE', #3140, #20686, #9915 ) ;
#14871 = ORIENTED_EDGE ( 'NONE', *, *, #2568, .T. ) ;
#14872 = CARTESIAN_POINT ( 'NONE',  ( -55.24340739397742084, 0.003826481709804142178, -0.009386184976286654491 ) ) ;
#14873 = CARTESIAN_POINT ( 'NONE',  ( -25.21435515916043357, 6.169479169075458458, -34.05351380035335751 ) ) ;
#14874 = CARTESIAN_POINT ( 'NONE',  ( -20.47566338032527966, 27.87687989047307013, -10.72601609985035331 ) ) ;
#14875 = FACE_OUTER_BOUND ( 'NONE', #2591, .T. ) ;
#14876 = CARTESIAN_POINT ( 'NONE',  ( -16.86833981943427929, -5.948101187261880085, -43.82216161736206317 ) ) ;
#14877 = DIRECTION ( 'NONE',  ( -0.5914120900931443270, 0.8010740644654249509, -0.09226095020377109157 ) ) ;
#14878 = ADVANCED_FACE ( 'NONE', ( #20749 ), #9504, .F. ) ;
#14879 = FACE_OUTER_BOUND ( 'NONE', #10140, .T. ) ;
#14880 = CARTESIAN_POINT ( 'NONE',  ( -1.048994561756802391, 26.29622118251734619, 37.49601524795380669 ) ) ;
#14882 = VERTEX_POINT ( 'NONE', #25088 ) ;
#14881 = ADVANCED_FACE ( 'NONE', ( #24523 ), #18485, .F. ) ;
#14883 = ORIENTED_EDGE ( 'NONE', *, *, #1268, .T. ) ;
#14885 = CARTESIAN_POINT ( 'NONE',  ( -1.056502255334265339, -14.64009593116072949, 43.40574022158788381 ) ) ;
#14884 = CARTESIAN_POINT ( 'NONE',  ( 109.1586900883932856, 0.0001010081143975987133, 0.007137750914550313082 ) ) ;
#14886 = EDGE_CURVE ( 'NONE', #26705, #21599, #5384, .T. ) ;
#14887 = CARTESIAN_POINT ( 'NONE',  ( 25.64708010899960655, -103.1718249732472117, -45.87517365398588964 ) ) ;
#14888 = CARTESIAN_POINT ( 'NONE',  ( 25.73574536432413851, 91.86645484851398180, -65.74844932374561779 ) ) ;
#14889 = ORIENTED_EDGE ( 'NONE', *, *, #21911, .F. ) ;
#14890 = CARTESIAN_POINT ( 'NONE',  ( 2.430230287190581429, -46.34481016236919260, 137.9371479820460991 ) ) ;
#14891 = CARTESIAN_POINT ( 'NONE',  ( 1.833485406944043827, -144.2578170162061895, -15.69895494453532869 ) ) ;
#14892 = CARTESIAN_POINT ( 'NONE',  ( -20.20612092514784663, 23.26073121129637045, -18.30568145913851907 ) ) ;
#14893 = ORIENTED_EDGE ( 'NONE', *, *, #24199, .T. ) ;
#14894 = VERTEX_POINT ( 'NONE', #749 ) ;
#14895 = B_SPLINE_CURVE_WITH_KNOTS ( 'NONE', 3,
 ( #17284, #21898, #4334, #12966, #21761, #7, #24210, #26350, #26486, #11100 ),
 .UNSPECIFIED., .F., .F.,
 ( 4, 3, 3, 4 ),
 ( 3.469446951953614189E-17, 0.0002669559177086189305, 0.0005339118354150960196, 0.001067817517169165984 ),
 .UNSPECIFIED. ) ;
#14896 = CARTESIAN_POINT ( 'NONE',  ( -1.619063947482197729, -29.22875152547781852, -35.99532424477369830 ) ) ;
#14897 = ORIENTED_EDGE ( 'NONE', *, *, #5648, .T. ) ;
#14898 = ORIENTED_EDGE ( 'NONE', *, *, #14180, .T. ) ;
#14899 = FACE_OUTER_BOUND ( 'NONE', #25111, .T. ) ;
#14900 = ORIENTED_EDGE ( 'NONE', *, *, #11503, .T. ) ;
#14901 = CARTESIAN_POINT ( 'NONE',  ( 30.59141879584294088, -55.75104644134820120, -101.9665761624296181 ) ) ;
#14902 =( BOUNDED_SURFACE ( )  B_SPLINE_SURFACE ( 3, 1, ( 
 ( #26500, #8963 ),
 ( #2754, #17855 ),
 ( #13397, #453 ),
 ( #18001, #13258 ) ),
 .UNSPECIFIED., .F., .F., .F. ) 
 B_SPLINE_SURFACE_WITH_KNOTS ( ( 4, 4 ),
 ( 2, 2 ),
 ( 0.000000000000000000, 1.000000000000000000 ),
 ( 0.000000000000000000, 1.000000000000000000 ),
 .UNSPECIFIED. ) 
 GEOMETRIC_REPRESENTATION_ITEM ( )  RATIONAL_B_SPLINE_SURFACE ( (
 ( 1.000000000000000000, 1.000000000000000000),
 ( 0.9934239774497837239, 0.8357310067453919133),
 ( 0.9934239774497837239, 0.8357310067453919133),
 ( 1.000000000000000000, 1.000000000000000000) ) ) 
 REPRESENTATION_ITEM ( '' )  SURFACE ( )  );
#14903 = CARTESIAN_POINT ( 'NONE',  ( 1.833485406944043827, 141.8265699653867387, 30.69200235378984232 ) ) ;
#14904 = CARTESIAN_POINT ( 'NONE',  ( 25.64660436782541808, -107.2041192742818509, 35.44263474731908303 ) ) ;
#14905 = CARTESIAN_POINT ( 'NONE',  ( 1.831572820252009626, -116.8148281295974868, 86.09108691067734753 ) ) ;
#14906 = DIRECTION ( 'NONE',  ( 0.000000000000000000, 0.000000000000000000, 1.000000000000000000 ) ) ;
#14907 = EDGE_CURVE ( 'NONE', #24734, #18908, #20524, .T. ) ;
#14908 = VERTEX_POINT ( 'NONE', #14416 ) ;
#14909 = CARTESIAN_POINT ( 'NONE',  ( 25.64660436782539321, 103.3839381879733992, 45.39454672041161132 ) ) ;
#14910 = CARTESIAN_POINT ( 'NONE',  ( -20.57838717382308502, 25.16001208503106668, -16.28767523336130196 ) ) ;
#14911 = DIRECTION ( 'NONE',  ( 0.000000000000000000, 1.000000000000000000, -6.938893903907228378E-16 ) ) ;
#14913 = ORIENTED_EDGE ( 'NONE', *, *, #4099, .F. ) ;
#14912 = EDGE_CURVE ( 'NONE', #21365, #25689, #10273, .T. ) ;
#14914 = VERTEX_POINT ( 'NONE', #23225 ) ;
#14915 = CARTESIAN_POINT ( 'NONE',  ( -8.786685647604892679, -53.04920435127177569, 7.199674155859498548 ) ) ;
#14916 = CARTESIAN_POINT ( 'NONE',  ( -18.41936578851709783, -29.33493038358050242, 30.66520733838684265 ) ) ;
#14917 = CARTESIAN_POINT ( 'NONE',  ( 109.1592201516379674, 0.005485778713202931790, 0.005631912476303835985 ) ) ;
#14918 = CARTESIAN_POINT ( 'NONE',  ( -5.986830583229481917, -46.64941882410784757, 19.95149887249902321 ) ) ;
#14919 = CARTESIAN_POINT ( 'NONE',  ( -7.733045908741336127, 5.980865481988145937, -52.15131830128824220 ) ) ;
#14920 = VERTEX_POINT ( 'NONE', #19032 ) ;
#14921 = CARTESIAN_POINT ( 'NONE',  ( -22.23226125620943705, -20.31044300692189708, -24.24619897613468211 ) ) ;
#14922 = CARTESIAN_POINT ( 'NONE',  ( 109.1586900883932856, -0.006757191295060861226, -0.002301750759599751131 ) ) ;
#14923 = ORIENTED_EDGE ( 'NONE', *, *, #1536, .F. ) ;
#14924 = CARTESIAN_POINT ( 'NONE',  ( 25.64692872815576408, -112.3258062264003172, 11.48248630407242743 ) ) ;
#14925 = CARTESIAN_POINT ( 'NONE',  ( 1.832998868059890096, 141.8272129421608838, 30.69214149074059961 ) ) ;
#14926 = CARTESIAN_POINT ( 'NONE',  ( -8.259864102781492079, -38.68084189741939127, 36.24929574824932388 ) ) ;
#14927 = CARTESIAN_POINT ( 'NONE',  ( 28.37599760073042887, 75.42809173301607473, 86.45296943207047491 ) ) ;
#14928 = CARTESIAN_POINT ( 'NONE',  ( -55.24728320129491266, -0.01453410071985230222, 0.0006547948648737443372 ) ) ;
#14929 = ORIENTED_EDGE ( 'NONE', *, *, #26407, .T. ) ;
#14930 = CARTESIAN_POINT ( 'NONE',  ( 109.1592201516379674, 0.004867031887010210903, -0.006174480289200333372 ) ) ;
#14931 = ORIENTED_EDGE ( 'NONE', *, *, #26065, .F. ) ;
#14932 = CARTESIAN_POINT ( 'NONE',  ( 32.73300124599739291, -113.0038235389599635, -32.68291970228351317 ) ) ;
#14933 = CARTESIAN_POINT ( 'NONE',  ( 25.81918753295377300, 65.67738364544850072, -91.98563552012969069 ) ) ;
#14934 = CARTESIAN_POINT ( 'NONE',  ( 25.64699802086727942, 103.0525896353907882, -46.14225289916203110 ) ) ;
#14935 = CARTESIAN_POINT ( 'NONE',  ( 55.49584447822657296, 36.04376091928632064, -62.96491934285955239 ) ) ;
#14936 = EDGE_CURVE ( 'NONE', #119, #24971, #8160, .T. ) ;
#14937 = CARTESIAN_POINT ( 'NONE',  ( -20.57838717382308147, -18.89542499756516847, -23.26537097894098594 ) ) ;
#14938 = EDGE_CURVE ( 'NONE', #2577, #10758, #22214, .T. ) ;
#14939 = FACE_OUTER_BOUND ( 'NONE', #7782, .T. ) ;
#14940 = CARTESIAN_POINT ( 'NONE',  ( 1.833485406944043827, 137.8414413349092058, -45.34878176254091642 ) ) ;
#14941 = CARTESIAN_POINT ( 'NONE',  ( -24.53237795827026346, 16.68575684089495326, -29.54731592868563439 ) ) ;
#14942 = CARTESIAN_POINT ( 'NONE',  ( 1.833485406944043827, -132.3460930279895535, 59.50871042846178938 ) ) ;
#14943 = EDGE_CURVE ( 'NONE', #14322, #309, #28074, .T. ) ;
#14944 = CARTESIAN_POINT ( 'NONE',  ( -55.24390624410018802, -0.007245494385991098352, -0.007503127514281985981 ) ) ;
#14945 = VECTOR ( 'NONE', #16472, 1000.000000000000114 ) ;
#14946 = CARTESIAN_POINT ( 'NONE',  ( -8.786685647604890903, -9.545808661480235102, 52.67761315067295413 ) ) ;
#14947 = CARTESIAN_POINT ( 'NONE',  ( 109.1721716018069657, -0.01695288006057377866, 0.001984900887706570523 ) ) ;
#14948 = CARTESIAN_POINT ( 'NONE',  ( -1.323830074806773283, -46.01435746200692023, -2.318057800980537930 ) ) ;
#14949 = ORIENTED_EDGE ( 'NONE', *, *, #22802, .F. ) ;
#14950 = ORIENTED_EDGE ( 'NONE', *, *, #581, .T. ) ;
#14951 = VERTEX_POINT ( 'NONE', #3768 ) ;
#14952 = CARTESIAN_POINT ( 'NONE',  ( 109.1592201516379674, -0.006536841731953435194, 0.004368284148528988643 ) ) ;
#14953 = CARTESIAN_POINT ( 'NONE',  ( 55.49584447822657296, -58.53775398922227424, -42.86099773636601640 ) ) ;
#14954 = CARTESIAN_POINT ( 'NONE',  ( 26.11404676487256893, -92.25884714080449100, 65.63269960453210672 ) ) ;
#14955 = LINE ( 'NONE', #17121, #22562 ) ;
#14956 = DIRECTION ( 'NONE',  ( -1.000000000000000000, -0.000000000000000000, -0.000000000000000000 ) ) ;
#14957 =( BOUNDED_SURFACE ( )  B_SPLINE_SURFACE ( 3, 1, ( 
 ( #24983, #22682 ),
 ( #20636, #5526 ),
 ( #27100, #26829 ),
 ( #20357, #16322 ) ),
 .UNSPECIFIED., .F., .F., .F. ) 
 B_SPLINE_SURFACE_WITH_KNOTS ( ( 4, 4 ),
 ( 2, 2 ),
 ( 0.000000000000000000, 1.000000000000000000 ),
 ( 0.000000000000000000, 1.000000000000000000 ),
 .UNSPECIFIED. ) 
 GEOMETRIC_REPRESENTATION_ITEM ( )  RATIONAL_B_SPLINE_SURFACE ( (
 ( 1.000000000000000000, 1.000000000000000000),
 ( 0.9956975270656955868, 0.8568959468854907557),
 ( 0.9956975270656955868, 0.8568959468854907557),
 ( 1.000000000000000000, 1.000000000000000000) ) ) 
 REPRESENTATION_ITEM ( '' )  SURFACE ( )  );
#14958 = CARTESIAN_POINT ( 'NONE',  ( -8.786685647604931759, 47.14957014837394667, 25.35688121747446999 ) ) ;
#14959 = CARTESIAN_POINT ( 'NONE',  ( -20.57838717382308147, -1.611677988432568709, -29.92853265176830746 ) ) ;
#14960 = ORIENTED_EDGE ( 'NONE', *, *, #20732, .T. ) ;
#14961 = CARTESIAN_POINT ( 'NONE',  ( 2.063896406836609909, 107.0521644432430577, -98.19887492195755385 ) ) ;
#14962 = CARTESIAN_POINT ( 'NONE',  ( -20.20612091757422846, -18.30568244821359869, 23.26073043121652262 ) ) ;
#14963 = CARTESIAN_POINT ( 'NONE',  ( -1.050231094221220296, -37.20185272688478051, -26.71409683968603588 ) ) ;
#14964 = CARTESIAN_POINT ( 'NONE',  ( 1.834118845439484335, 14.99112450600249424, 144.3336252355297802 ) ) ;
#14965 = ORIENTED_EDGE ( 'NONE', *, *, #28413, .T. ) ;
#14966 = CARTESIAN_POINT ( 'NONE',  ( 32.73300124599741423, -97.37344512919810313, -66.00340565729437969 ) ) ;
#14967 = B_SPLINE_CURVE_WITH_KNOTS ( 'NONE', 3,
 ( #20447, #4907, #24498, #11955, #18269, #24789 ),
 .UNSPECIFIED., .F., .F.,
 ( 4, 2, 4 ),
 ( 1.734723475976806902E-18, 0.0004335151646191491353, 0.0008670303292382965359 ),
 .UNSPECIFIED. ) ;
#14968 = LINE ( 'NONE', #12389, #1504 ) ;
#14969 = ORIENTED_EDGE ( 'NONE', *, *, #25536, .F. ) ;
#14970 = B_SPLINE_CURVE_WITH_KNOTS ( 'NONE', 3,
 ( #4609, #6788, #6645, #4902, #19867, #3134, #15397, #21895, #22177, #24207 ),
 .UNSPECIFIED., .F., .F.,
 ( 4, 2, 2, 2, 4 ),
 ( 8.673617379884035472E-19, 0.0003346267210630925128, 0.0006692534421261841582, 0.001003880163189275858, 0.001338506884252367449 ),
 .UNSPECIFIED. ) ;
#14971 = EDGE_LOOP ( 'NONE', ( #26678, #14515, #26878, #9422 ) ) ;
#14972 = VECTOR ( 'NONE', #5670, 999.9999999999997726 ) ;
#14973 = ORIENTED_EDGE ( 'NONE', *, *, #21320, .T. ) ;
#14974 = ADVANCED_FACE ( 'NONE', ( #10405 ), #25500, .F. ) ;
#14975 = CONICAL_SURFACE ( 'NONE', #18658, 117.6351876552689504, 0.9945805576725580410 ) ;
#14976 = CARTESIAN_POINT ( 'NONE',  ( 1.834118845439484335, -117.5010238212704081, 85.14950727125821572 ) ) ;
#14977 = ADVANCED_FACE ( 'NONE', ( #21323 ), #11690, .F. ) ;
#14978 = CARTESIAN_POINT ( 'NONE',  ( -55.24300891470650754, -0.009225237711100996510, 0.003362556190412404646 ) ) ;
#14979 = EDGE_CURVE ( 'NONE', #25910, #23596, #22542, .T. ) ;
#14980 = B_SPLINE_CURVE_WITH_KNOTS ( 'NONE', 3,
 ( #14989, #14857, #4053, #21614 ),
 .UNSPECIFIED., .F., .F.,
 ( 4, 4 ),
 ( 6.469565094841817044E-16, 0.008383748772660085113 ),
 .UNSPECIFIED. ) ;
#14981 = PLANE ( 'NONE',  #23075 ) ;
#14982 = CARTESIAN_POINT ( 'NONE',  ( 8.186469777910764023, -42.84118569629447393, 143.0750864738774908 ) ) ;
#14983 = ORIENTED_EDGE ( 'NONE', *, *, #24594, .F. ) ;
#14984 = CARTESIAN_POINT ( 'NONE',  ( -55.24390624410018802, -0.009374879212966679906, -0.004572280736703028189 ) ) ;
#14985 = B_SPLINE_CURVE_WITH_KNOTS ( 'NONE', 3,
 ( #15417, #25824, #19609, #21630, #6119, #23684, #24232, #12707 ),
 .UNSPECIFIED., .F., .F.,
 ( 4, 2, 2, 4 ),
 ( 1.993045536433795054E-17, 0.0002429588503611392926, 0.0004859177007222586901, 0.0009718354014445028518 ),
 .UNSPECIFIED. ) ;
#14986 = CARTESIAN_POINT ( 'NONE',  ( -55.24728320129491266, -0.009072670231977940022, 0.01137345571547076703 ) ) ;
#14987 = CARTESIAN_POINT ( 'NONE',  ( -22.34422965417122953, 37.30738373203627845, 6.759368364653937533 ) ) ;
#14988 = CARTESIAN_POINT ( 'NONE',  ( -2.911734481061404090, 40.13920818157116344, 25.69892591260225245 ) ) ;
#14989 = CARTESIAN_POINT ( 'NONE',  ( 32.73300124599738581, 99.90245962373917621, -62.10906484417127871 ) ) ;
#14990 = LINE ( 'NONE', #26211, #9242 ) ;
#14991 = CARTESIAN_POINT ( 'NONE',  ( -25.21435515916043002, 31.17620025257588523, -15.02493970636157705 ) ) ;
#14992 = ORIENTED_EDGE ( 'NONE', *, *, #5666, .T. ) ;
#14993 = ORIENTED_EDGE ( 'NONE', *, *, #21951, .F. ) ;
#14994 = CARTESIAN_POINT ( 'NONE',  ( -1.539760825549689294, 44.72358953107748647, 11.93465943778467597 ) ) ;
#14995 = ORIENTED_EDGE ( 'NONE', *, *, #15957, .T. ) ;
#14996 = B_SPLINE_CURVE_WITH_KNOTS ( 'NONE', 3,
 ( #25462, #5735, #12330, #23297, #21258, #19105, #3549, #18535, #27301, #5431 ),
 .UNSPECIFIED., .F., .F.,
 ( 4, 2, 2, 2, 4 ),
 ( 1.563658610346375379E-18, 0.0003346267210630944644, 0.0006692534421261873024, 0.001003880163189280195, 0.001338506884252373087 ),
 .UNSPECIFIED. ) ;
#14997 = ORIENTED_EDGE ( 'NONE', *, *, #10878, .T. ) ;
#14998 = VERTEX_POINT ( 'NONE', #9980 ) ;
#14999 = EDGE_CURVE ( 'NONE', #7798, #23222, #25656, .T. ) ;
#15000 = EDGE_CURVE ( 'NONE', #823, #17620, #8791, .T. ) ;
#15001 = CARTESIAN_POINT ( 'NONE',  ( 24.01988960052059596, 84.46375358746919915, 100.1926921796487022 ) ) ;
#15002 = ADVANCED_FACE ( 'NONE', ( #24065 ), #26213, .F. ) ;
#15003 = CARTESIAN_POINT ( 'NONE',  ( -55.24340739397742084, 0.009386184976286932047, 0.003826481709803695053 ) ) ;
#15004 = ADVANCED_FACE ( 'NONE', ( #4598 ), #16470, .F. ) ;
#15005 = CARTESIAN_POINT ( 'NONE',  ( -20.57838717382308502, 27.96569011373086866, -10.78122205917010135 ) ) ;
#15006 = DIRECTION ( 'NONE',  ( -0.5914120900931443270, 0.3352908775637156724, 0.7333565075147365775 ) ) ;
#15007 = CARTESIAN_POINT ( 'NONE',  ( 28.37603512858453669, -65.97809844506187460, 93.86378016273945946 ) ) ;
#15008 = CARTESIAN_POINT ( 'NONE',  ( 1.833485406944043827, -14.63699153649261575, -144.3694338680886347 ) ) ;
#15009 = CARTESIAN_POINT ( 'NONE',  ( 6.224689322667630975, 144.2687111683195269, 33.28770499679384187 ) ) ;
#15010 = CARTESIAN_POINT ( 'NONE',  ( -1.045287976400386842, 37.92705037016744285, -25.66401692420027203 ) ) ;
#15011 = CARTESIAN_POINT ( 'NONE',  ( 1.833721034905678948, 132.4192200895890323, -59.34646046113644502 ) ) ;
#15012 = ORIENTED_EDGE ( 'NONE', *, *, #6512, .T. ) ;
#15013 = EDGE_LOOP ( 'NONE', ( #8600, #7319, #311, #13837 ) ) ;
#15015 = FACE_BOUND ( 'NONE', #6377, .T. ) ;
#15014 = CARTESIAN_POINT ( 'NONE',  ( 2.263178113027034755, 144.7392881653025825, -13.80342493153361971 ) ) ;
#15016 = CARTESIAN_POINT ( 'NONE',  ( -7.078251931573406708, 34.59014398252973166, 38.93060825814192327 ) ) ;
#15018 = ADVANCED_FACE ( 'NONE', ( #26338 ), #20496, .F. ) ;
#15017 = CARTESIAN_POINT ( 'NONE',  ( 109.1778270068192853, 0.008360410075196072002, -0.004106684808170042375 ) ) ;
#15019 = CARTESIAN_POINT ( 'NONE',  ( 14.74894986621300319, -1.025372615548127706E-16, 37.50000000000001421 ) ) ;
#15020 = ORIENTED_EDGE ( 'NONE', *, *, #16176, .F. ) ;
#15021 = CARTESIAN_POINT ( 'NONE',  ( 26.11404676487256893, -12.95861723607530003, 112.4785329405481349 ) ) ;
#15022 = CARTESIAN_POINT ( 'NONE',  ( 32.73300124599732186, 0.000000000000000000, 0.000000000000000000 ) ) ;
#15023 = DIRECTION ( 'NONE',  ( 1.000000000000000000, -6.938893903907226837E-18, 1.734723475976806709E-18 ) ) ;
#15024 = ORIENTED_EDGE ( 'NONE', *, *, #21460, .T. ) ;
#15025 = EDGE_LOOP ( 'NONE', ( #20601, #14292, #8419, #3395 ) ) ;
#15026 = CARTESIAN_POINT ( 'NONE',  ( -1.323830074806774615, -16.42382241777507090, 43.04593525292983003 ) ) ;
#15027 = CARTESIAN_POINT ( 'NONE',  ( 2.433796855181233454, 118.5671979538056888, 84.34988187690970562 ) ) ;
#15028 = ORIENTED_EDGE ( 'NONE', *, *, #17280, .F. ) ;
#15029 = ADVANCED_FACE ( 'NONE', ( #15390 ), #22536, .F. ) ;
#15030 = B_SPLINE_CURVE_WITH_KNOTS ( 'NONE', 3,
 ( #10658, #17122, #4024, #8218, #23634, #6337, #14822 ),
 .UNSPECIFIED., .F., .F.,
 ( 4, 3, 4 ),
 ( 4.987111262633357592E-16, 0.02816610861753247180, 0.04000277880656273599 ),
 .UNSPECIFIED. ) ;
#15031 = CARTESIAN_POINT ( 'NONE',  ( 2.433796855181205476, -13.76554153471595043, -144.8571464219890572 ) ) ;
#15032 = ORIENTED_EDGE ( 'NONE', *, *, #13678, .F. ) ;
#15033 = EDGE_CURVE ( 'NONE', #16027, #19236, #6449, .T. ) ;
#15034 = CARTESIAN_POINT ( 'NONE',  ( -1.113548883309547710, 1.968251867498868934, -45.82026503946952545 ) ) ;
#15035 = CARTESIAN_POINT ( 'NONE',  ( -25.21435515916043357, -15.02493970636125198, 31.17620025257602379 ) ) ;
#15036 = CARTESIAN_POINT ( 'NONE',  ( 25.81918753295379432, -110.7464580477335971, -22.58534689649783544 ) ) ;
#15037 = CARTESIAN_POINT ( 'NONE',  ( 55.79472521941426777, 71.31192372336693097, -14.41365263906483207 ) ) ;
#15038 = CARTESIAN_POINT ( 'NONE',  ( -1.049817751779893227, 14.63752841325048237, -43.39729912094385611 ) ) ;
#15039 = DIRECTION ( 'NONE',  ( -0.5914120900931443270, 0.7693434820005534691, 0.2415416038592990700 ) ) ;
#15040 = CARTESIAN_POINT ( 'NONE',  ( 10.93730112726006354, 150.7858122213665126, -10.89264110824830034 ) ) ;
#15042 = CARTESIAN_POINT ( 'NONE',  ( 8.186469829614045679, 97.33125097511879176, 113.2805153378639886 ) ) ;
#15041 = LINE ( 'NONE', #13038, #18961 ) ;
#15043 = CARTESIAN_POINT ( 'NONE',  ( -55.24300891470648622, 0.007734635432133147095, 0.006048736206180498759 ) ) ;
#15044 = EDGE_LOOP ( 'NONE', ( #8653, #2669, #18178, #5612 ) ) ;
#15045 = VERTEX_POINT ( 'NONE', #8644 ) ;
#15046 = CARTESIAN_POINT ( 'NONE',  ( 2.433796855181233454, 16.65276281464563723, 144.5536872373192807 ) ) ;
#15047 = CARTESIAN_POINT ( 'NONE',  ( -1.259920593601967287, 25.19630221849107343, 38.49623866863322519 ) ) ;
#15048 = CARTESIAN_POINT ( 'NONE',  ( -8.786685647604890903, 47.14957014837354876, -25.35688121747519119 ) ) ;
#15049 = CARTESIAN_POINT ( 'NONE',  ( 28.37644542392839142, 58.62516076110045304, 109.6517504963491518 ) ) ;
#15050 = CARTESIAN_POINT ( 'NONE',  ( 25.81918753295378011, -90.88802830332004135, 67.18811037444402245 ) ) ;
#15051 = CARTESIAN_POINT ( 'NONE',  ( -21.41427618760457818, -25.94789270595494202, 16.60878262545447726 ) ) ;
#15052 = FACE_OUTER_BOUND ( 'NONE', #19386, .T. ) ;
#15053 = CARTESIAN_POINT ( 'NONE',  ( 109.1592201516379674, 0.007376275279032895593, -0.002720803050370492436 ) ) ;
#15054 = CARTESIAN_POINT ( 'NONE',  ( -8.786685647604706162, -38.68584556812290032, 37.00619870957955015 ) ) ;
#15055 = CARTESIAN_POINT ( 'NONE',  ( 25.87036335909428075, -55.67065048714079012, 98.40409479825417804 ) ) ;
#15056 = ORIENTED_EDGE ( 'NONE', *, *, #27325, .T. ) ;
#15057 = CARTESIAN_POINT ( 'NONE',  ( -55.24300891470648622, 0.007734635432133147095, 0.006048736206180498759 ) ) ;
#15058 = AXIS2_PLACEMENT_3D ( 'NONE', #12664, #6214, #23780 ) ;
#15059 = CARTESIAN_POINT ( 'NONE',  ( 109.1586900883932856, 0.002109621908814802386, -0.006819617742893407421 ) ) ;
#15060 = B_SPLINE_CURVE_WITH_KNOTS ( 'NONE', 3,
 ( #5537, #1610, #14020, #23119, #7720, #25268, #10410, #5249, #20643, #8388 ),
 .UNSPECIFIED., .F., .F.,
 ( 4, 3, 3, 4 ),
 ( 2.775557561562891351E-17, 0.0002669559177086295015, 0.0005339118354150786724, 0.001067817517169166635 ),
 .UNSPECIFIED. ) ;
#15061 = ADVANCED_FACE ( 'NONE', ( #19444 ), #2678, .F. ) ;
#15062 = ORIENTED_EDGE ( 'NONE', *, *, #4965, .F. ) ;
#15063 = CARTESIAN_POINT ( 'NONE',  ( -1.155001620486265645, 38.31519699443499150, -25.28075036143234300 ) ) ;
#15064 = ADVANCED_FACE ( 'NONE', ( #10820 ), #21158, .T. ) ;
#15065 = LINE ( 'NONE', #1978, #23950 ) ;
#15066 = CARTESIAN_POINT ( 'NONE',  ( 2.263178607246642216, 108.9830946142713941, 96.24282447295480836 ) ) ;
#15067 = EDGE_CURVE ( 'NONE', #9049, #11142, #4672, .T. ) ;
#15068 = CARTESIAN_POINT ( 'NONE',  ( -24.53239521893650377, -22.94500969220219488, 24.99972072650167476 ) ) ;
#15069 = CARTESIAN_POINT ( 'NONE',  ( -25.21435515916025594, 34.29329011225976842, -4.655591116594504086 ) ) ;
#15070 = CARTESIAN_POINT ( 'NONE',  ( -55.24340739397742084, -0.005344433640972736689, -0.008612749836246649457 ) ) ;
#15071 = CARTESIAN_POINT ( 'NONE',  ( -22.34422965417124018, -27.39717383755262148, 26.20925041532883881 ) ) ;
#15072 = CARTESIAN_POINT ( 'NONE',  ( -55.24390624410018802, 0.009209468562451588944, -0.004896917417127890151 ) ) ;
#15073 = B_SPLINE_CURVE_WITH_KNOTS ( 'NONE', 3,
 ( #13020, #4385, #21810, #2068, #6408, #1933, #8705, #21947 ),
 .UNSPECIFIED., .F., .F.,
 ( 4, 2, 2, 4 ),
 ( 0.000000000000000000, 0.0002429588503611198041, 0.0004859177007222396081, 0.0009718354014444737952 ),
 .UNSPECIFIED. ) ;
#15074 = CARTESIAN_POINT ( 'NONE',  ( 21.16825799904898631, 23.82367662028005384, -133.3214686481435081 ) ) ;
#15075 = CARTESIAN_POINT ( 'NONE',  ( -1.048994561756789734, -0.7655149579820232919, 45.79144455904142319 ) ) ;
#15076 = DIRECTION ( 'NONE',  ( 1.000000000000000000, -6.938893903907226837E-18, 1.734723475976806709E-18 ) ) ;
#15077 = CARTESIAN_POINT ( 'NONE',  ( -20.57838717382308147, -1.611677988432151709, 29.92853265176832878 ) ) ;
#15078 = CARTESIAN_POINT ( 'NONE',  ( 25.69398547355838858, -46.61500694509577158, -102.8740393624598681 ) ) ;
#15079 = CARTESIAN_POINT ( 'NONE',  ( -25.21435515916043713, -6.169479169075696490, -34.05351380035330777 ) ) ;
#15080 = ORIENTED_EDGE ( 'NONE', *, *, #20280, .F. ) ;
#15081 = EDGE_LOOP ( 'NONE', ( #25812, #22146, #8375, #22383 ) ) ;
#15082 = ORIENTED_EDGE ( 'NONE', *, *, #17631, .F. ) ;
#15083 = CARTESIAN_POINT ( 'NONE',  ( -12.82751273423876270, 48.43568301531151121, -6.573887447703007147 ) ) ;
#15084 = CARTESIAN_POINT ( 'NONE',  ( -20.37983603106074426, -28.74620395171555742, 7.753708011498863684 ) ) ;
#15085 = CARTESIAN_POINT ( 'NONE',  ( -8.259864102781673267, 38.68084189741949785, -36.24929574824924572 ) ) ;
#15086 = CARTESIAN_POINT ( 'NONE',  ( -10.86508079875786414, -50.32133009257452727, 9.118642906269784021 ) ) ;
#15087 = B_SPLINE_CURVE_WITH_KNOTS ( 'NONE', 3,
 ( #14028, #22547, #16047, #508, #655, #9443, #20647 ),
 .UNSPECIFIED., .F., .F.,
 ( 4, 3, 4 ),
 ( 0.000000000000000000, 0.006568092053401791003, 0.02506242213020846987 ),
 .UNSPECIFIED. ) ;
#15088 = CARTESIAN_POINT ( 'NONE',  ( -55.24271866751342941, 0.008488649505343330570, 0.004256484107795472684 ) ) ;
#15089 = ADVANCED_FACE ( 'NONE', ( #26902 ), #14618, .F. ) ;
#15090 = CARTESIAN_POINT ( 'NONE',  ( 16.75465622695626067, 75.09093759627036491, -120.7871673903169238 ) ) ;
#15091 = CARTESIAN_POINT ( 'NONE',  ( 1.833206308920069638, 97.64934899952852732, -107.3376449983717720 ) ) ;
#15092 = ORIENTED_EDGE ( 'NONE', *, *, #18024, .F. ) ;
#15093 = CARTESIAN_POINT ( 'NONE',  ( 32.73300124599735739, 39.98094346392311138, 110.6325518752275485 ) ) ;
#15094 = CARTESIAN_POINT ( 'NONE',  ( 26.28373643307409324, -55.65614982951218082, -114.7784771129679910 ) ) ;
#15095 = CARTESIAN_POINT ( 'NONE',  ( 25.64699802086725455, 23.24292564406190564, -110.4930320910558663 ) ) ;
#15096 = CARTESIAN_POINT ( 'NONE',  ( 1.832998868059890096, 15.69902610990374647, 144.2584710144581095 ) ) ;
#15097 = EDGE_CURVE ( 'NONE', #6273, #26826, #21855, .T. ) ;
#15098 = ORIENTED_EDGE ( 'NONE', *, *, #28078, .F. ) ;
#15099 = CARTESIAN_POINT ( 'NONE',  ( 25.64708228042120908, -112.2886173090158763, -11.84161204513374699 ) ) ;
#15100 = DIRECTION ( 'NONE',  ( 0.000000000000000000, 0.000000000000000000, 1.000000000000000000 ) ) ;
#15101 = ORIENTED_EDGE ( 'NONE', *, *, #16125, .F. ) ;
#15102 = ADVANCED_FACE ( 'NONE', ( #9211 ), #24380, .F. ) ;
#15103 = ORIENTED_EDGE ( 'NONE', *, *, #2764, .T. ) ;
#15104 = VERTEX_POINT ( 'NONE', #712 ) ;
#15105 = CARTESIAN_POINT ( 'NONE',  ( 109.1586059443104944, 0.005438258427225613027, -0.004524147648833186895 ) ) ;
#15106 = CARTESIAN_POINT ( 'NONE',  ( -1.239374126674604337, -35.79060836339833429, -28.97829083655425819 ) ) ;
#15107 = CARTESIAN_POINT ( 'NONE',  ( 1.833603222531960730, 72.16916166673740918, 125.8904991419469468 ) ) ;
#15108 =( BOUNDED_SURFACE ( )  B_SPLINE_SURFACE ( 3, 1, ( 
 ( #21126, #7779 ),
 ( #16533, #23452 ),
 ( #5449, #27320 ),
 ( #1411, #14363 ) ),
 .UNSPECIFIED., .F., .F., .F. ) 
 B_SPLINE_SURFACE_WITH_KNOTS ( ( 4, 4 ),
 ( 2, 2 ),
 ( 0.000000000000000000, 1.000000000000000000 ),
 ( 0.000000000000000000, 1.000000000000000000 ),
 .UNSPECIFIED. ) 
 GEOMETRIC_REPRESENTATION_ITEM ( )  RATIONAL_B_SPLINE_SURFACE ( (
 ( 1.000000000000000000, 1.000000000000000000),
 ( 0.7789835883360578528, 0.9689951854195403280),
 ( 0.7789835883360578528, 0.9689951854195403280),
 ( 1.000000000000000000, 1.000000000000000000) ) ) 
 REPRESENTATION_ITEM ( '' )  SURFACE ( )  );
#15109 = LINE ( 'NONE', #1468, #22054 ) ;
#15110 = EDGE_LOOP ( 'NONE', ( #13777, #20771, #25249, #2287 ) ) ;
#15111 = VERTEX_POINT ( 'NONE', #18123 ) ;
#15112 = CARTESIAN_POINT ( 'NONE',  ( -1.239374126674604337, 11.92219841463891861, 44.48112152129332486 ) ) ;
#15113 = CARTESIAN_POINT ( 'NONE',  ( -28.41354790283022069, -18.00456980371888704, 14.62505768302820464 ) ) ;
#15114 = CARTESIAN_POINT ( 'NONE',  ( -20.57838717382308502, 28.96176188950218844, -7.715628353033780584 ) ) ;
#15115 = B_SPLINE_CURVE_WITH_KNOTS ( 'NONE', 3,
 ( #26053, #16988, #3602, #15094, #25922, #25781, #5928 ),
 .UNSPECIFIED., .F., .F.,
 ( 4, 3, 4 ),
 ( 5.174130838430530436E-16, 0.02816610861753244405, 0.04000277880656296497 ),
 .UNSPECIFIED. ) ;
#15116 = CARTESIAN_POINT ( 'NONE',  ( 1.833603222531973609, 97.42748212378425876, -107.5392551439144313 ) ) ;
#15117 = CARTESIAN_POINT ( 'NONE',  ( -1.019300379054419947, 35.83762006677442002, 28.53917295602858673 ) ) ;
#15118 = CARTESIAN_POINT ( 'NONE',  ( 2.430230287190592531, 43.58368230469574200, -138.8342928068215656 ) ) ;
#15119 = CARTESIAN_POINT ( 'NONE',  ( 2.430230287190572103, -142.0258656395019443, -31.67257033707649683 ) ) ;
#15120 = EDGE_CURVE ( 'NONE', #8537, #7646, #1381, .T. ) ;
#15121 = ORIENTED_EDGE ( 'NONE', *, *, #7457, .T. ) ;
#15122 = ADVANCED_FACE ( 'NONE', ( #26756 ), #14731, .T. ) ;
#15123 = ORIENTED_EDGE ( 'NONE', *, *, #3384, .F. ) ;
#15124 = CARTESIAN_POINT ( 'NONE',  ( 109.1586059443104944, -0.0002768082440195784389, 0.007068659269322299411 ) ) ;
#15125 = CARTESIAN_POINT ( 'NONE',  ( -20.57838717382308147, -27.96569011373093971, -10.78122205916989529 ) ) ;
#15126 = ORIENTED_EDGE ( 'NONE', *, *, #11901, .T. ) ;
#15127 = ORIENTED_EDGE ( 'NONE', *, *, #11768, .T. ) ;
#15128 = ORIENTED_EDGE ( 'NONE', *, *, #25197, .T. ) ;
#15129 = B_SPLINE_CURVE_WITH_KNOTS ( 'NONE', 3,
 ( #8193, #6442, #23879, #21553, #26153, #3863 ),
 .UNSPECIFIED., .F., .F.,
 ( 4, 2, 4 ),
 ( 3.903127820947815962E-18, 0.0006311636237756731646, 0.001262327247551342426 ),
 .UNSPECIFIED. ) ;
#15130 = CARTESIAN_POINT ( 'NONE',  ( 1.833838850093465700, 138.0075868208086547, 44.84137955663270247 ) ) ;
#15131 = CARTESIAN_POINT ( 'NONE',  ( -25.21435515916025594, 1.749597353048488237E-16, -4.373993382621220594E-17 ) ) ;
#15132 = CARTESIAN_POINT ( 'NONE',  ( -20.20612092514784308, -18.30568145913859368, -23.26073121129629939 ) ) ;
#15133 =( BOUNDED_SURFACE ( )  B_SPLINE_SURFACE ( 3, 1, ( 
 ( #24681, #15718 ),
 ( #24534, #4798 ),
 ( #13562, #26806 ),
 ( #13992, #11408 ) ),
 .UNSPECIFIED., .F., .F., .F. ) 
 B_SPLINE_SURFACE_WITH_KNOTS ( ( 4, 4 ),
 ( 2, 2 ),
 ( 0.000000000000000000, 1.000000000000000000 ),
 ( 0.000000000000000000, 1.000000000000000000 ),
 .UNSPECIFIED. ) 
 GEOMETRIC_REPRESENTATION_ITEM ( )  RATIONAL_B_SPLINE_SURFACE ( (
 ( 1.000000000000000000, 1.000000000000000000),
 ( 0.9956975270656954757, 0.8568959468854893125),
 ( 0.9956975270656954757, 0.8568959468854893125),
 ( 1.000000000000000000, 1.000000000000000000) ) ) 
 REPRESENTATION_ITEM ( '' )  SURFACE ( )  );
#15134 = DIRECTION ( 'NONE',  ( -0.5914120900931443270, -0.7693434820005518038, -0.2415416038593042602 ) ) ;
#15135 = CARTESIAN_POINT ( 'NONE',  ( 109.1587776205901861, -0.006995903587863990490, -0.002185517590237659631 ) ) ;
#15136 = CARTESIAN_POINT ( 'NONE',  ( -22.34422965417127216, -5.100074259622869199, -37.57019010019544680 ) ) ;
#15137 = CARTESIAN_POINT ( 'NONE',  ( -8.786685647604898008, 38.68584556812353981, 37.00619870957891777 ) ) ;
#15138 = CARTESIAN_POINT ( 'NONE',  ( 1.834118845439484335, -72.40084790867243214, -125.7578880615052412 ) ) ;
#15139 = DIRECTION ( 'NONE',  ( 0.5946245182733607137, -0.7356888587241680044, 0.3243201896541516027 ) ) ;
#15140 = EDGE_CURVE ( 'NONE', #11627, #22401, #6921, .T. ) ;
#15141 = ORIENTED_EDGE ( 'NONE', *, *, #20827, .T. ) ;
#15142 = ORIENTED_EDGE ( 'NONE', *, *, #15603, .F. ) ;
#15143 = EDGE_CURVE ( 'NONE', #26642, #2443, #19110, .T. ) ;
#15145 = CARTESIAN_POINT ( 'NONE',  ( 26.11404676487259024, -57.58742681967517285, 97.48350837663589630 ) ) ;
#15144 = CARTESIAN_POINT ( 'NONE',  ( 1.831572820252008738, 108.4969585352567663, -96.36280042115824074 ) ) ;
#15146 = B_SPLINE_CURVE_WITH_KNOTS ( 'NONE', 3,
 ( #17243, #21714, #15212, #26441, #250, #8613 ),
 .UNSPECIFIED., .F., .F.,
 ( 4, 2, 4 ),
 ( 0.000000000000000000, 0.0004335184443140220763, 0.0008670368886280441527 ),
 .UNSPECIFIED. ) ;
#15147 = AXIS2_PLACEMENT_3D ( 'NONE', #12127, #20896, #1185 ) ;
#15148 = CARTESIAN_POINT ( 'NONE',  ( -25.21435515916043357, -16.39063784838764093, -30.48034229288631991 ) ) ;
#15149 = CARTESIAN_POINT ( 'NONE',  ( -1.056502255334265339, -37.35734037467615565, 26.51074901220544433 ) ) ;
#15150 = CARTESIAN_POINT ( 'NONE',  ( 10.93730112725932635, 0.000000000000000000, 0.000000000000000000 ) ) ;
#15151 = CARTESIAN_POINT ( 'NONE',  ( 109.1589550718174877, 0.006257602293694210574, -0.004269295012386581552 ) ) ;
#15152 = VERTEX_POINT ( 'NONE', #11229 ) ;
#15153 = CARTESIAN_POINT ( 'NONE',  ( -5.986830583229477476, 11.27873876172141365, -49.46736940480261779 ) ) ;
#15154 = EDGE_CURVE ( 'NONE', #12210, #2861, #20473, .T. ) ;
#15155 = CARTESIAN_POINT ( 'NONE',  ( 2.263178113027048077, 118.4461880110615084, -84.32376073259102611 ) ) ;
#15156 = CARTESIAN_POINT ( 'NONE',  ( -20.47566338032527611, 23.19796701701867647, -18.81547714195482612 ) ) ;
#15157 = ORIENTED_EDGE ( 'NONE', *, *, #17473, .T. ) ;
#15158 = VERTEX_POINT ( 'NONE', #22319 ) ;
#15159 = DIRECTION ( 'NONE',  ( -1.000000000000000000, 6.938893903907226837E-18, -1.734723475976806709E-18 ) ) ;
#15160 = ADVANCED_FACE ( 'NONE', ( #2582 ), #28070, .F. ) ;
#15161 = ORIENTED_EDGE ( 'NONE', *, *, #7499, .T. ) ;
#15162 = CARTESIAN_POINT ( 'NONE',  ( 2.063896406836609909, 118.3103904147681789, 84.29612368209191686 ) ) ;
#15163 = ORIENTED_EDGE ( 'NONE', *, *, #10638, .T. ) ;
#15164 = CARTESIAN_POINT ( 'NONE',  ( 109.1589550718175161, 0.005477029346534926200, -0.005233222325307182281 ) ) ;
#15165 = ORIENTED_EDGE ( 'NONE', *, *, #5092, .T. ) ;
#15166 = AXIS2_PLACEMENT_3D ( 'NONE', #5862, #10188, #1528 ) ;
#15167 = FACE_OUTER_BOUND ( 'NONE', #4057, .T. ) ;
#15168 = CARTESIAN_POINT ( 'NONE',  ( 109.1778270068192853, -0.007885345421917336339, 0.004958088776549072693 ) ) ;
#15169 = AXIS2_PLACEMENT_3D ( 'NONE', #19607, #26507, #2174 ) ;
#15170 = B_SPLINE_CURVE_WITH_KNOTS ( 'NONE', 3,
 ( #2994, #7181, #22288, #2548 ),
 .UNSPECIFIED., .F., .F.,
 ( 4, 4 ),
 ( 0.000000000000000000, 0.01077107196513873988 ),
 .UNSPECIFIED. ) ;
#15171 = CARTESIAN_POINT ( 'NONE',  ( 109.1587776205901577, -0.003057017121591250504, 0.006661366261224488383 ) ) ;
#15172 = CARTESIAN_POINT ( 'NONE',  ( 109.1586900883932856, 0.006479576224398247292, -0.002995460350188419631 ) ) ;
#15173 = CARTESIAN_POINT ( 'NONE',  ( 25.86096068574580187, -112.3259320600844120, -12.80894308910849055 ) ) ;
#15174 = CARTESIAN_POINT ( 'NONE',  ( -28.41354790283022069, 22.41474081378001060, -5.969609727608100158 ) ) ;
#15175 = PRODUCT ( 'pinion', 'pinion', '', ( #27292 ) ) ;
#15177 = CARTESIAN_POINT ( 'NONE',  ( -20.57838717382308147, -29.92853265176832878, -1.611677988432255848 ) ) ;
#15176 = CARTESIAN_POINT ( 'NONE',  ( 109.1586900883932856, 0.007109207791180751322, 0.0006456433529069300226 ) ) ;
#15178 = DIRECTION ( 'NONE',  ( 1.000000000000000000, -6.938893903907226837E-18, 1.734723475976806709E-18 ) ) ;
#15179 = EDGE_CURVE ( 'NONE', #27431, #11422, #7442, .T. ) ;
#15180 = ORIENTED_EDGE ( 'NONE', *, *, #947, .F. ) ;
#15181 = VERTEX_POINT ( 'NONE', #23331 ) ;
#15182 = FACE_OUTER_BOUND ( 'NONE', #854, .T. ) ;
#15183 = CARTESIAN_POINT ( 'NONE',  ( -1.113548883309539272, 25.34012683631610940, 38.22628252420783213 ) ) ;
#15184 = EDGE_CURVE ( 'NONE', #22553, #22201, #8454, .T. ) ;
#15185 = CARTESIAN_POINT ( 'NONE',  ( -1.031422197589711764, -37.93675465142452907, 25.67058493451483514 ) ) ;
#15186 = CARTESIAN_POINT ( 'NONE',  ( 25.64681081121880624, -75.86069728268932977, -83.63051021305977883 ) ) ;
#15187 = CARTESIAN_POINT ( 'NONE',  ( 25.70243777736189728, 97.44734253939077462, 57.10783651464997490 ) ) ;
#15188 = CARTESIAN_POINT ( 'NONE',  ( 25.69398547355838502, 90.93418986874891630, -66.98507266663659721 ) ) ;
#15189 = ORIENTED_EDGE ( 'NONE', *, *, #313, .T. ) ;
#15190 = CARTESIAN_POINT ( 'NONE',  ( 1.833838850093440387, -44.84137955663319275, 138.0075868208085694 ) ) ;
#15191 = CARTESIAN_POINT ( 'NONE',  ( -4.162674018437144241, 25.90909455705170217, 41.48630000627025538 ) ) ;
#15192 = EDGE_CURVE ( 'NONE', #2685, #21851, #9157, .T. ) ;
#15193 = VECTOR ( 'NONE', #167, 1000.000000000000000 ) ;
#15194 = CARTESIAN_POINT ( 'NONE',  ( 2.430230287190581429, -60.50928654924843642, 132.3371620660948906 ) ) ;
#15195 = CARTESIAN_POINT ( 'NONE',  ( 2.433796855181205476, -145.5024947199069629, -1.451562450951161987 ) ) ;
#15196 = CARTESIAN_POINT ( 'NONE',  ( 25.64681081121880624, -56.09509703373412748, 97.99105938547904771 ) ) ;
#15197 = CIRCLE ( 'NONE', #16599, 34.60786435723138510 ) ;
#15198 = ORIENTED_EDGE ( 'NONE', *, *, #9707, .F. ) ;
#15199 = CARTESIAN_POINT ( 'NONE',  ( 109.1589550718175161, -0.004632048724982944926, -0.005994046294305891559 ) ) ;
#15200 = CONICAL_SURFACE ( 'NONE', #4184, 34.60786435723138510, 0.8559913436420825139 ) ;
#15201 = CARTESIAN_POINT ( 'NONE',  ( 1.894214914920945514, -59.90782071839110756, -132.2104617488243150 ) ) ;
#15202 = ORIENTED_EDGE ( 'NONE', *, *, #3299, .F. ) ;
#15203 = CARTESIAN_POINT ( 'NONE',  ( 10.93730112725932635, 0.000000000000000000, 0.000000000000000000 ) ) ;
#15204 = DIRECTION ( 'NONE',  ( -0.7637818620346800147, -0.3617919495470753866, 0.5345501402766286159 ) ) ;
#15205 = DIRECTION ( 'NONE',  ( 0.000000000000000000, 0.000000000000000000, -1.000000000000000000 ) ) ;
#15206 = CARTESIAN_POINT ( 'NONE',  ( -1.155031165708881202, -12.20332162035433576, 44.25214473648924951 ) ) ;
#15207 = CARTESIAN_POINT ( 'NONE',  ( 10.93730112725932635, 0.000000000000000000, 0.000000000000000000 ) ) ;
#15208 = DIRECTION ( 'NONE',  ( 0.7563875759206387661, 0.5490129373055256945, -0.3556158456312918936 ) ) ;
#15209 = VECTOR ( 'NONE', #23000, 1000.000000000000000 ) ;
#15210 = B_SPLINE_CURVE_WITH_KNOTS ( 'NONE', 3,
 ( #2303, #19882, #170, #8959, #17716, #24506 ),
 .UNSPECIFIED., .F., .F.,
 ( 4, 2, 4 ),
 ( 1.396102177145585797E-16, 0.003570751334075631788, 0.007141502668151123931 ),
 .UNSPECIFIED. ) ;
#15211 = CARTESIAN_POINT ( 'NONE',  ( -25.21435515916043713, -25.00736669481004526, 23.92354251275963861 ) ) ;
#15212 = CARTESIAN_POINT ( 'NONE',  ( -20.24419206586953379, 28.55732805495827265, 7.929973069813099684 ) ) ;
#15213 = CARTESIAN_POINT ( 'NONE',  ( 119.2224693531408803, -69.99999999999998579, -40.00000000000002132 ) ) ;
#15214 = CARTESIAN_POINT ( 'NONE',  ( -25.21435515916043002, -4.655591116594591128, -34.29329011225954105 ) ) ;
#15215 = VECTOR ( 'NONE', #22039, 1000.000000000000114 ) ;
#15216 = CARTESIAN_POINT ( 'NONE',  ( 2.063896406836605024, 132.1577797566306458, 60.31174178979853195 ) ) ;
#15217 = LINE ( 'NONE', #10507, #12974 ) ;
#15218 = CARTESIAN_POINT ( 'NONE',  ( -1.031422197589716205, -43.06660437151298026, 15.60268798220682562 ) ) ;
#15219 = ORIENTED_EDGE ( 'NONE', *, *, #15285, .F. ) ;
#15220 = AXIS2_PLACEMENT_3D ( 'NONE', #15440, #21802, #21652 ) ;
#15221 = VERTEX_POINT ( 'NONE', #27618 ) ;
#15222 = ORIENTED_EDGE ( 'NONE', *, *, #9408, .T. ) ;
#15223 = DIRECTION ( 'NONE',  ( 0.000000000000000000, 0.000000000000000000, 1.000000000000000000 ) ) ;
#15224 = CARTESIAN_POINT ( 'NONE',  ( -20.20612091757424977, 28.48192249925588371, -8.058516044219283359 ) ) ;
#15225 = EDGE_CURVE ( 'NONE', #27772, #25254, #6051, .T. ) ;
#15226 = CARTESIAN_POINT ( 'NONE',  ( 109.1587776205901861, 0.001605238040368368738, 0.007151389024635758027 ) ) ;
#15227 = DIRECTION ( 'NONE',  ( 0.5914120900931445490, -0.6476200150380184706, -0.4804373588864787603 ) ) ;
#15228 = CARTESIAN_POINT ( 'NONE',  ( -20.21097721650786738, -9.464413208035280078, -28.05863614620935209 ) ) ;
#15229 = CARTESIAN_POINT ( 'NONE',  ( 32.73300124599738581, -16.10546300444743650, -116.5274707358856858 ) ) ;
#15230 = CARTESIAN_POINT ( 'NONE',  ( 13.84597867724974662, -146.3210145202069725, 10.56985607909754776 ) ) ;
#15231 = ORIENTED_EDGE ( 'NONE', *, *, #18152, .T. ) ;
#15232 = CARTESIAN_POINT ( 'NONE',  ( -5.986830583229486358, 50.53158596890444443, -4.559539818181313819 ) ) ;
#15233 = CARTESIAN_POINT ( 'NONE',  ( -4.178947244162637631, -11.88256963646706410, 47.46809051147732816 ) ) ;
#15234 = CARTESIAN_POINT ( 'NONE',  ( 2.430230287190572103, -43.58368230469294247, -138.8342928068224751 ) ) ;
#15235 = CARTESIAN_POINT ( 'NONE',  ( 25.65782528836479415, -112.9169519833626509, -0.5778133093789715735 ) ) ;
#15236 = ADVANCED_FACE ( 'NONE', ( #3583 ), #21433, .F. ) ;
#15237 = EDGE_CURVE ( 'NONE', #20966, #10454, #10208, .T. ) ;
#15238 = CARTESIAN_POINT ( 'NONE',  ( -4.178947244162647401, 41.47292084251672151, 25.96944194166747621 ) ) ;
#15239 = EDGE_LOOP ( 'NONE', ( #4627, #5679, #19093, #13055 ) ) ;
#15240 = CARTESIAN_POINT ( 'NONE',  ( -4.162674018437131807, -37.46098494546610880, -31.44946543094281921 ) ) ;
#15241 = CARTESIAN_POINT ( 'NONE',  ( -20.20997486282892552, -0.3303743256173646836, 29.60348406988233450 ) ) ;
#15242 = VERTEX_POINT ( 'NONE', #12363 ) ;
#15243 = EDGE_LOOP ( 'NONE', ( #20978, #24457, #12589, #19698 ) ) ;
#15244 = VERTEX_POINT ( 'NONE', #25494 ) ;
#15245 = VECTOR ( 'NONE', #7946, 1000.000000000000227 ) ;
#15246 = CARTESIAN_POINT ( 'NONE',  ( -20.20700224038492721, 28.44216453106536946, -8.199606986804427677 ) ) ;
#15247 = CARTESIAN_POINT ( 'NONE',  ( -8.786685647604885574, 6.096987947571466530E-17, -1.524246986892866633E-17 ) ) ;
#15248 = DIRECTION ( 'NONE',  ( 0.000000000000000000, 0.000000000000000000, -1.000000000000000000 ) ) ;
#15249 = ORIENTED_EDGE ( 'NONE', *, *, #20467, .T. ) ;
#15250 = CARTESIAN_POINT ( 'NONE',  ( -2.265401668238146815, 29.73100299756566756, -36.42007794497261841 ) ) ;
#15251 = CARTESIAN_POINT ( 'NONE',  ( -1.050230346682677007, -0.0006945978172492803249, 45.79907861045643358 ) ) ;
#15252 = ORIENTED_EDGE ( 'NONE', *, *, #23285, .T. ) ;
#15253 = CONICAL_SURFACE ( 'NONE', #23127, 117.6351876552689504, 0.9945805576725580410 ) ;
#15254 = DIRECTION ( 'NONE',  ( -1.000000000000000000, -0.000000000000000000, -0.000000000000000000 ) ) ;
#15255 = ADVANCED_FACE ( 'NONE', ( #8342 ), #16115, .T. ) ;
#15256 = CARTESIAN_POINT ( 'NONE',  ( 55.49584447822657296, 36.50733923851198170, 62.69727227546415094 ) ) ;
#15257 = CARTESIAN_POINT ( 'NONE',  ( 2.063896406836609909, -144.6078654718900793, -13.84738934186338355 ) ) ;
#15258 = CIRCLE ( 'NONE', #2898, 117.6351876552689504 ) ;
#15259 = CARTESIAN_POINT ( 'NONE',  ( 32.73300124599735739, -62.10906484417306928, 99.90245962373816724 ) ) ;
#15260 = LINE ( 'NONE', #13386, #11433 ) ;
#15261 = CARTESIAN_POINT ( 'NONE',  ( -20.47566338032515887, -7.708089572830225222, 28.85746366088577375 ) ) ;
#15262 = VECTOR ( 'NONE', #23812, 1000.000000000000000 ) ;
#15263 = CARTESIAN_POINT ( 'NONE',  ( 109.1586059443104944, 0.003127959656212866632, -0.006344953511164441902 ) ) ;
#15264 = CARTESIAN_POINT ( 'NONE',  ( -1.031422197589711987, -37.93675465142491277, -25.67058493451428802 ) ) ;
#15265 = ORIENTED_EDGE ( 'NONE', *, *, #12962, .F. ) ;
#15266 = ORIENTED_EDGE ( 'NONE', *, *, #8333, .F. ) ;
#15267 = DIRECTION ( 'NONE',  ( 1.000000000000000000, -6.938893903907226837E-18, 1.734723475976806709E-18 ) ) ;
#15268 = LINE ( 'NONE', #8536, #11601 ) ;
#15269 = VERTEX_POINT ( 'NONE', #21565 ) ;
#15270 = VERTEX_POINT ( 'NONE', #17240 ) ;
#15271 = ORIENTED_EDGE ( 'NONE', *, *, #20228, .F. ) ;
#15272 = DIRECTION ( 'NONE',  ( -1.000000000000000000, -0.000000000000000000, -0.000000000000000000 ) ) ;
#15274 =( BOUNDED_SURFACE ( )  B_SPLINE_SURFACE ( 3, 1, ( 
 ( #11646, #9492 ),
 ( #702, #27021 ),
 ( #15263, #17570 ),
 ( #24902, #26356 ) ),
 .UNSPECIFIED., .F., .F., .F. ) 
 B_SPLINE_SURFACE_WITH_KNOTS ( ( 4, 4 ),
 ( 2, 2 ),
 ( 0.000000000000000000, 1.000000000000000000 ),
 ( 0.000000000000000000, 1.000000000000000000 ),
 .UNSPECIFIED. ) 
 GEOMETRIC_REPRESENTATION_ITEM ( )  RATIONAL_B_SPLINE_SURFACE ( (
 ( 1.000000000000000000, 1.000000000000000000),
 ( 0.9960225298536222738, 0.9999952330161893110),
 ( 0.9960225298536222738, 0.9999952330161893110),
 ( 1.000000000000000000, 1.000000000000000000) ) ) 
 REPRESENTATION_ITEM ( '' )  SURFACE ( )  );
#15273 = CIRCLE ( 'NONE', #15741, 117.6351876552689504 ) ;
#15275 = FACE_OUTER_BOUND ( 'NONE', #18205, .T. ) ;
#15276 = CIRCLE ( 'NONE', #2903, 151.1787379149930359 ) ;
#15277 = CARTESIAN_POINT ( 'NONE',  ( 30.59138290137887140, -101.9665464510083694, -55.75105126024025282 ) ) ;
#15278 = CARTESIAN_POINT ( 'NONE',  ( -1.045287976400365970, -45.76855895860947498, -1.530335034933654859 ) ) ;
#15279 = EDGE_CURVE ( 'NONE', #8696, #24633, #25989, .T. ) ;
#15280 = LINE ( 'NONE', #23821, #11636 ) ;
#15281 = EDGE_CURVE ( 'NONE', #13658, #21691, #6473, .T. ) ;
#15282 = CARTESIAN_POINT ( 'NONE',  ( 109.1592201516379674, -0.002913740842103232798, 0.007302213399787543455 ) ) ;
#15283 = CARTESIAN_POINT ( 'NONE',  ( -1.048996300304498419, 0.7649764263858191971, 45.79145529752468491 ) ) ;
#15284 = CARTESIAN_POINT ( 'NONE',  ( -4.162674018437137136, 37.46098494546635038, 31.44946543094254920 ) ) ;
#15285 = EDGE_CURVE ( 'NONE', #28115, #2245, #2780, .T. ) ;
#15286 = CARTESIAN_POINT ( 'NONE',  ( -7.078251931573400491, 51.82710018979476274, 5.101176922830847893 ) ) ;
#15287 = CARTESIAN_POINT ( 'NONE',  ( 13.36082413113063083, -137.0038452127805328, 67.94366799842767080 ) ) ;
#15288 = CARTESIAN_POINT ( 'NONE',  ( -20.20612091757420359, -23.26073043121646933, -18.30568244821369817 ) ) ;
#15289 = ORIENTED_EDGE ( 'NONE', *, *, #10984, .F. ) ;
#15290 = ORIENTED_EDGE ( 'NONE', *, *, #26566, .F. ) ;
#15292 = CARTESIAN_POINT ( 'NONE',  ( 30.59141879584314694, 60.43012207291116766, -99.26511058698837076 ) ) ;
#15291 = DIRECTION ( 'NONE',  ( -1.000000000000000000, -0.000000000000000000, -0.000000000000000000 ) ) ;
#15293 = CARTESIAN_POINT ( 'NONE',  ( -55.25719721206881729, 0.01115102788683387629, -0.0006290797159233242576 ) ) ;
#15294 = CARTESIAN_POINT ( 'NONE',  ( -4.780792508754331038, 11.68149851467529210, 48.13366140756546230 ) ) ;
#15295 = CARTESIAN_POINT ( 'NONE',  ( 1.833485406944057594, -0.5339064996874559599, -145.1085452359073429 ) ) ;
#15296 = CARTESIAN_POINT ( 'NONE',  ( 28.43349137099835033, -80.08535015163967330, 94.99961975860227881 ) ) ;
#15297 = CIRCLE ( 'NONE', #21306, 28.92774122539760384 ) ;
#15298 = ORIENTED_EDGE ( 'NONE', *, *, #8880, .T. ) ;
#15299 = CARTESIAN_POINT ( 'NONE',  ( -7.711401346138389457, 10.36923727626120773, -51.42722225669425740 ) ) ;
#15300 = VECTOR ( 'NONE', #9922, 1000.000000000000114 ) ;
#15301 = FACE_OUTER_BOUND ( 'NONE', #12101, .T. ) ;
#15302 = CARTESIAN_POINT ( 'NONE',  ( -1.046936909428682672, -37.78538189376526901, -25.87632113675147849 ) ) ;
#15303 = VERTEX_POINT ( 'NONE', #10498 ) ;
#15304 = ORIENTED_EDGE ( 'NONE', *, *, #713, .F. ) ;
#15305 = VERTEX_POINT ( 'NONE', #19266 ) ;
#15306 = FACE_OUTER_BOUND ( 'NONE', #5698, .T. ) ;
#15307 = ORIENTED_EDGE ( 'NONE', *, *, #9388, .F. ) ;
#15308 = B_SPLINE_CURVE_WITH_KNOTS ( 'NONE', 3,
 ( #20200, #9283, #2794, #9134, #11573, #26679, #20353 ),
 .UNSPECIFIED., .F., .F.,
 ( 4, 3, 4 ),
 ( 0.000000000000000000, 0.006568092053401769319, 0.02506242213020846987 ),
 .UNSPECIFIED. ) ;
#15309 = B_SPLINE_CURVE_WITH_KNOTS ( 'NONE', 3,
 ( #27011, #19982, #15642, #24318, #24892, #22148 ),
 .UNSPECIFIED., .F., .F.,
 ( 4, 2, 4 ),
 ( 0.000000000000000000, 0.003570751334075635691, 0.007141502668151271382 ),
 .UNSPECIFIED. ) ;
#15310 = CARTESIAN_POINT ( 'NONE',  ( -1.239374126674604337, 42.99367564261279995, -16.50008610789313934 ) ) ;
#15311 = AXIS2_PLACEMENT_3D ( 'NONE', #5794, #23356, #27930 ) ;
#15312 =( BOUNDED_SURFACE ( )  B_SPLINE_SURFACE ( 3, 1, ( 
 ( #8924, #4873 ),
 ( #15506, #18105 ),
 ( #26321, #15812 ),
 ( #13645, #17952 ) ),
 .UNSPECIFIED., .F., .F., .F. ) 
 B_SPLINE_SURFACE_WITH_KNOTS ( ( 4, 4 ),
 ( 2, 2 ),
 ( 0.000000000000000000, 1.000000000000000000 ),
 ( 0.000000000000000000, 1.000000000000000000 ),
 .UNSPECIFIED. ) 
 GEOMETRIC_REPRESENTATION_ITEM ( )  RATIONAL_B_SPLINE_SURFACE ( (
 ( 1.000000000000000000, 1.000000000000000000),
 ( 0.9956975270656955868, 0.8568959468854907557),
 ( 0.9956975270656955868, 0.8568959468854907557),
 ( 1.000000000000000000, 1.000000000000000000) ) ) 
 REPRESENTATION_ITEM ( '' )  SURFACE ( )  );
#15313 = EDGE_CURVE ( 'NONE', #6648, #565, #28011, .T. ) ;
#15314 = ORIENTED_EDGE ( 'NONE', *, *, #1816, .F. ) ;
#15315 = CARTESIAN_POINT ( 'NONE',  ( 6.224689322667647851, -121.2721959030532162, -84.93872395423099420 ) ) ;
#15316 = CARTESIAN_POINT ( 'NONE',  ( 28.37599760073041821, -55.80522390574049041, -100.2461467136616307 ) ) ;
#15317 = CARTESIAN_POINT ( 'NONE',  ( -1.259972190295306715, -38.49631882650665204, -25.19627397134285474 ) ) ;
#15318 = EDGE_CURVE ( 'NONE', #3680, #13750, #16346, .T. ) ;
#15319 = B_SPLINE_CURVE_WITH_KNOTS ( 'NONE', 3,
 ( #9526, #5343, #15696, #27062, #22489, #24507 ),
 .UNSPECIFIED., .F., .F.,
 ( 4, 2, 4 ),
 ( 0.000000000000000000, 0.003570751334075635258, 0.007141502668151270515 ),
 .UNSPECIFIED. ) ;
#15320 = CARTESIAN_POINT ( 'NONE',  ( -1.045287976400383290, 12.68782741917383738, 44.00138577190627842 ) ) ;
#15321 = DIRECTION ( 'NONE',  ( 1.000000000000000000, -6.938893903907226837E-18, 1.734723475976806709E-18 ) ) ;
#15322 = CARTESIAN_POINT ( 'NONE',  ( 32.73300124599735739, 44.31599526637956643, 108.9684813982490539 ) ) ;
#15323 = CARTESIAN_POINT ( 'NONE',  ( 1.833485406944057594, 125.9346397303435197, 72.09189602597754742 ) ) ;
#15324 = CARTESIAN_POINT ( 'NONE',  ( 2.433796855181205476, -118.5671979538062146, 84.34988187690890982 ) ) ;
#15325 = CARTESIAN_POINT ( 'NONE',  ( -55.24340739397742794, 0.008612749836243148785, 0.005344433640974122733 ) ) ;
#15326 = ORIENTED_EDGE ( 'NONE', *, *, #2905, .F. ) ;
#15327 = CARTESIAN_POINT ( 'NONE',  ( 25.64703792032468499, 56.32669596053575134, -97.85829113439902471 ) ) ;
#15328 = CARTESIAN_POINT ( 'NONE',  ( 1.831572820252009626, -86.09108691067693542, -116.8148281295977995 ) ) ;
#15330 = CARTESIAN_POINT ( 'NONE',  ( 25.65782528836481902, 45.39960327191609935, 103.3897864210297115 ) ) ;
#15329 = CARTESIAN_POINT ( 'NONE',  ( -1.239374126674604337, -38.61989855450920572, 25.08410696974284448 ) ) ;
#15331 = B_SPLINE_CURVE_WITH_KNOTS ( 'NONE', 3,
 ( #21370, #16788, #1226, #17188, #25976, #14315, #10025, #18787 ),
 .UNSPECIFIED., .F., .F.,
 ( 4, 2, 2, 4 ),
 ( 0.000000000000000000, 0.0002429592666046771667, 0.0004859185332093543335, 0.0009718370664186896934 ),
 .UNSPECIFIED. ) ;
#15332 = PLANE ( 'NONE',  #17477 ) ;
#15333 = CARTESIAN_POINT ( 'NONE',  ( 25.64681081121879203, 97.57530875170606066, 56.81519825470789442 ) ) ;
#15334 = B_SPLINE_CURVE_WITH_KNOTS ( 'NONE', 3,
 ( #3151, #2867, #15955, #8808, #993, #16097 ),
 .UNSPECIFIED., .F., .F.,
 ( 4, 2, 4 ),
 ( 0.000000000000000000, 0.0004335184443140221305, 0.0008670368886280442611 ),
 .UNSPECIFIED. ) ;
#15335 = CARTESIAN_POINT ( 'NONE',  ( 1.833485406944043827, -137.8414413349082110, -45.34878176254374438 ) ) ;
#15336 = ORIENTED_EDGE ( 'NONE', *, *, #26608, .F. ) ;
#15337 = CARTESIAN_POINT ( 'NONE',  ( -55.24390624410018802, -0.007503127514277506058, -0.007245494385991484328 ) ) ;
#15338 = FACE_OUTER_BOUND ( 'NONE', #4043, .T. ) ;
#15339 = CARTESIAN_POINT ( 'NONE',  ( 10.93730112725990367, -108.9902118373734652, -104.7670965581022671 ) ) ;
#15340 = CARTESIAN_POINT ( 'NONE',  ( 32.73300124599732186, 0.000000000000000000, 0.000000000000000000 ) ) ;
#15341 = CARTESIAN_POINT ( 'NONE',  ( 25.64708010899966339, 75.51173009720632479, -83.94602815988591260 ) ) ;
#15342 = ORIENTED_EDGE ( 'NONE', *, *, #23793, .F. ) ;
#15343 = CARTESIAN_POINT ( 'NONE',  ( -1.239374126674604337, -11.92219841463861130, -44.48112152129341013 ) ) ;
#15344 = CARTESIAN_POINT ( 'NONE',  ( 6.224689322667630975, -97.14981701196246888, -111.7293398381274869 ) ) ;
#15345 = CARTESIAN_POINT ( 'NONE',  ( 1.833838850093440165, -97.09738119087785435, 107.8375718686136508 ) ) ;
#15346 = ORIENTED_EDGE ( 'NONE', *, *, #2253, .F. ) ;
#15347 = CARTESIAN_POINT ( 'NONE',  ( 32.73300124599738581, 32.68291970228383292, -113.0038235389598782 ) ) ;
#15348 = ADVANCED_FACE ( 'NONE', ( #26165 ), #1753, .F. ) ;
#15349 = CARTESIAN_POINT ( 'NONE',  ( 32.73300124599734318, 97.37344512919861472, 66.00340565729376863 ) ) ;
#15350 = DIRECTION ( 'NONE',  ( 0.000000000000000000, 5.223019709707975211E-21, -1.000000000000000000 ) ) ;
#15351 = EDGE_CURVE ( 'NONE', #9272, #25971, #13349, .T. ) ;
#15352 = ORIENTED_EDGE ( 'NONE', *, *, #18060, .T. ) ;
#15353 = DIRECTION ( 'NONE',  ( 1.000000000000000000, -6.938893903907226837E-18, 1.734723475976806709E-18 ) ) ;
#15354 = EDGE_CURVE ( 'NONE', #28309, #20148, #26630, .T. ) ;
#15355 = CARTESIAN_POINT ( 'NONE',  ( 2.108985857320913038, 132.2056553747752901, -60.26444811757266251 ) ) ;
#15356 = CARTESIAN_POINT ( 'NONE',  ( 109.1624594426973260, 0.002129375066970632790, -0.01582142368018301867 ) ) ;
#15357 = DIRECTION ( 'NONE',  ( 0.5914120900931444380, -0.008020494143007482132, 0.8063295922669342364 ) ) ;
#15358 = CARTESIAN_POINT ( 'NONE',  ( 2.430230287190592531, -142.0258656395023706, 31.67257033707456770 ) ) ;
#15359 = DIRECTION ( 'NONE',  ( 0.000000000000000000, 0.000000000000000000, 1.000000000000000000 ) ) ;
#15360 =( BOUNDED_SURFACE ( )  B_SPLINE_SURFACE ( 3, 1, ( 
 ( #12706, #1212 ),
 ( #17027, #8135 ),
 ( #14872, #3507 ),
 ( #12291, #21059 ) ),
 .UNSPECIFIED., .F., .F., .F. ) 
 B_SPLINE_SURFACE_WITH_KNOTS ( ( 4, 4 ),
 ( 2, 2 ),
 ( 0.000000000000000000, 1.000000000000000000 ),
 ( 0.000000000000000000, 1.000000000000000000 ),
 .UNSPECIFIED. ) 
 GEOMETRIC_REPRESENTATION_ITEM ( )  RATIONAL_B_SPLINE_SURFACE ( (
 ( 1.000000000000000000, 1.000000000000000000),
 ( 0.9934239774497838349, 0.8357310067453913582),
 ( 0.9934239774497838349, 0.8357310067453913582),
 ( 1.000000000000000000, 1.000000000000000000) ) ) 
 REPRESENTATION_ITEM ( '' )  SURFACE ( )  );
#15361 = EDGE_CURVE ( 'NONE', #1094, #20246, #4824, .T. ) ;
#15362 = DIRECTION ( 'NONE',  ( -1.000000000000000000, -0.000000000000000000, -0.000000000000000000 ) ) ;
#15363 = DIRECTION ( 'NONE',  ( 0.000000000000000000, 0.000000000000000000, 1.000000000000000000 ) ) ;
#15364 = CARTESIAN_POINT ( 'NONE',  ( 26.04756280548352620, -98.56594554799085017, -55.62433096787529507 ) ) ;
#15365 = VERTEX_POINT ( 'NONE', #15069 ) ;
#15366 = ORIENTED_EDGE ( 'NONE', *, *, #20949, .F. ) ;
#15367 = DIRECTION ( 'NONE',  ( 1.000000000000000000, -0.000000000000000000, -0.000000000000000000 ) ) ;
#15368 = CARTESIAN_POINT ( 'NONE',  ( -20.57838717382308502, 28.96176188950218844, -7.715628353033780584 ) ) ;
#15369 = CARTESIAN_POINT ( 'NONE',  ( -2.911734481061421853, 36.84482841982651280, -30.23325065583374638 ) ) ;
#15370 = B_SPLINE_CURVE_WITH_KNOTS ( 'NONE', 3,
 ( #3433, #20849, #7627, #3146, #20977, #7919, #22593 ),
 .UNSPECIFIED., .F., .F.,
 ( 4, 3, 4 ),
 ( 0.000000000000000000, 0.006568092053401790135, 0.02506242213020846640 ),
 .UNSPECIFIED. ) ;
#15371 = CARTESIAN_POINT ( 'NONE',  ( 32.73300124599738581, -97.37344512919901263, 66.00340565729310072 ) ) ;
#15372 = DIRECTION ( 'NONE',  ( -0.000000000000000000, -0.000000000000000000, 1.000000000000000000 ) ) ;
#15373 = CARTESIAN_POINT ( 'NONE',  ( -25.21435515916043713, 23.92354251275973809, 25.00736669480994934 ) ) ;
#15374 = ORIENTED_EDGE ( 'NONE', *, *, #13544, .F. ) ;
#15375 = CARTESIAN_POINT ( 'NONE',  ( 1.893872463202053824, 132.2106029832902720, 59.90695624048730394 ) ) ;
#15376 = CARTESIAN_POINT ( 'NONE',  ( -55.25297051322618813, -0.001818774723748856851, 0.01483298743815036902 ) ) ;
#15377 = CARTESIAN_POINT ( 'NONE',  ( 109.1721716018069657, 0.01550977894512766374, -0.007126480965770760380 ) ) ;
#15378 = CARTESIAN_POINT ( 'NONE',  ( -20.20700224038492721, -27.82980252387826781, -10.08426345511578504 ) ) ;
#15379 = CARTESIAN_POINT ( 'NONE',  ( -25.21435515916043357, -34.29329011225959079, -4.655591116594231416 ) ) ;
#15380 = CARTESIAN_POINT ( 'NONE',  ( 13.36082413113061307, -81.89226687792178438, 129.1512766091118749 ) ) ;
#15381 = CARTESIAN_POINT ( 'NONE',  ( 1.833485406944043827, 132.7804117027896211, -58.53321471326746916 ) ) ;
#15382 = CARTESIAN_POINT ( 'NONE',  ( 25.64692872815576408, -56.17679456083732958, -97.94438212068882876 ) ) ;
#15383 = ORIENTED_EDGE ( 'NONE', *, *, #24594, .T. ) ;
#15384 = B_SPLINE_CURVE_WITH_KNOTS ( 'NONE', 3,
 ( #26648, #15277, #22051, #6962 ),
 .UNSPECIFIED., .F., .F.,
 ( 4, 4 ),
 ( 2.372452373067096320E-16, 0.008383748772659710413 ),
 .UNSPECIFIED. ) ;
#15385 = ORIENTED_EDGE ( 'NONE', *, *, #19235, .T. ) ;
#15386 = ORIENTED_EDGE ( 'NONE', *, *, #11026, .F. ) ;
#15387 = EDGE_CURVE ( 'NONE', #27689, #27511, #20104, .T. ) ;
#15388 = B_SPLINE_CURVE_WITH_KNOTS ( 'NONE', 3,
 ( #12620, #17226, #25607, #26013, #15051, #23874 ),
 .UNSPECIFIED., .F., .F.,
 ( 4, 2, 4 ),
 ( 3.681866292528241208E-16, 0.003576372551511175675, 0.007152745103021982721 ),
 .UNSPECIFIED. ) ;
#15389 = FACE_OUTER_BOUND ( 'NONE', #28116, .T. ) ;
#15390 = FACE_OUTER_BOUND ( 'NONE', #28066, .T. ) ;
#15391 = CARTESIAN_POINT ( 'NONE',  ( -1.583189561560256253, 25.21827308671232615, -38.94740041318302559 ) ) ;
#15392 = ADVANCED_FACE ( 'NONE', ( #24709 ), #668, .F. ) ;
#15393 = VERTEX_POINT ( 'NONE', #925 ) ;
#15394 = CARTESIAN_POINT ( 'NONE',  ( -1.583189561560252701, -36.01941156322808268, -29.24830400313153334 ) ) ;
#15395 = CARTESIAN_POINT ( 'NONE',  ( 2.430230287190589422, 71.49654683843687053, -126.7388733285337281 ) ) ;
#15396 = ORIENTED_EDGE ( 'NONE', *, *, #23790, .T. ) ;
#15397 = CARTESIAN_POINT ( 'NONE',  ( -1.113427685306994652, -25.34053733836502431, 38.22586258295222450 ) ) ;
#15398 = VERTEX_POINT ( 'NONE', #25119 ) ;
#15399 = CARTESIAN_POINT ( 'NONE',  ( -55.24390624410018802, -0.001451500391950358120, -0.01032895241567008057 ) ) ;
#15400 = CARTESIAN_POINT ( 'NONE',  ( -55.24340739397742084, -0.006539691034612123317, 0.007744344507854589339 ) ) ;
#15401 = CARTESIAN_POINT ( 'NONE',  ( 10.93730112725990189, -97.44200844886194091, -115.5857507957714461 ) ) ;
#15402 = CARTESIAN_POINT ( 'NONE',  ( 109.1624594426973118, 0.01531968460306869402, 0.004489871836309402252 ) ) ;
#15403 = CARTESIAN_POINT ( 'NONE',  ( -1.583189561560255143, 29.24830400313165413, -36.01941156322797610 ) ) ;
#15404 = CARTESIAN_POINT ( 'NONE',  ( 28.37599760073042177, 33.74340001061105454, 109.6580863494831135 ) ) ;
#15405 = CARTESIAN_POINT ( 'NONE',  ( -8.786685647604890903, -47.14957014837335691, 25.35688121747554291 ) ) ;
#15406 = CARTESIAN_POINT ( 'NONE',  ( 1.833750490713699444, 14.90257883162752961, 144.3424379351781113 ) ) ;
#15407 = CARTESIAN_POINT ( 'NONE',  ( 109.1586059443104944, -0.005067816690893775511, -0.004935564877218384661 ) ) ;
#15408 = VERTEX_POINT ( 'NONE', #14297 ) ;
#15409 = ORIENTED_EDGE ( 'NONE', *, *, #9554, .F. ) ;
#15410 = CARTESIAN_POINT ( 'NONE',  ( -20.57838717382308502, 23.26537097894105699, -18.89542499756508320 ) ) ;
#15411 = CARTESIAN_POINT ( 'NONE',  ( 25.64660436782546427, 35.44263474731944541, 107.2041192742817088 ) ) ;
#15412 = ORIENTED_EDGE ( 'NONE', *, *, #18312, .T. ) ;
#15413 = EDGE_LOOP ( 'NONE', ( #24549, #24041, #9478, #3895 ) ) ;
#15414 = ORIENTED_EDGE ( 'NONE', *, *, #6446, .F. ) ;
#15415 = ADVANCED_FACE ( 'NONE', ( #24836 ), #27313, .F. ) ;
#15416 = EDGE_CURVE ( 'NONE', #12008, #24090, #19335, .T. ) ;
#15417 = CARTESIAN_POINT ( 'NONE',  ( 25.64681081121879203, -83.63051021305848565, -75.86069728269076506 ) ) ;
#15418 = CARTESIAN_POINT ( 'NONE',  ( 25.64670758986457244, 11.30712635241989794, 112.3434365398308898 ) ) ;
#15419 = EDGE_CURVE ( 'NONE', #11951, #24512, #21624, .T. ) ;
#15420 = LINE ( 'NONE', #15868, #1861 ) ;
#15421 = CARTESIAN_POINT ( 'NONE',  ( 2.433796855181205476, 132.3327394885231456, 60.50726454507948660 ) ) ;
#15422 = CARTESIAN_POINT ( 'NONE',  ( -25.21435515916043713, 30.48034229288662544, 16.39063784838709736 ) ) ;
#15423 = ADVANCED_FACE ( 'NONE', ( #18189 ), #7862, .T. ) ;
#15424 = CARTESIAN_POINT ( 'NONE',  ( -1.323830074806773727, 43.04593525292991529, 16.42382241777492524 ) ) ;
#15425 = CARTESIAN_POINT ( 'NONE',  ( 10.93730112725932635, 1.851405574867327964E-14, 151.1787379149930359 ) ) ;
#15426 = CARTESIAN_POINT ( 'NONE',  ( -8.786685647604890903, -48.22796981442785835, -23.24040270374372952 ) ) ;
#15427 = CARTESIAN_POINT ( 'NONE',  ( -1.046936909428696438, 36.28616897897453697, -27.93981068760634656 ) ) ;
#15428 = CARTESIAN_POINT ( 'NONE',  ( 25.64681081121879203, -35.28660243342475411, -107.2555980796244910 ) ) ;
#15429 = ORIENTED_EDGE ( 'NONE', *, *, #21911, .T. ) ;
#15430 = SHAPE_REPRESENTATION ( 'MAT-025', ( #3866, #8424, #24522, #11665, #17625, #21322 ), #27767 ) ;
#15431 = ORIENTED_EDGE ( 'NONE', *, *, #15584, .T. ) ;
#15433 = CARTESIAN_POINT ( 'NONE',  ( 25.64681081121879203, -66.70335573067806934, -91.10197563708015878 ) ) ;
#15432 = CARTESIAN_POINT ( 'NONE',  ( 25.64700659047694131, 91.21315746821524328, 66.55152787776158618 ) ) ;
#15434 = CARTESIAN_POINT ( 'NONE',  ( 26.11404676487257603, -110.5078194225162918, 24.64483677384812665 ) ) ;
#15435 = FACE_BOUND ( 'NONE', #20584, .T. ) ;
#15436 = CARTESIAN_POINT ( 'NONE',  ( 25.98107933586734575, 110.4296102877914905, 24.58827779736819963 ) ) ;
#15437 = CARTESIAN_POINT ( 'NONE',  ( 109.1587776205901577, 0.005502145856754162359, -0.004842060007774067441 ) ) ;
#15438 = ADVANCED_FACE ( 'NONE', ( #20783 ), #3613, .F. ) ;
#15439 = ORIENTED_EDGE ( 'NONE', *, *, #15313, .F. ) ;
#15440 = CARTESIAN_POINT ( 'NONE',  ( 32.73300124599732186, 0.000000000000000000, 0.000000000000000000 ) ) ;
#15441 = VERTEX_POINT ( 'NONE', #7414 ) ;
#15442 = CARTESIAN_POINT ( 'NONE',  ( 109.1592201516379674, -0.007302213399787572945, -0.002913740842103159506 ) ) ;
#15443 = DIRECTION ( 'NONE',  ( 0.7563875759206389882, -0.03500244528122105347, 0.6531865459554679898 ) ) ;
#15444 = ORIENTED_EDGE ( 'NONE', *, *, #17728, .T. ) ;
#15445 = VERTEX_POINT ( 'NONE', #18769 ) ;
#15446 = CARTESIAN_POINT ( 'NONE',  ( -1.056502255334264895, 13.66916755949850604, -43.72121397317227576 ) ) ;
#15447 =( BOUNDED_SURFACE ( )  B_SPLINE_SURFACE ( 3, 1, ( 
 ( #8195, #3865 ),
 ( #12495, #25888 ),
 ( #19127, #6184 ),
 ( #16958, #1693 ) ),
 .UNSPECIFIED., .F., .F., .F. ) 
 B_SPLINE_SURFACE_WITH_KNOTS ( ( 4, 4 ),
 ( 2, 2 ),
 ( 0.000000000000000000, 1.000000000000000000 ),
 ( 0.000000000000000000, 1.000000000000000000 ),
 .UNSPECIFIED. ) 
 GEOMETRIC_REPRESENTATION_ITEM ( )  RATIONAL_B_SPLINE_SURFACE ( (
 ( 1.000000000000000000, 1.000000000000000000),
 ( 0.6386103224230302855, 0.9954351624131538845),
 ( 0.6386103224230302855, 0.9954351624131538845),
 ( 1.000000000000000000, 1.000000000000000000) ) ) 
 REPRESENTATION_ITEM ( '' )  SURFACE ( )  );
#15448 = EDGE_CURVE ( 'NONE', #17039, #23477, #7090, .T. ) ;
#15449 = ORIENTED_EDGE ( 'NONE', *, *, #19031, .F. ) ;
#15450 = CARTESIAN_POINT ( 'NONE',  ( -12.82751273423877514, -44.03362901246993744, 21.21958768041844579 ) ) ;
#15451 = EDGE_LOOP ( 'NONE', ( #19053, #25370, #3772, #12951 ) ) ;
#15452 = ADVANCED_FACE ( 'NONE', ( #5244 ), #4956, .T. ) ;
#15453 = EDGE_CURVE ( 'NONE', #21625, #9465, #22534, .T. ) ;
#15454 = CARTESIAN_POINT ( 'NONE',  ( 26.11404676487259024, 67.46175819463365997, 90.92995828888226129 ) ) ;
#15455 = ORIENTED_EDGE ( 'NONE', *, *, #2602, .T. ) ;
#15456 = CARTESIAN_POINT ( 'NONE',  ( -55.24300891470648622, -0.009439835024157194193, 0.002702093572889528381 ) ) ;
#15457 = CARTESIAN_POINT ( 'NONE',  ( -1.045287976400351981, -15.59869763335126436, -43.05558670614231431 ) ) ;
#15458 = CARTESIAN_POINT ( 'NONE',  ( 2.430230287190572103, -126.7388733285349787, 71.49654683843465364 ) ) ;
#15459 = CARTESIAN_POINT ( 'NONE',  ( 2.430230287190572103, 71.49654683843509417, 126.7388733285347513 ) ) ;
#15460 = CARTESIAN_POINT ( 'NONE',  ( 30.59141879584282364, 44.78722686469206593, 107.2355637993502029 ) ) ;
#15461 = CARTESIAN_POINT ( 'NONE',  ( 109.1624594426973118, -0.0004639210235603736013, -0.01595733256932006794 ) ) ;
#15463 = CARTESIAN_POINT ( 'NONE',  ( 26.04756280548354397, -33.91579348271593375, 107.9769918539638951 ) ) ;
#15462 = CARTESIAN_POINT ( 'NONE',  ( 109.1592201516379674, 0.007051465909551715011, 0.003476928926125415296 ) ) ;
#15464 = CARTESIAN_POINT ( 'NONE',  ( 25.64699802086723679, -56.24956056770090385, 97.90265915240011907 ) ) ;
#15465 = ORIENTED_EDGE ( 'NONE', *, *, #24597, .F. ) ;
#15466 = CARTESIAN_POINT ( 'NONE',  ( 5.340103579038186332, -96.93942141937377244, 111.1041836885944036 ) ) ;
#15467 = CARTESIAN_POINT ( 'NONE',  ( -55.24198130335446422, -0.009170435128244796077, 0.001516807524704069481 ) ) ;
#15468 = CARTESIAN_POINT ( 'NONE',  ( 26.11404676487257603, -102.9690087468798509, -47.08215554553621729 ) ) ;
#15469 = CARTESIAN_POINT ( 'NONE',  ( 16.75465622695644896, 131.7467602971417762, -53.58152542127552209 ) ) ;
#15470 = CARTESIAN_POINT ( 'NONE',  ( 32.73300124599734318, 114.2056417606548706, 28.19767303745648945 ) ) ;
#15471 = ORIENTED_EDGE ( 'NONE', *, *, #9030, .T. ) ;
#15472 = CARTESIAN_POINT ( 'NONE',  ( 25.64703792032468854, -35.03296646432486483, -107.3388703233125909 ) ) ;
#15473 = CARTESIAN_POINT ( 'NONE',  ( 25.64681081121879203, 112.2483031020013442, 12.21581276189844800 ) ) ;
#15474 = CARTESIAN_POINT ( 'NONE',  ( 1.834118845439484335, 97.22976650547570898, -107.7186227765444642 ) ) ;
#15475 = ORIENTED_EDGE ( 'NONE', *, *, #22610, .F. ) ;
#15476 = CARTESIAN_POINT ( 'NONE',  ( 109.1778270068192853, -0.008236503545668662218, -0.004349865064721219338 ) ) ;
#15477 = EDGE_CURVE ( 'NONE', #27145, #243, #535, .T. ) ;
#15478 =( BOUNDED_SURFACE ( )  B_SPLINE_SURFACE ( 3, 1, ( 
 ( #13174, #24277 ),
 ( #13314, #1814 ),
 ( #21831, #17498 ),
 ( #19243, #12895 ) ),
 .UNSPECIFIED., .F., .F., .F. ) 
 B_SPLINE_SURFACE_WITH_KNOTS ( ( 4, 4 ),
 ( 2, 2 ),
 ( 0.000000000000000000, 1.000000000000000000 ),
 ( 0.000000000000000000, 1.000000000000000000 ),
 .UNSPECIFIED. ) 
 GEOMETRIC_REPRESENTATION_ITEM ( )  RATIONAL_B_SPLINE_SURFACE ( (
 ( 1.000000000000000000, 1.000000000000000000),
 ( 0.6386103224230316178, 0.9954351624131538845),
 ( 0.6386103224230316178, 0.9954351624131538845),
 ( 1.000000000000000000, 1.000000000000000000) ) ) 
 REPRESENTATION_ITEM ( '' )  SURFACE ( )  );
#15479 = ADVANCED_FACE ( 'NONE', ( #1634 ), #4703, .F. ) ;
#15480 = CARTESIAN_POINT ( 'NONE',  ( 1.833838850855463720, -97.16351016225966930, 107.7780290788693947 ) ) ;
#15481 = ORIENTED_EDGE ( 'NONE', *, *, #25590, .F. ) ;
#15482 = CARTESIAN_POINT ( 'NONE',  ( -55.25297051322618813, 0.01354497706059944184, 0.006313402748433108967 ) ) ;
#15483 = CARTESIAN_POINT ( 'NONE',  ( 30.59141879584321444, 95.58042137919564141, -66.10404588653692315 ) ) ;
#15484 = VERTEX_POINT ( 'NONE', #12571 ) ;
#15485 = B_SPLINE_CURVE_WITH_KNOTS ( 'NONE', 3,
 ( #11605, #11039, #19802, #2530, #26706, #95, #18074 ),
 .UNSPECIFIED., .F., .F.,
 ( 4, 3, 4 ),
 ( 5.916500692592983104E-16, 0.02816610861753241976, 0.04000277880656278456 ),
 .UNSPECIFIED. ) ;
#15486 = CARTESIAN_POINT ( 'NONE',  ( 32.73300124599735739, -105.8473486001054482, 51.32617430724869223 ) ) ;
#15487 = DIRECTION ( 'NONE',  ( 0.000000000000000000, 1.000000000000000000, -6.938893903907228378E-16 ) ) ;
#15488 = CARTESIAN_POINT ( 'NONE',  ( 25.64708010899963497, 23.52908206539902025, 110.4325102642035574 ) ) ;
#15489 = FACE_OUTER_BOUND ( 'NONE', #794, .T. ) ;
#15490 = CARTESIAN_POINT ( 'NONE',  ( -55.25297051322618813, -0.002853887643043501524, -0.01466904165775538733 ) ) ;
#15491 = EDGE_LOOP ( 'NONE', ( #9473, #10511, #17609, #18272, #24224, #17403 ) ) ;
#15492 = CARTESIAN_POINT ( 'NONE',  ( 9.884929003653626367, -103.8128997986850095, -109.0134320167743880 ) ) ;
#15493 = EDGE_CURVE ( 'NONE', #26221, #9758, #5714, .T. ) ;
#15494 = CARTESIAN_POINT ( 'NONE',  ( -12.82751273423878047, -8.715310691359913875, 48.09651489336692975 ) ) ;
#15495 = CARTESIAN_POINT ( 'NONE',  ( 25.87036335909428075, -46.88819766600042271, -102.8789780196093204 ) ) ;
#15496 = CARTESIAN_POINT ( 'NONE',  ( 25.81918753295377655, -98.34688456803354484, -55.70247894228274532 ) ) ;
#15497 = VERTEX_POINT ( 'NONE', #5686 ) ;
#15498 = ORIENTED_EDGE ( 'NONE', *, *, #27288, .T. ) ;
#15499 = ORIENTED_EDGE ( 'NONE', *, *, #21119, .T. ) ;
#15500 = ORIENTED_EDGE ( 'NONE', *, *, #12642, .F. ) ;
#15501 = CARTESIAN_POINT ( 'NONE',  ( -1.048994561756799060, -26.29622118251707619, -37.49601524795400564 ) ) ;
#15502 = DIRECTION ( 'NONE',  ( 0.7637818620346800147, -0.3617919495470791613, -0.5345501402766260624 ) ) ;
#15503 = CARTESIAN_POINT ( 'NONE',  ( -1.619063947482197729, 2.489035965910801895, 46.30105812165545842 ) ) ;
#15504 = CARTESIAN_POINT ( 'NONE',  ( 109.1589550718174877, 0.006669585340466646639, -0.003591809816105017393 ) ) ;
#15505 = CARTESIAN_POINT ( 'NONE',  ( 1.833485406944057594, 59.50871042846225834, 132.3460930279893262 ) ) ;
#15506 = CARTESIAN_POINT ( 'NONE',  ( 109.1587776205901861, -0.005502145856762338978, -0.004842060007769368075 ) ) ;
#15507 = ORIENTED_EDGE ( 'NONE', *, *, #5946, .F. ) ;
#15508 = CARTESIAN_POINT ( 'NONE',  ( 25.73574536432414916, -34.14219540448061707, -107.6875787074510811 ) ) ;
#15509 = CARTESIAN_POINT ( 'NONE',  ( 1.833485406944043827, -117.7091014914955309, 84.86072343962528919 ) ) ;
#15510 = CARTESIAN_POINT ( 'NONE',  ( 2.433796855181205476, -57.85512797797802165, -133.5135467655523769 ) ) ;
#15511 = EDGE_CURVE ( 'NONE', #10615, #23186, #26985, .T. ) ;
#15512 = CARTESIAN_POINT ( 'NONE',  ( -1.056502255334264895, -37.35734037467652513, -26.51074901220491498 ) ) ;
#15513 = ADVANCED_FACE ( 'NONE', ( #23255 ), #5538, .T. ) ;
#15515 = CARTESIAN_POINT ( 'NONE',  ( 25.86096068574578766, -74.90357932134571683, -84.67961880569373534 ) ) ;
#15514 = B_SPLINE_CURVE_WITH_KNOTS ( 'NONE', 3,
 ( #1575, #25903, #12779, #25497 ),
 .UNSPECIFIED., .F., .F.,
 ( 4, 4 ),
 ( 0.000000000000000000, 0.008383560773332736360 ),
 .UNSPECIFIED. ) ;
#15516 = CARTESIAN_POINT ( 'NONE',  ( -8.786685647604931759, 47.14957014837394667, 25.35688121747446999 ) ) ;
#15518 = EDGE_CURVE ( 'NONE', #21137, #19603, #21139, .T. ) ;
#15517 = DIRECTION ( 'NONE',  ( -1.000000000000000000, -0.000000000000000000, -0.000000000000000000 ) ) ;
#15519 = CARTESIAN_POINT ( 'NONE',  ( -55.24390624410018802, -0.01032895241566962087, 0.001451500391950532459 ) ) ;
#15520 = ORIENTED_EDGE ( 'NONE', *, *, #25554, .F. ) ;
#15521 = EDGE_CURVE ( 'NONE', #864, #12683, #26279, .T. ) ;
#15522 = ORIENTED_EDGE ( 'NONE', *, *, #25822, .T. ) ;
#15523 = ORIENTED_EDGE ( 'NONE', *, *, #16485, .F. ) ;
#15524 = CARTESIAN_POINT ( 'NONE',  ( 6.224689322667630975, 111.7293398381277569, -97.14981701196212782 ) ) ;
#15525 =( BOUNDED_SURFACE ( )  B_SPLINE_SURFACE ( 3, 1, ( 
 ( #2369, #19948 ),
 ( #228, #17777 ),
 ( #26006, #7008 ),
 ( #22841, #20510 ) ),
 .UNSPECIFIED., .F., .F., .F. ) 
 B_SPLINE_SURFACE_WITH_KNOTS ( ( 4, 4 ),
 ( 2, 2 ),
 ( 0.000000000000000000, 1.000000000000000000 ),
 ( 0.000000000000000000, 1.000000000000000000 ),
 .UNSPECIFIED. ) 
 GEOMETRIC_REPRESENTATION_ITEM ( )  RATIONAL_B_SPLINE_SURFACE ( (
 ( 1.000000000000000000, 1.000000000000000000),
 ( 0.9956975270656955868, 0.8568959468854907557),
 ( 0.9956975270656955868, 0.8568959468854907557),
 ( 1.000000000000000000, 1.000000000000000000) ) ) 
 REPRESENTATION_ITEM ( '' )  SURFACE ( )  );
#15526 = CARTESIAN_POINT ( 'NONE',  ( -55.24390624410018802, -0.007503127514277506058, -0.007245494385991484328 ) ) ;
#15527 = CARTESIAN_POINT ( 'NONE',  ( -55.24340739397742794, 0.01010924026184123470, -0.0007387096945706978770 ) ) ;
#15528 = ORIENTED_EDGE ( 'NONE', *, *, #26987, .T. ) ;
#15529 = CARTESIAN_POINT ( 'NONE',  ( 99.22246935314075245, -69.99999999999998579, 40.00000000000003553 ) ) ;
#15530 = CARTESIAN_POINT ( 'NONE',  ( -1.155001620486249214, -12.20337535396710749, -44.25209926692303952 ) ) ;
#15531 = VERTEX_POINT ( 'NONE', #28104 ) ;
#15532 = LINE ( 'NONE', #20679, #20322 ) ;
#15533 = ORIENTED_EDGE ( 'NONE', *, *, #10963, .F. ) ;
#15534 = DIRECTION ( 'NONE',  ( -0.5946245182733608248, 0.7356888587241636746, 0.3243201896541614282 ) ) ;
#15535 = CARTESIAN_POINT ( 'NONE',  ( 55.79472521941428198, 15.83764557006269946, 71.00924468211162832 ) ) ;
#15536 = B_SPLINE_CURVE_WITH_KNOTS ( 'NONE', 3,
 ( #12374, #7951, #18718, #5780, #5477, #16714 ),
 .UNSPECIFIED., .F., .F.,
 ( 4, 2, 4 ),
 ( 2.168404344971008868E-18, 0.0006311636237756631899, 0.001262327247551324211 ),
 .UNSPECIFIED. ) ;
#15537 = CARTESIAN_POINT ( 'NONE',  ( 55.79472521941428198, -62.63970324008288770, 37.00555938668237133 ) ) ;
#15538 = CARTESIAN_POINT ( 'NONE',  ( 2.108985857320909929, 73.75356715683084019, 125.1820688103224342 ) ) ;
#15539 = CARTESIAN_POINT ( 'NONE',  ( 109.1587776205901577, -8.330235397649874362E-05, 0.007328861771496576576 ) ) ;
#15540 = CARTESIAN_POINT ( 'NONE',  ( 25.64681081121879203, -23.06870491922242650, -110.5293738517610933 ) ) ;
#15541 = CARTESIAN_POINT ( 'NONE',  ( -1.619063947482197729, -25.20140673341401438, -38.92136151114898723 ) ) ;
#15542 = ADVANCED_FACE ( 'NONE', ( #17173 ), #6557, .F. ) ;
#15543 = DIRECTION ( 'NONE',  ( 0.000000000000000000, 0.000000000000000000, 1.000000000000000000 ) ) ;
#15544 = CARTESIAN_POINT ( 'NONE',  ( 25.64681081121879203, -66.70335573067929147, 91.10197563707923507 ) ) ;
#15545 = CARTESIAN_POINT ( 'NONE',  ( -1.019300379054419725, -38.21680004809182662, -25.26451264419630860 ) ) ;
#15546 = VERTEX_POINT ( 'NONE', #10152 ) ;
#15547 = AXIS2_PLACEMENT_3D ( 'NONE', #25642, #7952, #25204 ) ;
#15548 = VERTEX_POINT ( 'NONE', #18921 ) ;
#15550 = EDGE_CURVE ( 'NONE', #24539, #5490, #18298, .T. ) ;
#15549 = CARTESIAN_POINT ( 'NONE',  ( -1.045287976400365970, 44.00138577190666922, 12.68782741917247670 ) ) ;
#15551 = CARTESIAN_POINT ( 'NONE',  ( -1.048171036023513025, 45.78635789057865679, 1.020520027229292470 ) ) ;
#15552 = ORIENTED_EDGE ( 'NONE', *, *, #1633, .T. ) ;
#15553 = ORIENTED_EDGE ( 'NONE', *, *, #22131, .F. ) ;
#15554 = ORIENTED_EDGE ( 'NONE', *, *, #21352, .T. ) ;
#15555 = CARTESIAN_POINT ( 'NONE',  ( -20.57838717382308147, -1.611677988432568709, -29.92853265176830746 ) ) ;
#15556 = B_SPLINE_CURVE_WITH_KNOTS ( 'NONE', 3,
 ( #25534, #18464, #27232, #5813, #3627, #7546 ),
 .UNSPECIFIED., .F., .F.,
 ( 4, 2, 4 ),
 ( 4.296969928001729735E-16, 0.003576372551511233788, 0.007152745103022037365 ),
 .UNSPECIFIED. ) ;
#15557 = CARTESIAN_POINT ( 'NONE',  ( 1.833809397773845218, 137.9524943416725478, 45.01060836636568041 ) ) ;
#15558 =( BOUNDED_SURFACE ( )  B_SPLINE_SURFACE ( 3, 1, ( 
 ( #22009, #24186 ),
 ( #4444, #13790 ),
 ( #24470, #843 ),
 ( #11794, #4736 ) ),
 .UNSPECIFIED., .F., .F., .F. ) 
 B_SPLINE_SURFACE_WITH_KNOTS ( ( 4, 4 ),
 ( 2, 2 ),
 ( 0.000000000000000000, 1.000000000000000000 ),
 ( 0.000000000000000000, 1.000000000000000000 ),
 .UNSPECIFIED. ) 
 GEOMETRIC_REPRESENTATION_ITEM ( )  RATIONAL_B_SPLINE_SURFACE ( (
 ( 1.000000000000000000, 1.000000000000000000),
 ( 0.6386103224230302855, 0.9954351624131538845),
 ( 0.6386103224230302855, 0.9954351624131538845),
 ( 1.000000000000000000, 1.000000000000000000) ) ) 
 REPRESENTATION_ITEM ( '' )  SURFACE ( )  );
#15559 = B_SPLINE_CURVE_WITH_KNOTS ( 'NONE', 3,
 ( #7867, #5696, #23265, #21069, #14598, #23401, #8954, #20155, #15011, #1773 ),
 .UNSPECIFIED., .F., .F.,
 ( 4, 3, 3, 4 ),
 ( 1.387778780781445676E-17, 0.0002669559177086280378, 0.0005339118354151154268, 0.001067817517169168152 ),
 .UNSPECIFIED. ) ;
#15560 = CARTESIAN_POINT ( 'NONE',  ( -1.583189561560255143, -44.83405390829663872, 11.94859433442949381 ) ) ;
#15561 = CARTESIAN_POINT ( 'NONE',  ( -20.20612091757427109, -16.46550228026411844, -24.59769958242381094 ) ) ;
#15562 = VECTOR ( 'NONE', #28055, 1000.000000000000000 ) ;
#15563 = CARTESIAN_POINT ( 'NONE',  ( 1.894214914920941961, 43.94587946447585125, -138.3376769255504541 ) ) ;
#15564 = DIRECTION ( 'NONE',  ( 1.000000000000000000, -6.938893903907226837E-18, 1.734723475976806709E-18 ) ) ;
#15565 = CARTESIAN_POINT ( 'NONE',  ( -1.539763995773681282, 43.19716353142356269, 16.63252574782999460 ) ) ;
#15566 = LINE ( 'NONE', #13273, #20862 ) ;
#15567 = CARTESIAN_POINT ( 'NONE',  ( 30.58324630866340499, 113.7441547345752468, -41.10517620771084779 ) ) ;
#15568 = CARTESIAN_POINT ( 'NONE',  ( 109.1586900883932856, 0.003656351050324885277, -0.006130969560693676386 ) ) ;
#15569 = CARTESIAN_POINT ( 'NONE',  ( -1.583189561560252701, -29.24830400313139478, 36.01941156322819637 ) ) ;
#15570 = VERTEX_POINT ( 'NONE', #18462 ) ;
#15571 = CARTESIAN_POINT ( 'NONE',  ( -55.24271866751342941, -0.004256484107795216812, 0.008488649505342837909 ) ) ;
#15572 = EDGE_CURVE ( 'NONE', #23252, #27866, #2624, .T. ) ;
#15573 = CARTESIAN_POINT ( 'NONE',  ( 25.86096068574579121, -22.52859312382108214, -110.7864907291861556 ) ) ;
#15574 = CARTESIAN_POINT ( 'NONE',  ( -55.24198130335446422, 0.006527480770976314475, -0.006617369590168970667 ) ) ;
#15575 = CARTESIAN_POINT ( 'NONE',  ( 30.58324630866344052, -77.95273942827404312, 92.47020419020155657 ) ) ;
#15576 = ORIENTED_EDGE ( 'NONE', *, *, #23329, .T. ) ;
#15577 = CARTESIAN_POINT ( 'NONE',  ( -1.239374126674604337, -16.50008610789329921, -42.99367564261275021 ) ) ;
#15578 = ORIENTED_EDGE ( 'NONE', *, *, #26475, .F. ) ;
#15580 = ADVANCED_FACE ( 'NONE', ( #759 ), #26222, .T. ) ;
#15579 = CARTESIAN_POINT ( 'NONE',  ( -20.20700224038492721, -29.58392382092672790, 0.9908225410481621420 ) ) ;
#15581 = CARTESIAN_POINT ( 'NONE',  ( 26.11404676487256893, -12.95861723607530003, 112.4785329405481349 ) ) ;
#15582 = ORIENTED_EDGE ( 'NONE', *, *, #16054, .T. ) ;
#15583 = VERTEX_POINT ( 'NONE', #27230 ) ;
#15584 = EDGE_CURVE ( 'NONE', #11640, #20199, #7816, .T. ) ;
#15585 = DIRECTION ( 'NONE',  ( 0.000000000000000000, 0.000000000000000000, 1.000000000000000000 ) ) ;
#15586 = ORIENTED_EDGE ( 'NONE', *, *, #26601, .T. ) ;
#15587 = CARTESIAN_POINT ( 'NONE',  ( 30.59138290137915206, 92.40465044710842335, -70.47507990428483993 ) ) ;
#15588 = VERTEX_POINT ( 'NONE', #13705 ) ;
#15589 = CARTESIAN_POINT ( 'NONE',  ( 25.98552792386801258, 67.36997957637663603, 90.89136171349112203 ) ) ;
#15590 = EDGE_CURVE ( 'NONE', #7066, #18960, #14127, .T. ) ;
#15591 = LINE ( 'NONE', #13302, #20725 ) ;
#15592 =( BOUNDED_SURFACE ( )  B_SPLINE_SURFACE ( 3, 1, ( 
 ( #11729, #12015 ),
 ( #20787, #1079 ),
 ( #9866, #27407 ),
 ( #27700, #1215 ) ),
 .UNSPECIFIED., .F., .F., .F. ) 
 B_SPLINE_SURFACE_WITH_KNOTS ( ( 4, 4 ),
 ( 2, 2 ),
 ( 0.000000000000000000, 1.000000000000000000 ),
 ( 0.000000000000000000, 1.000000000000000000 ),
 .UNSPECIFIED. ) 
 GEOMETRIC_REPRESENTATION_ITEM ( )  RATIONAL_B_SPLINE_SURFACE ( (
 ( 1.000000000000000000, 1.000000000000000000),
 ( 0.9593753223639863714, 0.9995975284513187731),
 ( 0.9593753223639863714, 0.9995975284513187731),
 ( 1.000000000000000000, 1.000000000000000000) ) ) 
 REPRESENTATION_ITEM ( '' )  SURFACE ( )  );
#15593 = CARTESIAN_POINT ( 'NONE',  ( 26.11404676487257603, 112.7148551500681890, -10.71016160607451262 ) ) ;
#15594 = CARTESIAN_POINT ( 'NONE',  ( -1.583189561560255143, -29.24830400313138767, 36.01941156322820348 ) ) ;
#15595 = EDGE_CURVE ( 'NONE', #22601, #13932, #7690, .T. ) ;
#15596 = CARTESIAN_POINT ( 'NONE',  ( -21.41427618760457463, -23.81423075802597111, -19.54551635498120277 ) ) ;
#15597 = CARTESIAN_POINT ( 'NONE',  ( -20.47566262905010248, -29.82700878811085232, -1.586617686065453725 ) ) ;
#15598 = CARTESIAN_POINT ( 'NONE',  ( -55.24340739397742794, -0.002421372372456151618, 0.009842732675348802793 ) ) ;
#15600 = ORIENTED_EDGE ( 'NONE', *, *, #11341, .T. ) ;
#15599 = B_SPLINE_CURVE_WITH_KNOTS ( 'NONE', 3,
 ( #12794, #22002, #1717, #11068, #10930, #10798 ),
 .UNSPECIFIED., .F., .F.,
 ( 4, 2, 4 ),
 ( 4.336808689942017736E-19, 0.0006311571484586052470, 0.001262314296917210060 ),
 .UNSPECIFIED. ) ;
#15601 = CARTESIAN_POINT ( 'NONE',  ( 26.04756280548352620, 83.36043467252123662, -76.55292122839955482 ) ) ;
#15602 = CARTESIAN_POINT ( 'NONE',  ( -20.20700224038492721, -29.58392382092672790, 0.9908225410481621420 ) ) ;
#15603 = EDGE_CURVE ( 'NONE', #7969, #8336, #18020, .T. ) ;
#15604 = CARTESIAN_POINT ( 'NONE',  ( 1.831572820252009626, -43.90210991190716072, 138.3111855986059595 ) ) ;
#15605 = CARTESIAN_POINT ( 'NONE',  ( -4.162674018437141576, 18.33413805792438112, -45.34593312138888876 ) ) ;
#15606 =( BOUNDED_SURFACE ( )  B_SPLINE_SURFACE ( 3, 1, ( 
 ( #15613, #24435 ),
 ( #12906, #4702 ),
 ( #13471, #21697 ),
 ( #22269, #2532 ) ),
 .UNSPECIFIED., .F., .F., .F. ) 
 B_SPLINE_SURFACE_WITH_KNOTS ( ( 4, 4 ),
 ( 2, 2 ),
 ( 0.000000000000000000, 1.000000000000000000 ),
 ( 0.000000000000000000, 1.000000000000000000 ),
 .UNSPECIFIED. ) 
 GEOMETRIC_REPRESENTATION_ITEM ( )  RATIONAL_B_SPLINE_SURFACE ( (
 ( 1.000000000000000000, 1.000000000000000000),
 ( 0.9960225298536222738, 0.9999952330161893110),
 ( 0.9960225298536222738, 0.9999952330161893110),
 ( 1.000000000000000000, 1.000000000000000000) ) ) 
 REPRESENTATION_ITEM ( '' )  SURFACE ( )  );
#15607 = ORIENTED_EDGE ( 'NONE', *, *, #21752, .F. ) ;
#15608 = CARTESIAN_POINT ( 'NONE',  ( -1.539763995773694827, 16.63252574783043869, -43.19716353142335663 ) ) ;
#15609 = CARTESIAN_POINT ( 'NONE',  ( 19.66333377628710366, -51.89484018353753214, -127.6002314355563243 ) ) ;
#15610 = DIRECTION ( 'NONE',  ( -0.5946245182733608248, -0.3243201896541638707, 0.7356888587241625643 ) ) ;
#15611 = CARTESIAN_POINT ( 'NONE',  ( 32.73300124599735739, -39.98094346392385745, 110.6325518752272501 ) ) ;
#15612 = VERTEX_POINT ( 'NONE', #26807 ) ;
#15613 = CARTESIAN_POINT ( 'NONE',  ( 109.1586900883932856, 0.007088091345229654248, -0.0008465529156635364033 ) ) ;
#15614 = VECTOR ( 'NONE', #9960, 1000.000000000000114 ) ;
#15615 = B_SPLINE_CURVE_WITH_KNOTS ( 'NONE', 3,
 ( #10131, #12691, #8117, #18901, #25535, #10547, #14573, #27819, #19310, #3628 ),
 .UNSPECIFIED., .F., .F.,
 ( 4, 3, 3, 4 ),
 ( 1.040834085586084257E-17, 0.0002669560319015743151, 0.0005492286108966385264, 0.0008315040496093428378 ),
 .UNSPECIFIED. ) ;
#15616 = CARTESIAN_POINT ( 'NONE',  ( -1.259972190295308714, -35.85909728507027694, 28.82609802125297449 ) ) ;
#15617 = VECTOR ( 'NONE', #15905, 1000.000000000000114 ) ;
#15618 = ORIENTED_EDGE ( 'NONE', *, *, #2253, .T. ) ;
#15619 = CARTESIAN_POINT ( 'NONE',  ( 13.36082413113061307, 84.67697637120410548, 127.3428651193251113 ) ) ;
#15620 = CARTESIAN_POINT ( 'NONE',  ( 55.79472521941428198, 14.41365263906652139, -71.31192372336661833 ) ) ;
#15621 = CARTESIAN_POINT ( 'NONE',  ( 24.22246935314087324, 70.00000000000004263, 39.99999999999999289 ) ) ;
#15622 = ORIENTED_EDGE ( 'NONE', *, *, #9380, .F. ) ;
#15623 = DIRECTION ( 'NONE',  ( 1.000000000000000000, 0.000000000000000000, 0.000000000000000000 ) ) ;
#15624 = DIRECTION ( 'NONE',  ( 0.5914120900931444380, 0.07630783613000277632, 0.8027508043202542520 ) ) ;
#15625 = CARTESIAN_POINT ( 'NONE',  ( 25.64700659047694131, -35.10784848926738988, 107.3144208978484073 ) ) ;
#15626 = CARTESIAN_POINT ( 'NONE',  ( 25.64703792032469210, 23.62108504469244963, 110.4127989088530910 ) ) ;
#15627 = CARTESIAN_POINT ( 'NONE',  ( 26.11404676487257603, -74.91683232330916553, -84.89295829319569009 ) ) ;
#15628 = CARTESIAN_POINT ( 'NONE',  ( 1.833485406944057594, -125.4007332306550921, 73.01664920992921282 ) ) ;
#15629 = ORIENTED_EDGE ( 'NONE', *, *, #19363, .F. ) ;
#15630 = FACE_OUTER_BOUND ( 'NONE', #21597, .T. ) ;
#15631 = EDGE_CURVE ( 'NONE', #600, #20457, #15874, .T. ) ;
#15632 = CARTESIAN_POINT ( 'NONE',  ( -1.583189561560253589, -38.94740041318312507, -25.21827308671218049 ) ) ;
#15633 = CARTESIAN_POINT ( 'NONE',  ( 25.64660436782550335, 34.33930645842144003, -107.5626123667555731 ) ) ;
#15634 = CARTESIAN_POINT ( 'NONE',  ( -5.986830583229478364, 19.95149887249920440, 46.64941882410778362 ) ) ;
#15635 = ORIENTED_EDGE ( 'NONE', *, *, #15828, .T. ) ;
#15636 = ADVANCED_FACE ( 'NONE', ( #21038 ), #14275, .T. ) ;
#15637 = AXIS2_PLACEMENT_3D ( 'NONE', #20194, #15736, #24698 ) ;
#15638 = ORIENTED_EDGE ( 'NONE', *, *, #11941, .T. ) ;
#15639 = ORIENTED_EDGE ( 'NONE', *, *, #27615, .T. ) ;
#15640 = CARTESIAN_POINT ( 'NONE',  ( -1.050231094221204753, -43.47885872350344982, 14.39477892760344879 ) ) ;
#15641 = CARTESIAN_POINT ( 'NONE',  ( 26.11404676487257603, 67.46175819463486789, -90.92995828888132337 ) ) ;
#15642 = CARTESIAN_POINT ( 'NONE',  ( -22.23226125620929139, -2.179935373562669643, -31.55376588768476509 ) ) ;
#15643 = CIRCLE ( 'NONE', #27606, 34.60786435723138510 ) ;
#15644 = EDGE_CURVE ( 'NONE', #3087, #8562, #16731, .T. ) ;
#15645 = FACE_OUTER_BOUND ( 'NONE', #22639, .T. ) ;
#15646 = B_SPLINE_CURVE_WITH_KNOTS ( 'NONE', 3,
 ( #2366, #15463, #6855, #11444, #20506, #24415, #13737, #792 ),
 .UNSPECIFIED., .F., .F.,
 ( 4, 2, 2, 4 ),
 ( 6.938893903907228378E-18, 0.0002429592666046760283, 0.0004859185332093451178, 0.0009718370664186966323 ),
 .UNSPECIFIED. ) ;
#15647 = CARTESIAN_POINT ( 'NONE',  ( 94.22246935314088034, -90.00000000000005684, 12.49999999999999467 ) ) ;
#15648 = CARTESIAN_POINT ( 'NONE',  ( -4.780792508754331038, -49.38761389561005188, -3.764354093953405922 ) ) ;
#15649 = CARTESIAN_POINT ( 'NONE',  ( 16.75465622695678647, -117.7275519421679633, 79.80233222761944489 ) ) ;
#15650 = ORIENTED_EDGE ( 'NONE', *, *, #7445, .T. ) ;
#15651 = CARTESIAN_POINT ( 'NONE',  ( -1.619063947482197729, 46.30105812165548684, -2.489035965910316506 ) ) ;
#15652 = DIRECTION ( 'NONE',  ( 1.000000000000000000, -6.938893903907226837E-18, 1.734723475976806709E-18 ) ) ;
#15654 = AXIS2_PLACEMENT_3D ( 'NONE', #10891, #23868, #26420 ) ;
#15653 =( BOUNDED_SURFACE ( )  B_SPLINE_SURFACE ( 3, 1, ( 
 ( #27115, #20931 ),
 ( #16477, #10017 ),
 ( #16188, #3514 ),
 ( #18777, #14024 ) ),
 .UNSPECIFIED., .F., .F., .F. ) 
 B_SPLINE_SURFACE_WITH_KNOTS ( ( 4, 4 ),
 ( 2, 2 ),
 ( 0.000000000000000000, 1.000000000000000000 ),
 ( 0.000000000000000000, 1.000000000000000000 ),
 .UNSPECIFIED. ) 
 GEOMETRIC_REPRESENTATION_ITEM ( )  RATIONAL_B_SPLINE_SURFACE ( (
 ( 1.000000000000000000, 1.000000000000000000),
 ( 0.9956975270656955868, 0.8568959468854907557),
 ( 0.9956975270656955868, 0.8568959468854907557),
 ( 1.000000000000000000, 1.000000000000000000) ) ) 
 REPRESENTATION_ITEM ( '' )  SURFACE ( )  );
#15655 = CARTESIAN_POINT ( 'NONE',  ( 1.833485406944057594, -145.1085452359073429, 0.5339064996879626657 ) ) ;
#15656 = CARTESIAN_POINT ( 'NONE',  ( 32.73300124599734318, 108.9684813982489118, 44.31599526637995012 ) ) ;
#15657 = CARTESIAN_POINT ( 'NONE',  ( 26.11404676487257603, 102.9690087468801352, 47.08215554553553517 ) ) ;
#15658 = ORIENTED_EDGE ( 'NONE', *, *, #13841, .T. ) ;
#15659 = CARTESIAN_POINT ( 'NONE',  ( 109.1624594426973118, -0.01102230012606818417, -0.01154818537151451434 ) ) ;
#15660 = B_SPLINE_CURVE_WITH_KNOTS ( 'NONE', 3,
 ( #18786, #7874, #3521, #25276, #16633, #27123 ),
 .UNSPECIFIED., .F., .F.,
 ( 4, 2, 4 ),
 ( 0.000000000000000000, 0.0004335151646191514122, 0.0008670303292383013064 ),
 .UNSPECIFIED. ) ;
#15661 = VERTEX_POINT ( 'NONE', #14704 ) ;
#15662 = DIRECTION ( 'NONE',  ( -1.000000000000000000, -0.000000000000000000, -0.000000000000000000 ) ) ;
#15663 = CARTESIAN_POINT ( 'NONE',  ( -55.25297051322618813, -0.01093108995495129139, -0.01019003092403723831 ) ) ;
#15664 = ORIENTED_EDGE ( 'NONE', *, *, #24154, .T. ) ;
#15665 = VERTEX_POINT ( 'NONE', #23513 ) ;
#15666 = ORIENTED_EDGE ( 'NONE', *, *, #19555, .F. ) ;
#15667 = VECTOR ( 'NONE', #11094, 1000.000000000000000 ) ;
#15668 = CIRCLE ( 'NONE', #5560, 34.60786435723138510 ) ;
#15669 = B_SPLINE_CURVE_WITH_KNOTS ( 'NONE', 3,
 ( #15347, #24438, #11187, #4279 ),
 .UNSPECIFIED., .F., .F.,
 ( 4, 4 ),
 ( 5.513692426328523236E-16, 0.008383748772660020929 ),
 .UNSPECIFIED. ) ;
#15670 = CARTESIAN_POINT ( 'NONE',  ( 32.73300124599735739, -32.68291970228314369, 113.0038235389601340 ) ) ;
#15671 = CARTESIAN_POINT ( 'NONE',  ( 25.81918753295378011, 84.61657260023643801, 74.93271318951751425 ) ) ;
#15672 = CARTESIAN_POINT ( 'NONE',  ( -1.583189561560256253, -44.83405390829680215, -11.94859433442884900 ) ) ;
#15673 = AXIS2_PLACEMENT_3D ( 'NONE', #10173, #3669, #12176 ) ;
#15674 = EDGE_CURVE ( 'NONE', #15769, #1484, #3604, .T. ) ;
#15675 = ORIENTED_EDGE ( 'NONE', *, *, #13731, .T. ) ;
#15676 = CARTESIAN_POINT ( 'NONE',  ( -12.94347594948482083, 21.16159467081353540, -43.91326021875521946 ) ) ;
#15677 = DIRECTION ( 'NONE',  ( 0.5914120900931444380, -0.6570486713847307758, 0.4674599267565279770 ) ) ;
#15678 = VERTEX_POINT ( 'NONE', #7833 ) ;
#15679 = EDGE_CURVE ( 'NONE', #12673, #20443, #16658, .T. ) ;
#15680 = CARTESIAN_POINT ( 'NONE',  ( 25.98552792386800547, 92.15963349013364336, 65.62435323276200450 ) ) ;
#15681 = VERTEX_POINT ( 'NONE', #5272 ) ;
#15682 = CARTESIAN_POINT ( 'NONE',  ( 2.263178607246661755, 126.6115608827437455, 71.48082837426046865 ) ) ;
#15683 = CARTESIAN_POINT ( 'NONE',  ( -1.048171036023494596, -37.64178826568587510, 26.08692787913908617 ) ) ;
#15684 = CARTESIAN_POINT ( 'NONE',  ( 1.832998868059890096, -144.2584710144579390, -15.69902610990519776 ) ) ;
#15685 = CARTESIAN_POINT ( 'NONE',  ( 1.893872463202051604, 96.41404152942938310, 108.5026245911422222 ) ) ;
#15686 = CARTESIAN_POINT ( 'NONE',  ( -1.058473599757806971, -12.47539220917832914, 44.07591602137168252 ) ) ;
#15687 = CARTESIAN_POINT ( 'NONE',  ( -20.57838717382308147, 29.92853265176831812, 1.611677988432465014 ) ) ;
#15688 = EDGE_CURVE ( 'NONE', #1116, #5458, #11758, .T. ) ;
#15689 = CARTESIAN_POINT ( 'NONE',  ( 109.1624594426973118, 0.01503296564241277805, -0.005372302061316116054 ) ) ;
#15690 = CARTESIAN_POINT ( 'NONE',  ( -20.57838717382308147, -7.715628353033481268, 28.96176188950225949 ) ) ;
#15691 = VECTOR ( 'NONE', #3814, 1000.000000000000227 ) ;
#15692 = B_SPLINE_CURVE_WITH_KNOTS ( 'NONE', 3,
 ( #6860, #26285, #19526, #15470 ),
 .UNSPECIFIED., .F., .F.,
 ( 4, 4 ),
 ( 0.000000000000000000, 0.008383560773332725952 ),
 .UNSPECIFIED. ) ;
#15693 = CARTESIAN_POINT ( 'NONE',  ( -8.786685647604890903, -47.14957014837335691, 25.35688121747554291 ) ) ;
#15694 = CARTESIAN_POINT ( 'NONE',  ( -55.24198130335446422, -0.001516807524703878444, -0.009170435128245257514 ) ) ;
#15695 = CARTESIAN_POINT ( 'NONE',  ( 1.833206310202347256, -44.13245377365727506, 138.2356391007181173 ) ) ;
#15696 = CARTESIAN_POINT ( 'NONE',  ( -22.23226125620929139, 2.179935373562892131, 31.55376588768475798 ) ) ;
#15697 = ORIENTED_EDGE ( 'NONE', *, *, #11773, .F. ) ;
#15698 = AXIS2_PLACEMENT_3D ( 'NONE', #1326, #1611, #16744 ) ;
#15699 = VERTEX_POINT ( 'NONE', #13754 ) ;
#15700 = CARTESIAN_POINT ( 'NONE',  ( -1.113427685307007975, 44.18561238466754304, 12.28784199929889098 ) ) ;
#15701 = ORIENTED_EDGE ( 'NONE', *, *, #17643, .T. ) ;
#15702 =( BOUNDED_SURFACE ( )  B_SPLINE_SURFACE ( 3, 1, ( 
 ( #3683, #12460 ),
 ( #25581, #1527 ),
 ( #16653, #1107 ),
 ( #25446, #18663 ) ),
 .UNSPECIFIED., .F., .F., .F. ) 
 B_SPLINE_SURFACE_WITH_KNOTS ( ( 4, 4 ),
 ( 2, 2 ),
 ( 0.000000000000000000, 1.000000000000000000 ),
 ( 0.000000000000000000, 1.000000000000000000 ),
 .UNSPECIFIED. ) 
 GEOMETRIC_REPRESENTATION_ITEM ( )  RATIONAL_B_SPLINE_SURFACE ( (
 ( 1.000000000000000000, 1.000000000000000000),
 ( 0.9960225298536222738, 0.9999952330161893110),
 ( 0.9960225298536222738, 0.9999952330161893110),
 ( 1.000000000000000000, 1.000000000000000000) ) ) 
 REPRESENTATION_ITEM ( '' )  SURFACE ( )  );
#15703 = VERTEX_POINT ( 'NONE', #9459 ) ;
#15704 = ORIENTED_EDGE ( 'NONE', *, *, #5940, .T. ) ;
#15705 = CARTESIAN_POINT ( 'NONE',  ( -1.045287976400362417, 25.66401692419989899, -37.92705037016767733 ) ) ;
#15706 = CARTESIAN_POINT ( 'NONE',  ( 1.833485406944057594, 138.1714136985308699, 44.33323125129973619 ) ) ;
#15707 = ORIENTED_EDGE ( 'NONE', *, *, #17916, .T. ) ;
#15708 = EDGE_CURVE ( 'NONE', #384, #11657, #12872, .T. ) ;
#15709 = EDGE_CURVE ( 'NONE', #3000, #16465, #25586, .T. ) ;
#15710 = CARTESIAN_POINT ( 'NONE',  ( -1.031422197589711764, -44.01264471863837713, 12.69107518035547777 ) ) ;
#15711 = LINE ( 'NONE', #6454, #934 ) ;
#15712 = CONICAL_SURFACE ( 'NONE', #7493, 34.60786435723138510, 0.8559913436420825139 ) ;
#15713 = CARTESIAN_POINT ( 'NONE',  ( -1.046935749539993799, 43.14401153755488849, 15.35946454248350435 ) ) ;
#15714 = EDGE_CURVE ( 'NONE', #10003, #16572, #19745, .T. ) ;
#15715 = DIRECTION ( 'NONE',  ( 1.000000000000000000, -6.938893903907226837E-18, 1.734723475976806709E-18 ) ) ;
#15716 = CARTESIAN_POINT ( 'NONE',  ( 32.73300124599738581, -92.86301839380070078, 72.21147546950520280 ) ) ;
#15717 = CARTESIAN_POINT ( 'NONE',  ( 2.433796855181233454, 138.8296532063088193, 43.58222566461690661 ) ) ;
#15718 = CARTESIAN_POINT ( 'NONE',  ( 2.430230287190589422, -118.5711603495675490, -84.35270093935379521 ) ) ;
#15719 = EDGE_CURVE ( 'NONE', #17840, #5960, #1874, .T. ) ;
#15720 = CARTESIAN_POINT ( 'NONE',  ( -4.162674018437132695, -45.34593312138897403, -18.33413805792422124 ) ) ;
#15721 = FACE_OUTER_BOUND ( 'NONE', #6917, .T. ) ;
#15722 = CARTESIAN_POINT ( 'NONE',  ( 16.75465622695668699, -75.09093759626914277, 120.7871673903169096 ) ) ;
#15723 = FACE_OUTER_BOUND ( 'NONE', #11011, .T. ) ;
#15724 = ORIENTED_EDGE ( 'NONE', *, *, #8205, .F. ) ;
#15725 = B_SPLINE_CURVE_WITH_KNOTS ( 'NONE', 3,
 ( #19101, #23292, #16363, #16810, #23158, #23008 ),
 .UNSPECIFIED., .F., .F.,
 ( 4, 2, 4 ),
 ( 6.505213034913026604E-19, 0.0004335151646191484848, 0.0008670303292382963191 ),
 .UNSPECIFIED. ) ;
#15727 = CARTESIAN_POINT ( 'NONE',  ( -2.911734481061388990, -46.11606034418772282, -12.03743348210763031 ) ) ;
#15726 = FACE_OUTER_BOUND ( 'NONE', #2008, .T. ) ;
#15728 = CARTESIAN_POINT ( 'NONE',  ( 10.93730112725945425, 115.5857507957700818, 97.44200844886312041 ) ) ;
#15729 = CARTESIAN_POINT ( 'NONE',  ( -1.050230346682677007, -37.05264119692671443, 26.91946103437146931 ) ) ;
#15730 = B_SPLINE_CURVE_WITH_KNOTS ( 'NONE', 3,
 ( #21124, #11930, #18693, #20697, #991, #9783, #7634, #7778 ),
 .UNSPECIFIED., .F., .F.,
 ( 4, 2, 2, 4 ),
 ( 6.938893903907228378E-18, 0.0002429592666046787117, 0.0004859185332093504846, 0.0009718370664186806946 ),
 .UNSPECIFIED. ) ;
#15731 = CARTESIAN_POINT ( 'NONE',  ( -20.24399999263414784, 29.60996018918694617, 1.282322917263571282 ) ) ;
#15732 = CARTESIAN_POINT ( 'NONE',  ( -8.786685647604890903, -37.00619870957961410, -38.68584556812286479 ) ) ;
#15733 = ORIENTED_EDGE ( 'NONE', *, *, #25751, .F. ) ;
#15734 = CARTESIAN_POINT ( 'NONE',  ( 1.833838848569439017, -15.34509722932435416, -144.2962335061012595 ) ) ;
#15735 = ORIENTED_EDGE ( 'NONE', *, *, #20637, .F. ) ;
#15736 = DIRECTION ( 'NONE',  ( 1.000000000000000000, -6.938893903907226837E-18, 1.734723475976806709E-18 ) ) ;
#15737 = CARTESIAN_POINT ( 'NONE',  ( 1.833721034905663183, -29.82176961967010342, 142.0123736691685963 ) ) ;
#15738 = ORIENTED_EDGE ( 'NONE', *, *, #18153, .T. ) ;
#15739 = ORIENTED_EDGE ( 'NONE', *, *, #16903, .F. ) ;
#15740 = DIRECTION ( 'NONE',  ( 1.000000000000000000, -6.938893903907226837E-18, 1.734723475976806709E-18 ) ) ;
#15741 = AXIS2_PLACEMENT_3D ( 'NONE', #229, #16290, #15996 ) ;
#15742 = ORIENTED_EDGE ( 'NONE', *, *, #26929, .F. ) ;
#15743 = CARTESIAN_POINT ( 'NONE',  ( 119.2224693531408803, -69.99999999999998579, 19.99999999999996092 ) ) ;
#15745 =( BOUNDED_SURFACE ( )  B_SPLINE_SURFACE ( 3, 1, ( 
 ( #16305, #13857 ),
 ( #20335, #23097 ),
 ( #3076, #5511 ),
 ( #18467, #11849 ) ),
 .UNSPECIFIED., .F., .F., .F. ) 
 B_SPLINE_SURFACE_WITH_KNOTS ( ( 4, 4 ),
 ( 2, 2 ),
 ( 0.000000000000000000, 1.000000000000000000 ),
 ( 0.000000000000000000, 1.000000000000000000 ),
 .UNSPECIFIED. ) 
 GEOMETRIC_REPRESENTATION_ITEM ( )  RATIONAL_B_SPLINE_SURFACE ( (
 ( 1.000000000000000000, 1.000000000000000000),
 ( 0.6386103224230302855, 0.9954351624131538845),
 ( 0.6386103224230302855, 0.9954351624131538845),
 ( 1.000000000000000000, 1.000000000000000000) ) ) 
 REPRESENTATION_ITEM ( '' )  SURFACE ( )  );
#15744 = CIRCLE ( 'NONE', #22678, 151.1787379149930359 ) ;
#15746 = EDGE_LOOP ( 'NONE', ( #26945, #11517, #11648, #3082 ) ) ;
#15747 = B_SPLINE_CURVE_WITH_KNOTS ( 'NONE', 3,
 ( #5607, #5018, #3444, #12223, #7338, #18842, #15961, #9497 ),
 .UNSPECIFIED., .F., .F.,
 ( 4, 2, 2, 4 ),
 ( 3.469446951953614189E-18, 0.0002429592666046780070, 0.0004859185332093525446, 0.0009718370664186804777 ),
 .UNSPECIFIED. ) ;
#15748 = CARTESIAN_POINT ( 'NONE',  ( 2.263178113027049854, -125.2099934853446115, -73.90841366068515583 ) ) ;
#15749 = EDGE_CURVE ( 'NONE', #28186, #10573, #13225, .T. ) ;
#15750 = DIRECTION ( 'NONE',  ( 0.000000000000000000, 0.000000000000000000, 1.000000000000000000 ) ) ;
#15751 = B_SPLINE_CURVE_WITH_KNOTS ( 'NONE', 3,
 ( #25358, #10099, #12247, #1298 ),
 .UNSPECIFIED., .F., .F.,
 ( 4, 4 ),
 ( 3.353811493843786478E-16, 0.01077107486149842322 ),
 .UNSPECIFIED. ) ;
#15752 = B_SPLINE_CURVE_WITH_KNOTS ( 'NONE', 3,
 ( #19271, #16409, #12098, #5468, #23051, #1158 ),
 .UNSPECIFIED., .F., .F.,
 ( 4, 2, 4 ),
 ( 1.604619215278546562E-17, 0.0006311636237756963665, 0.001262327247551376036 ),
 .UNSPECIFIED. ) ;
#15753 = CARTESIAN_POINT ( 'NONE',  ( 2.263178113027048521, 137.8402779654370534, 46.26071604342116927 ) ) ;
#15754 = CARTESIAN_POINT ( 'NONE',  ( -1.619063947482197729, 44.80407745103800465, 11.94059994246113021 ) ) ;
#15755 = EDGE_CURVE ( 'NONE', #27931, #6993, #2201, .T. ) ;
#15756 = CARTESIAN_POINT ( 'NONE',  ( 109.1586059443104944, 0.004378796245583033847, -0.005555961672780077194 ) ) ;
#15757 = CARTESIAN_POINT ( 'NONE',  ( 1.834118845439484335, 107.9567937753793530, 96.96525081350034725 ) ) ;
#15758 = EDGE_CURVE ( 'NONE', #8378, #16670, #20426, .T. ) ;
#15759 = AXIS2_PLACEMENT_3D ( 'NONE', #13487, #11051, #18087 ) ;
#15760 = CARTESIAN_POINT ( 'NONE',  ( 109.1592201516379674, 0.005485778713193748164, -0.005631912476305715558 ) ) ;
#15761 = CARTESIAN_POINT ( 'NONE',  ( -1.058473599757821404, -1.755404039369745650, -45.77379534793243465 ) ) ;
#15762 = AXIS2_PLACEMENT_3D ( 'NONE', #22038, #4475, #15543 ) ;
#15763 = ORIENTED_EDGE ( 'NONE', *, *, #13155, .T. ) ;
#15764 = CARTESIAN_POINT ( 'NONE',  ( 109.1586059443104944, 0.007058870754606102506, 0.0004635842312796298998 ) ) ;
#15765 = AXIS2_PLACEMENT_3D ( 'NONE', #26909, #24782, #22622 ) ;
#15766 = CARTESIAN_POINT ( 'NONE',  ( -20.57838717382308147, 16.28767523336157552, 25.16001208503087838 ) ) ;
#15767 = CARTESIAN_POINT ( 'NONE',  ( 1.833485406944057594, 0.5339064996884692604, 145.1085452359073429 ) ) ;
#15768 = CARTESIAN_POINT ( 'NONE',  ( 2.108393763691195577, -137.7805780486502840, -46.11438684123302068 ) ) ;
#15769 = VERTEX_POINT ( 'NONE', #24436 ) ;
#15770 = CARTESIAN_POINT ( 'NONE',  ( 1.833838850093440387, 44.84138612521095268, 138.0075846865482845 ) ) ;
#15771 = CARTESIAN_POINT ( 'NONE',  ( 1.831572820252009626, -125.1738732943815364, 73.40899645745960811 ) ) ;
#15772 = ORIENTED_EDGE ( 'NONE', *, *, #25538, .F. ) ;
#15773 = CARTESIAN_POINT ( 'NONE',  ( 109.1586900883932856, -0.003656351050324926043, 0.006130969560693652967 ) ) ;
#15774 = ORIENTED_EDGE ( 'NONE', *, *, #12696, .F. ) ;
#15775 = CARTESIAN_POINT ( 'NONE',  ( 25.64681081121880624, -112.3352186517031441, 11.38886654529637887 ) ) ;
#15776 = VECTOR ( 'NONE', #26055, 1000.000000000000114 ) ;
#15777 = CARTESIAN_POINT ( 'NONE',  ( -20.20612092514784663, -28.48192215759672408, -8.058517256680987728 ) ) ;
#15778 = CARTESIAN_POINT ( 'NONE',  ( 1.833838848569414370, -96.96512505224302458, 107.9566558236573570 ) ) ;
#15779 = LINE ( 'NONE', #20138, #23850 ) ;
#15780 = ORIENTED_EDGE ( 'NONE', *, *, #24716, .T. ) ;
#15781 = DIRECTION ( 'NONE',  ( -0.7563875759206388771, -0.6320336713238522419, -0.1685564395263275950 ) ) ;
#15782 = CIRCLE ( 'NONE', #5211, 34.60786435723138510 ) ;
#15783 = ORIENTED_EDGE ( 'NONE', *, *, #10859, .T. ) ;
#15784 = CARTESIAN_POINT ( 'NONE',  ( -1.583189561560256253, -16.68617981233733261, -43.29471907393735819 ) ) ;
#15785 = EDGE_CURVE ( 'NONE', #17500, #2726, #2535, .T. ) ;
#15786 = ORIENTED_EDGE ( 'NONE', *, *, #6948, .T. ) ;
#15788 = B_SPLINE_CURVE_WITH_KNOTS ( 'NONE', 3,
 ( #21189, #25946, #16886, #4051, #17155, #10690, #3921 ),
 .UNSPECIFIED., .F., .F.,
 ( 4, 3, 4 ),
 ( 1.062518129035794345E-17, 0.0007657099931970561164, 0.001530725384384652287 ),
 .UNSPECIFIED. ) ;
#15787 = FACE_OUTER_BOUND ( 'NONE', #26746, .T. ) ;
#15789 = B_SPLINE_CURVE_WITH_KNOTS ( 'NONE', 3,
 ( #7589, #14171, #3252, #12035, #20809, #1095, #15770, #24580, #4839, #5119 ),
 .UNSPECIFIED., .F., .F.,
 ( 4, 3, 3, 4 ),
 ( 2.081668171172168513E-17, 0.0002669559177086255441, 0.0005339118354151051269, 0.001067817517169169670 ),
 .UNSPECIFIED. ) ;
#15790 = CARTESIAN_POINT ( 'NONE',  ( -25.21435515916043713, -23.92354251275918031, 25.00736669481048224 ) ) ;
#15791 = EDGE_CURVE ( 'NONE', #22965, #16076, #4704, .T. ) ;
#15792 = CARTESIAN_POINT ( 'NONE',  ( 1.832998868059890096, 117.0819875546707038, -85.72499093307982321 ) ) ;
#15793 = CARTESIAN_POINT ( 'NONE',  ( 25.81918753295379076, 107.7789657594975097, 34.03777907511953771 ) ) ;
#15794 = DIRECTION ( 'NONE',  ( 0.000000000000000000, 5.223019709707975211E-21, -1.000000000000000000 ) ) ;
#15795 = CARTESIAN_POINT ( 'NONE',  ( -23.79248802219722947, -3.207402715357382306, -33.03370827286730105 ) ) ;
#15796 = EDGE_CURVE ( 'NONE', #20894, #23418, #25941, .T. ) ;
#15797 = VERTEX_POINT ( 'NONE', #20230 ) ;
#15798 =( BOUNDED_SURFACE ( )  B_SPLINE_SURFACE ( 3, 1, ( 
 ( #5188, #11378 ),
 ( #2894, #20446 ),
 ( #26625, #13964 ),
 ( #20153, #15980 ) ),
 .UNSPECIFIED., .F., .F., .F. ) 
 B_SPLINE_SURFACE_WITH_KNOTS ( ( 4, 4 ),
 ( 2, 2 ),
 ( 0.000000000000000000, 1.000000000000000000 ),
 ( 0.000000000000000000, 1.000000000000000000 ),
 .UNSPECIFIED. ) 
 GEOMETRIC_REPRESENTATION_ITEM ( )  RATIONAL_B_SPLINE_SURFACE ( (
 ( 1.000000000000000000, 1.000000000000000000),
 ( 0.9956975270656954757, 0.8568959468854893125),
 ( 0.9956975270656954757, 0.8568959468854893125),
 ( 1.000000000000000000, 1.000000000000000000) ) ) 
 REPRESENTATION_ITEM ( '' )  SURFACE ( )  );
#15799 = VECTOR ( 'NONE', #16691, 1000.000000000000114 ) ;
#15800 = CARTESIAN_POINT ( 'NONE',  ( -55.25719721206881729, -0.01041086141212477223, 0.004044147484878232723 ) ) ;
#15801 = CARTESIAN_POINT ( 'NONE',  ( 2.433796855181233454, -60.50726454507816499, -132.3327394885237425 ) ) ;
#15802 = CARTESIAN_POINT ( 'NONE',  ( -7.711401346138398338, 21.83927363365101115, 47.70038152767067885 ) ) ;
#15803 = ORIENTED_EDGE ( 'NONE', *, *, #3377, .F. ) ;
#15804 = VERTEX_POINT ( 'NONE', #527 ) ;
#15805 = ORIENTED_EDGE ( 'NONE', *, *, #28350, .F. ) ;
#15806 = CARTESIAN_POINT ( 'NONE',  ( 14.74894986621300141, -20.00000000000000000, 1.693217769544952477E-16 ) ) ;
#15807 = B_SPLINE_CURVE_WITH_KNOTS ( 'NONE', 3,
 ( #13685, #24510, #5053, #11530 ),
 .UNSPECIFIED., .F., .F.,
 ( 4, 4 ),
 ( 1.909141801897607538E-16, 0.001982023823822941146 ),
 .UNSPECIFIED. ) ;
#15808 = CARTESIAN_POINT ( 'NONE',  ( 2.063896406836605024, -133.2511741302124335, 57.85593781835370208 ) ) ;
#15809 = CARTESIAN_POINT ( 'NONE',  ( 26.11404676487256893, -12.95861723607530003, 112.4785329405481349 ) ) ;
#15810 = CARTESIAN_POINT ( 'NONE',  ( 1.833721034905651637, 144.3516387774751593, 14.81406766075982695 ) ) ;
#15811 = CARTESIAN_POINT ( 'NONE',  ( 25.98107933586732088, -103.7920584735895773, 45.01656174308536862 ) ) ;
#15812 = CARTESIAN_POINT ( 'NONE',  ( 2.063896406836605024, 71.46753739786015558, 126.4736179849650313 ) ) ;
#15813 = ORIENTED_EDGE ( 'NONE', *, *, #12736, .F. ) ;
#15814 = CARTESIAN_POINT ( 'NONE',  ( 8.186469777910893697, -146.7694294853781685, -27.65107827750229674 ) ) ;
#15815 = DIRECTION ( 'NONE',  ( 0.000000000000000000, 5.223019709708233256E-21, -1.000000000000000000 ) ) ;
#15816 = CARTESIAN_POINT ( 'NONE',  ( 1.833485406944043827, -145.1085452359073145, -0.5339064996899981486 ) ) ;
#15817 = FACE_OUTER_BOUND ( 'NONE', #11292, .T. ) ;
#15818 = CARTESIAN_POINT ( 'NONE',  ( 13.36082413113061307, 94.94363694444213309, -119.8836995922717108 ) ) ;
#15819 = ORIENTED_EDGE ( 'NONE', *, *, #10633, .F. ) ;
#15821 = CARTESIAN_POINT ( 'NONE',  ( 1.893872463202029399, 45.75900850850183588, -137.7483215415844597 ) ) ;
#15820 = B_SPLINE_CURVE_WITH_KNOTS ( 'NONE', 3,
 ( #5951, #16745, #5504, #14426 ),
 .UNSPECIFIED., .F., .F.,
 ( 4, 4 ),
 ( 1.977889076651310254E-16, 0.001982023823822932906 ),
 .UNSPECIFIED. ) ;
#15822 = CARTESIAN_POINT ( 'NONE',  ( 30.58324630866350446, 8.712468656082224427, -120.6294372749320587 ) ) ;
#15823 = CARTESIAN_POINT ( 'NONE',  ( -1.056502255334265339, -13.66916755949880802, -43.72121397317219049 ) ) ;
#15824 = ORIENTED_EDGE ( 'NONE', *, *, #12188, .F. ) ;
#15825 = VERTEX_POINT ( 'NONE', #24811 ) ;
#15826 = EDGE_CURVE ( 'NONE', #25218, #8356, #849, .T. ) ;
#15827 = ORIENTED_EDGE ( 'NONE', *, *, #23880, .T. ) ;
#15828 = EDGE_CURVE ( 'NONE', #27008, #12942, #14246, .T. ) ;
#15829 = CARTESIAN_POINT ( 'NONE',  ( 16.05277956358211711, -39.81690014528761168, 137.6634701901228084 ) ) ;
#15830 = CARTESIAN_POINT ( 'NONE',  ( 30.59138290137884653, -113.0806461017755140, 26.79783179610965504 ) ) ;
#15831 = EDGE_CURVE ( 'NONE', #15929, #24730, #16296, .T. ) ;
#15832 = CARTESIAN_POINT ( 'NONE',  ( 26.04756280548354397, 57.54844730865669788, 97.45505646068853878 ) ) ;
#15833 = CARTESIAN_POINT ( 'NONE',  ( 2.433796855181233454, 57.85512797798071460, -133.5135467655512400 ) ) ;
#15834 = DIRECTION ( 'NONE',  ( -0.5946245182733607137, 0.5994612328333183138, 0.5357871896547470314 ) ) ;
#15835 = VERTEX_POINT ( 'NONE', #14121 ) ;
#15836 = CARTESIAN_POINT ( 'NONE',  ( -1.031422197589716205, -37.93675465142491277, -25.67058493451430934 ) ) ;
#15837 = CARTESIAN_POINT ( 'NONE',  ( 1.831572820252009626, -16.14965423926112464, -144.2101521542832074 ) ) ;
#15838 = CARTESIAN_POINT ( 'NONE',  ( -1.048994561756789734, -0.7655149579820232919, 45.79144455904142319 ) ) ;
#15839 = ORIENTED_EDGE ( 'NONE', *, *, #21609, .T. ) ;
#15840 =( BOUNDED_SURFACE ( )  B_SPLINE_SURFACE ( 3, 1, ( 
 ( #541, #2846 ),
 ( #9046, #18096 ),
 ( #26874, #7463 ),
 ( #22433, #17802 ) ),
 .UNSPECIFIED., .F., .F., .F. ) 
 B_SPLINE_SURFACE_WITH_KNOTS ( ( 4, 4 ),
 ( 2, 2 ),
 ( 0.000000000000000000, 1.000000000000000000 ),
 ( 0.000000000000000000, 1.000000000000000000 ),
 .UNSPECIFIED. ) 
 GEOMETRIC_REPRESENTATION_ITEM ( )  RATIONAL_B_SPLINE_SURFACE ( (
 ( 1.000000000000000000, 1.000000000000000000),
 ( 0.9593753223639863714, 0.9995975284513187731),
 ( 0.9593753223639863714, 0.9995975284513187731),
 ( 1.000000000000000000, 1.000000000000000000) ) ) 
 REPRESENTATION_ITEM ( '' )  SURFACE ( )  );
#15841 = CARTESIAN_POINT ( 'NONE',  ( -23.79223135445719706, 33.03345552685145492, 3.207301057648455966 ) ) ;
#15842 = ORIENTED_EDGE ( 'NONE', *, *, #3090, .F. ) ;
#15843 = CARTESIAN_POINT ( 'NONE',  ( 1.833485406944043827, 30.69200235379130959, -141.8265699653863976 ) ) ;
#15844 = CARTESIAN_POINT ( 'NONE',  ( 25.64681081121879203, -45.54494737132156246, -103.3177883989783936 ) ) ;
#15845 = CARTESIAN_POINT ( 'NONE',  ( -10.86508079875782151, 46.07061504567116828, 22.20099862734772245 ) ) ;
#15846 = CARTESIAN_POINT ( 'NONE',  ( -1.049819825607590351, 14.63675055554442395, 43.39756533277866879 ) ) ;
#15847 = CARTESIAN_POINT ( 'NONE',  ( 2.433796855181205476, 60.50726454508082952, -132.3327394885224919 ) ) ;
#15848 = CARTESIAN_POINT ( 'NONE',  ( 32.73300124599740002, -89.94078864464006529, -75.82012867748569818 ) ) ;
#15849 = CARTESIAN_POINT ( 'NONE',  ( 2.433796855181205476, 16.65276281464756636, -144.5536872373190533 ) ) ;
#15850 = B_SPLINE_CURVE_WITH_KNOTS ( 'NONE', 3,
 ( #24381, #4799, #13275, #470, #323, #8979, #2183, #15875 ),
 .UNSPECIFIED., .F., .F.,
 ( 4, 2, 2, 4 ),
 ( 1.551583845779545699E-17, 0.0002429592666046909361, 0.0004859185332093663681, 0.0009718370664186812367 ),
 .UNSPECIFIED. ) ;
#15851 = B_SPLINE_CURVE_WITH_KNOTS ( 'NONE', 3,
 ( #18937, #17322, #27854, #27713, #5845, #8281, #12583, #8151 ),
 .UNSPECIFIED., .F., .F.,
 ( 4, 2, 2, 4 ),
 ( 0.000000000000000000, 0.0002429588503611205359, 0.0004859177007222410718, 0.0009718354014444899498 ),
 .UNSPECIFIED. ) ;
#15852 = CARTESIAN_POINT ( 'NONE',  ( 1.831572820252008738, 107.1759352627506416, 97.82994539998418304 ) ) ;
#15853 = CARTESIAN_POINT ( 'NONE',  ( 1.833485406944057594, 58.53321471327059555, -132.7804117027882285 ) ) ;
#15854 = CARTESIAN_POINT ( 'NONE',  ( 25.64708010899965629, -107.3680906278374323, 34.94352788466252235 ) ) ;
#15855 = B_SPLINE_CURVE_WITH_KNOTS ( 'NONE', 3,
 ( #13648, #2004, #11213, #22007 ),
 .UNSPECIFIED., .F., .F.,
 ( 4, 4 ),
 ( 0.000000000000000000, 0.008383560773332738095 ),
 .UNSPECIFIED. ) ;
#15856 = EDGE_CURVE ( 'NONE', #1309, #2120, #20469, .T. ) ;
#15857 = ORIENTED_EDGE ( 'NONE', *, *, #5204, .F. ) ;
#15858 = CARTESIAN_POINT ( 'NONE',  ( -1.323439229708132769, 44.47813215539063947, 12.01475235539399300 ) ) ;
#15859 = CARTESIAN_POINT ( 'NONE',  ( 2.433796855181205476, 71.49415740225076377, 126.7346379669258312 ) ) ;
#15860 = ORIENTED_EDGE ( 'NONE', *, *, #22939, .T. ) ;
#15861 = ORIENTED_EDGE ( 'NONE', *, *, #2865, .F. ) ;
#15862 = EDGE_CURVE ( 'NONE', #10945, #6911, #7752, .T. ) ;
#15863 = ORIENTED_EDGE ( 'NONE', *, *, #7366, .F. ) ;
#15864 = CARTESIAN_POINT ( 'NONE',  ( -1.463510566862821882, -2.430838777909866355, 46.14841196428346848 ) ) ;
#15865 = EDGE_CURVE ( 'NONE', #27652, #8378, #10150, .T. ) ;
#15866 = CARTESIAN_POINT ( 'NONE',  ( -4.473127245936434626, -45.82513704981530367, 18.25038884639918280 ) ) ;
#15867 = CARTESIAN_POINT ( 'NONE',  ( -55.24390624410018802, -0.007245494385991098352, -0.007503127514281985981 ) ) ;
#15868 = CARTESIAN_POINT ( 'NONE',  ( -28.13707043255157103, -22.88591869784691823, -0.7675454997506192534 ) ) ;
#15869 = CARTESIAN_POINT ( 'NONE',  ( -55.24390624410018802, -0.01032895241566633357, -0.001451500391952961289 ) ) ;
#15870 = CARTESIAN_POINT ( 'NONE',  ( 2.430230287190581429, 118.5711603495692827, -84.35270093935136515 ) ) ;
#15871 = CARTESIAN_POINT ( 'NONE',  ( 13.84597867724970577, -49.85807424839853752, 137.9700459519988556 ) ) ;
#15872 = CARTESIAN_POINT ( 'NONE',  ( 32.73300124599735739, 3.836798148478847370, 117.5726003567930178 ) ) ;
#15873 = CARTESIAN_POINT ( 'NONE',  ( 109.1778270068192853, -0.006682187084648866932, 0.006489198140359601387 ) ) ;
#15874 = LINE ( 'NONE', #24682, #4631 ) ;
#15875 = CARTESIAN_POINT ( 'NONE',  ( 25.64681081121879203, -66.03065707438999254, 91.59071981940550700 ) ) ;
#15876 = CARTESIAN_POINT ( 'NONE',  ( -9.156249394959713683, -8.027840202794317648, -53.90509764945126392 ) ) ;
#15877 = CARTESIAN_POINT ( 'NONE',  ( -20.57838717382308147, -23.26537097894118133, -18.89542499756491978 ) ) ;
#15878 = VERTEX_POINT ( 'NONE', #11700 ) ;
#15879 = CARTESIAN_POINT ( 'NONE',  ( 25.64708010899965984, -66.41183455464074825, -91.31497827399797984 ) ) ;
#15880 = CARTESIAN_POINT ( 'NONE',  ( 2.430230287190592531, -126.7388733285340123, -71.49654683843642999 ) ) ;
#15881 = CARTESIAN_POINT ( 'NONE',  ( 1.834118845439484335, -125.7578880615040049, -72.40084790867462061 ) ) ;
#15882 = FACE_OUTER_BOUND ( 'NONE', #10123, .T. ) ;
#15883 = CARTESIAN_POINT ( 'NONE',  ( 21.16825799904902539, -131.4851843440079335, 32.46271504707898714 ) ) ;
#15884 =( BOUNDED_SURFACE ( )  B_SPLINE_SURFACE ( 3, 1, ( 
 ( #27564, #1096 ),
 ( #9885, #25434 ),
 ( #5710, #21236 ),
 ( #12308, #1517 ) ),
 .UNSPECIFIED., .F., .F., .F. ) 
 B_SPLINE_SURFACE_WITH_KNOTS ( ( 4, 4 ),
 ( 2, 2 ),
 ( 0.000000000000000000, 1.000000000000000000 ),
 ( 0.000000000000000000, 1.000000000000000000 ),
 .UNSPECIFIED. ) 
 GEOMETRIC_REPRESENTATION_ITEM ( )  RATIONAL_B_SPLINE_SURFACE ( (
 ( 1.000000000000000000, 1.000000000000000000),
 ( 0.7789835883360578528, 0.9689951854195403280),
 ( 0.7789835883360578528, 0.9689951854195403280),
 ( 1.000000000000000000, 1.000000000000000000) ) ) 
 REPRESENTATION_ITEM ( '' )  SURFACE ( )  );
#15885 = CARTESIAN_POINT ( 'NONE',  ( -20.20997486282892552, -0.3303743256173646836, 29.60348406988233450 ) ) ;
#15886 = EDGE_CURVE ( 'NONE', #27831, #15797, #11149, .T. ) ;
#15887 = ORIENTED_EDGE ( 'NONE', *, *, #17510, .T. ) ;
#15888 = CARTESIAN_POINT ( 'NONE',  ( -1.619063947482201282, -16.67502769180592992, -43.26576862488428077 ) ) ;
#15889 = CARTESIAN_POINT ( 'NONE',  ( -1.239374126674604337, 35.79060836339854745, 28.97829083655398819 ) ) ;
#15890 = ORIENTED_EDGE ( 'NONE', *, *, #7996, .T. ) ;
#15891 = EDGE_CURVE ( 'NONE', #14327, #15152, #21452, .T. ) ;
#15892 = B_SPLINE_CURVE_WITH_KNOTS ( 'NONE', 3,
 ( #200, #17749, #26391, #6692, #13426, #17878, #6266, #25103 ),
 .UNSPECIFIED., .F., .F.,
 ( 4, 2, 2, 4 ),
 ( 0.000000000000000000, 0.0002429588503611167412, 0.0004859177007222334824, 0.0009718354014444809509 ),
 .UNSPECIFIED. ) ;
#15893 = CARTESIAN_POINT ( 'NONE',  ( 30.59138290137878613, 26.79783179610999255, 113.0806461017753861 ) ) ;
#15894 = EDGE_LOOP ( 'NONE', ( #24120, #627, #2002, #9851 ) ) ;
#15895 = CARTESIAN_POINT ( 'NONE',  ( 28.37599760073042532, -98.45181492308078930, -58.91309773266252847 ) ) ;
#15896 = ORIENTED_EDGE ( 'NONE', *, *, #28129, .T. ) ;
#15897 = EDGE_CURVE ( 'NONE', #18596, #11834, #13847, .T. ) ;
#15898 = B_SPLINE_CURVE_WITH_KNOTS ( 'NONE', 3,
 ( #487, #638, #9426, #21025, #25521, #7817, #26825, #9281, #7676, #341 ),
 .UNSPECIFIED., .F., .F.,
 ( 4, 2, 2, 2, 4 ),
 ( 5.898697549827394244E-18, 0.0003346267210630972291, 0.0006692534421261884950, 0.001003880163189279761, 0.001338506884252371135 ),
 .UNSPECIFIED. ) ;
#15899 = ORIENTED_EDGE ( 'NONE', *, *, #8005, .T. ) ;
#15900 = FACE_OUTER_BOUND ( 'NONE', #25523, .T. ) ;
#15901 = EDGE_CURVE ( 'NONE', #17999, #14115, #17658, .T. ) ;
#15902 = CARTESIAN_POINT ( 'NONE',  ( 10.93730112725990367, -149.7554878793147566, -20.69552240458495973 ) ) ;
#15903 = CARTESIAN_POINT ( 'NONE',  ( -1.019300379054419725, 25.26451264419644716, -38.21680004809172004 ) ) ;
#15904 = CARTESIAN_POINT ( 'NONE',  ( 109.1586059443104944, -0.006856640434643085195, 0.001740416220259381535 ) ) ;
#15905 = DIRECTION ( 'NONE',  ( -0.5946245182733607137, 0.08697490616138922603, 0.7992853357633875611 ) ) ;
#15906 = CARTESIAN_POINT ( 'NONE',  ( 25.98107933586738483, -110.4296102877912631, -24.58827779736892438 ) ) ;
#15907 = CARTESIAN_POINT ( 'NONE',  ( -20.20612091757422846, -29.57813639663779526, -1.137293889216260512 ) ) ;
#15908 = CARTESIAN_POINT ( 'NONE',  ( 13.84597867724971465, -101.6650905919619419, 105.7628030201716456 ) ) ;
#15909 = ORIENTED_EDGE ( 'NONE', *, *, #12725, .T. ) ;
#15910 = CARTESIAN_POINT ( 'NONE',  ( -55.24340739397742794, -0.006539691034608149933, -0.007744344507854676943 ) ) ;
#15912 = CARTESIAN_POINT ( 'NONE',  ( -8.786685647604898008, 48.22796981442765940, -23.24040270374399952 ) ) ;
#15911 = CARTESIAN_POINT ( 'NONE',  ( -22.23342874802668589, 11.82490389046315116, -29.33662284748865900 ) ) ;
#15913 = CARTESIAN_POINT ( 'NONE',  ( 109.1587776205901577, 0.004375189885414170615, -0.005880209827417003793 ) ) ;
#15914 = CARTESIAN_POINT ( 'NONE',  ( -20.90916690077964191, -39.20864005633521998, 5.322316104228396405 ) ) ;
#15915 = ORIENTED_EDGE ( 'NONE', *, *, #9594, .T. ) ;
#15916 = DIRECTION ( 'NONE',  ( -1.000000000000000000, 0.000000000000000000, 0.000000000000000000 ) ) ;
#15917 = CARTESIAN_POINT ( 'NONE',  ( -24.53239521893651442, 16.68574937151015192, 29.54733954334095358 ) ) ;
#15918 = CARTESIAN_POINT ( 'NONE',  ( 6.224689322667647851, -84.93872395423059629, 121.2721959030534862 ) ) ;
#15919 = ORIENTED_EDGE ( 'NONE', *, *, #22680, .T. ) ;
#15920 = CARTESIAN_POINT ( 'NONE',  ( 109.1589550718175161, 0.003591809816099524391, -0.006669585340474280290 ) ) ;
#15921 = ADVANCED_FACE ( 'NONE', ( #1323 ), #24218, .F. ) ;
#15922 = ORIENTED_EDGE ( 'NONE', *, *, #2687, .F. ) ;
#15923 = CARTESIAN_POINT ( 'NONE',  ( -8.786685647604890903, 47.14957014837354876, -25.35688121747519119 ) ) ;
#15924 = EDGE_CURVE ( 'NONE', #13159, #20294, #20058, .T. ) ;
#15925 = VERTEX_POINT ( 'NONE', #22654 ) ;
#15926 = ORIENTED_EDGE ( 'NONE', *, *, #4648, .T. ) ;
#15927 = CARTESIAN_POINT ( 'NONE',  ( -20.57838717382308147, -16.28767523336102130, 25.16001208503123365 ) ) ;
#15928 = B_SPLINE_CURVE_WITH_KNOTS ( 'NONE', 3,
 ( #2538, #17927, #14014, #16467, #17656, #5383 ),
 .UNSPECIFIED., .F., .F.,
 ( 4, 2, 4 ),
 ( 4.336808689942017736E-19, 0.0006311636237756775014, 0.001262327247551354569 ),
 .UNSPECIFIED. ) ;
#15929 = VERTEX_POINT ( 'NONE', #19548 ) ;
#15930 = B_SPLINE_CURVE_WITH_KNOTS ( 'NONE', 3,
 ( #5842, #15014, #3662, #1359, #12438, #27980 ),
 .UNSPECIFIED., .F., .F.,
 ( 4, 2, 4 ),
 ( 2.602085213965210642E-18, 0.0006311636237756776098, 0.001262327247551352618 ),
 .UNSPECIFIED. ) ;
#15931 = CARTESIAN_POINT ( 'NONE',  ( -20.20612091757424977, 28.48192249925588371, -8.058516044219283359 ) ) ;
#15932 = CARTESIAN_POINT ( 'NONE',  ( -24.53239521893653219, 24.99972072650176713, 22.94500969220215580 ) ) ;
#15933 = CARTESIAN_POINT ( 'NONE',  ( -55.24390624410018802, 0.01032895241567037548, -0.001451500391950801341 ) ) ;
#15934 = CARTESIAN_POINT ( 'NONE',  ( 119.2224693531408803, 69.99999999999998579, -40.00000000000000711 ) ) ;
#15935 = VERTEX_POINT ( 'NONE', #26169 ) ;
#15936 = CARTESIAN_POINT ( 'NONE',  ( 25.64699802086723679, 0.2377811728597830354, 112.9109702078780089 ) ) ;
#15937 = CARTESIAN_POINT ( 'NONE',  ( 8.186469829613953308, 149.3111477833936078, 3.468244397267471246 ) ) ;
#15938 = LINE ( 'NONE', #4997, #5856 ) ;
#15939 = ORIENTED_EDGE ( 'NONE', *, *, #11680, .T. ) ;
#15940 = B_SPLINE_CURVE_WITH_KNOTS ( 'NONE', 3,
 ( #1859, #10519, #25513, #1449 ),
 .UNSPECIFIED., .F., .F.,
 ( 4, 4 ),
 ( 0.000000000000000000, 0.01077107196513845538 ),
 .UNSPECIFIED. ) ;
#15941 = EDGE_LOOP ( 'NONE', ( #970, #22970, #5787, #10793 ) ) ;
#15942 = ORIENTED_EDGE ( 'NONE', *, *, #3036, .T. ) ;
#15943 = CARTESIAN_POINT ( 'NONE',  ( -1.048172774974294175, 37.64158596421250991, 26.08722459372745206 ) ) ;
#15944 = CARTESIAN_POINT ( 'NONE',  ( 109.1589550718175161, 0.004900004919101233827, -0.005777059646713199673 ) ) ;
#15945 = FACE_OUTER_BOUND ( 'NONE', #11857, .T. ) ;
#15946 = CARTESIAN_POINT ( 'NONE',  ( 13.84597867724975728, 49.85807424839934043, -137.9700459519982871 ) ) ;
#15947 = LINE ( 'NONE', #9775, #14833 ) ;
#15948 = CARTESIAN_POINT ( 'NONE',  ( -55.24198130335446422, 0.004163123460802997666, 0.008310594958152995454 ) ) ;
#15949 = CARTESIAN_POINT ( 'NONE',  ( -28.13707043255157103, 0.7675454997506996335, -22.88591869784691113 ) ) ;
#15950 = ORIENTED_EDGE ( 'NONE', *, *, #459, .T. ) ;
#15951 = FACE_OUTER_BOUND ( 'NONE', #11974, .T. ) ;
#15952 = CARTESIAN_POINT ( 'NONE',  ( 8.186469829614265947, -102.4860667297603243, 108.6390983847746980 ) ) ;
#15953 = CARTESIAN_POINT ( 'NONE',  ( 1.833838850855461722, -145.1097630809418320, -0.08898185259725979734 ) ) ;
#15954 = FACE_OUTER_BOUND ( 'NONE', #9169, .T. ) ;
#15955 = CARTESIAN_POINT ( 'NONE',  ( -20.24419206586952313, -27.76448493191437095, 10.37009329716794248 ) ) ;
#15956 = DIRECTION ( 'NONE',  ( 0.5914120900931444380, 0.7398809652418028016, -0.3206367055789413611 ) ) ;
#15957 = EDGE_CURVE ( 'NONE', #6789, #23146, #25793, .T. ) ;
#15958 = ORIENTED_EDGE ( 'NONE', *, *, #20495, .T. ) ;
#15959 = CARTESIAN_POINT ( 'NONE',  ( 32.73300124599740002, 66.00340565729470654, -97.37344512919790418 ) ) ;
#15960 = EDGE_LOOP ( 'NONE', ( #5137, #5778 ) ) ;
#15961 = CARTESIAN_POINT ( 'NONE',  ( 25.64660436782563480, 110.3216080362391409, -24.04259444204547336 ) ) ;
#15962 = EDGE_CURVE ( 'NONE', #335, #18831, #20777, .T. ) ;
#15963 = CARTESIAN_POINT ( 'NONE',  ( 2.430230287190581429, -86.70145658344736717, 116.8646894862409198 ) ) ;
#15964 = ORIENTED_EDGE ( 'NONE', *, *, #4745, .T. ) ;
#15965 = EDGE_CURVE ( 'NONE', #27450, #11640, #3960, .T. ) ;
#15966 = VERTEX_POINT ( 'NONE', #24166 ) ;
#15967 = ORIENTED_EDGE ( 'NONE', *, *, #28101, .F. ) ;
#15968 = CARTESIAN_POINT ( 'NONE',  ( 2.430230287190572103, 107.1617224697464366, 98.44218333480806393 ) ) ;
#15969 = CARTESIAN_POINT ( 'NONE',  ( -1.019300379054419725, -44.15350047934408195, -12.21833869579447729 ) ) ;
#15970 = DIRECTION ( 'NONE',  ( -1.000000000000000000, -0.000000000000000000, -0.000000000000000000 ) ) ;
#15971 = CARTESIAN_POINT ( 'NONE',  ( 24.01988960052056754, 17.94039809062794788, -129.8107982898199566 ) ) ;
#15972 = CARTESIAN_POINT ( 'NONE',  ( 16.05277956358199276, 121.7045645913028693, -75.66118899150391996 ) ) ;
#15973 = CARTESIAN_POINT ( 'NONE',  ( 25.64708010899967405, 34.94352788466287763, 107.3680906278372760 ) ) ;
#15974 = EDGE_CURVE ( 'NONE', #23403, #4018, #20721, .T. ) ;
#15975 = CARTESIAN_POINT ( 'NONE',  ( -20.20700224038492010, -0.9908225410476447781, 29.58392382092673500 ) ) ;
#15976 = ORIENTED_EDGE ( 'NONE', *, *, #8545, .F. ) ;
#15977 = VERTEX_POINT ( 'NONE', #21569 ) ;
#15978 = CARTESIAN_POINT ( 'NONE',  ( -1.045287976400362417, -15.59869763335038506, 43.05558670614261985 ) ) ;
#15979 = CARTESIAN_POINT ( 'NONE',  ( -1.045287976400379737, -37.92705037016725100, 25.66401692420055269 ) ) ;
#15980 = CARTESIAN_POINT ( 'NONE',  ( 1.832998868059858122, -141.8272129421610543, 30.69214149073968656 ) ) ;
#15981 = DIRECTION ( 'NONE',  ( 0.8320502949607718746, 0.000000000000000000, -0.5547001952908368061 ) ) ;
#15982 = DIRECTION ( 'NONE',  ( 0.5946245182733607137, -0.2456431038754811613, -0.7655593692109013970 ) ) ;
#15983 = CARTESIAN_POINT ( 'NONE',  ( -25.21435515916025594, 1.749597353048488237E-16, -4.373993382621220594E-17 ) ) ;
#15984 = EDGE_CURVE ( 'NONE', #19211, #22079, #16294, .T. ) ;
#15985 = EDGE_LOOP ( 'NONE', ( #807, #22370, #21269, #18092 ) ) ;
#15986 = CARTESIAN_POINT ( 'NONE',  ( -1.539763995773683503, 44.72359274866481371, -11.93465967526309868 ) ) ;
#15987 = DIRECTION ( 'NONE',  ( 0.000000000000000000, 0.000000000000000000, 1.000000000000000000 ) ) ;
#15988 = EDGE_CURVE ( 'NONE', #18758, #14894, #9790, .T. ) ;
#15989 = B_SPLINE_CURVE_WITH_KNOTS ( 'NONE', 3,
 ( #14054, #4856, #16221, #11621 ),
 .UNSPECIFIED., .F., .F.,
 ( 4, 4 ),
 ( 2.596296363159515209E-17, 0.008383748772659474491 ),
 .UNSPECIFIED. ) ;
#15990 = DIRECTION ( 'NONE',  ( -1.000000000000000000, -0.000000000000000000, -0.000000000000000000 ) ) ;
#15991 = DIRECTION ( 'NONE',  ( 0.000000000000000000, 5.223019709707975211E-21, -1.000000000000000000 ) ) ;
#15992 = CARTESIAN_POINT ( 'NONE',  ( -1.058473599757832062, 44.07591602137171094, 12.47539220917817815 ) ) ;
#15993 = ORIENTED_EDGE ( 'NONE', *, *, #20174, .T. ) ;
#15994 = ORIENTED_EDGE ( 'NONE', *, *, #14329, .T. ) ;
#15995 = ORIENTED_EDGE ( 'NONE', *, *, #8466, .T. ) ;
#15996 = DIRECTION ( 'NONE',  ( 0.000000000000000000, 0.000000000000000000, 1.000000000000000000 ) ) ;
#15997 = CARTESIAN_POINT ( 'NONE',  ( -1.046936909428696438, 36.28616897897453697, -27.93981068760634656 ) ) ;
#15998 = B_SPLINE_CURVE_WITH_KNOTS ( 'NONE', 3,
 ( #22337, #10965, #21902, #299 ),
 .UNSPECIFIED., .F., .F.,
 ( 4, 4 ),
 ( 0.000000000000000000, 0.01077107196513877110 ),
 .UNSPECIFIED. ) ;
#15999 = CARTESIAN_POINT ( 'NONE',  ( -1.583189561560256253, 2.490696082060512406, 46.33203782964458384 ) ) ;
#16000 = UNCERTAINTY_MEASURE_WITH_UNIT (LENGTH_MEASURE( 1.000000000000000082E-05 ), #25277, 'distance_accuracy_value', 'NONE');
#16001 = CARTESIAN_POINT ( 'NONE',  ( -2.904412668506652473, -17.42365698954667863, 44.35433137608958276 ) ) ;
#16002 = CARTESIAN_POINT ( 'NONE',  ( 109.1586059443104944, 0.004935564877224682574, 0.005067816690886773300 ) ) ;
#16003 = CARTESIAN_POINT ( 'NONE',  ( 28.37603512858443011, -105.5302493666424084, -45.02094145483482635 ) ) ;
#16004 = CARTESIAN_POINT ( 'NONE',  ( -1.539763995773680172, -16.63252574783015092, 43.19716353142347742 ) ) ;
#16005 = CARTESIAN_POINT ( 'NONE',  ( -20.21097721650787804, 23.76068422213757714, -17.67178726257366606 ) ) ;
#16006 = VECTOR ( 'NONE', #1224, 1000.000000000000114 ) ;
#16007 = CARTESIAN_POINT ( 'NONE',  ( 2.263178113027064953, -31.59906256848382000, 141.9207360579561055 ) ) ;
#16008 = ADVANCED_FACE ( 'NONE', ( #1986, #28317, #15489, #23762 ), #19410, .F. ) ;
#16009 = CARTESIAN_POINT ( 'NONE',  ( -5.986830583229481917, -46.64941882410784757, 19.95149887249902321 ) ) ;
#16010 = CARTESIAN_POINT ( 'NONE',  ( 109.1586059443104944, 0.001921075557418361855, -0.006808232911146196685 ) ) ;
#16011 = LINE ( 'NONE', #5072, #4071 ) ;
#16012 = EDGE_CURVE ( 'NONE', #13097, #17077, #28180, .T. ) ;
#16013 = CARTESIAN_POINT ( 'NONE',  ( -25.21435515916043713, -30.48034229288650820, -16.39063784838731053 ) ) ;
#16014 = EDGE_CURVE ( 'NONE', #20645, #18370, #17380, .T. ) ;
#16015 = LINE ( 'NONE', #17876, #27622 ) ;
#16016 = FACE_OUTER_BOUND ( 'NONE', #12259, .T. ) ;
#16017 = B_SPLINE_CURVE_WITH_KNOTS ( 'NONE', 3,
 ( #22397, #5107, #20212, #17902 ),
 .UNSPECIFIED., .F., .F.,
 ( 4, 4 ),
 ( 3.113236650999850422E-16, 0.008383748772659758985 ),
 .UNSPECIFIED. ) ;
#16018 = CARTESIAN_POINT ( 'NONE',  ( 28.37599760073042177, 65.97809271467136227, 93.86375353586188908 ) ) ;
#16019 = CARTESIAN_POINT ( 'NONE',  ( 109.1721716018069515, 0.01281875973823902275, -0.01127028715939376591 ) ) ;
#16020 = ORIENTED_EDGE ( 'NONE', *, *, #15758, .T. ) ;
#16021 = CARTESIAN_POINT ( 'NONE',  ( -55.24271866751342941, 0.001545935011627245191, 0.009369360294294363373 ) ) ;
#16022 = ORIENTED_EDGE ( 'NONE', *, *, #21580, .T. ) ;
#16023 = DIRECTION ( 'NONE',  ( 1.000000000000000000, -6.938893903907226837E-18, 1.734723475976806709E-18 ) ) ;
#16024 = CARTESIAN_POINT ( 'NONE',  ( 1.833838850855487479, -30.25705358194946726, 141.9202662332486682 ) ) ;
#16025 = ORIENTED_EDGE ( 'NONE', *, *, #12570, .F. ) ;
#16026 = ORIENTED_EDGE ( 'NONE', *, *, #26690, .T. ) ;
#16027 = VERTEX_POINT ( 'NONE', #19823 ) ;
#16028 = ORIENTED_EDGE ( 'NONE', *, *, #4559, .F. ) ;
#16029 = CARTESIAN_POINT ( 'NONE',  ( -1.583189561560256253, 11.94859433442902130, -44.83405390829675952 ) ) ;
#16030 = B_SPLINE_CURVE_WITH_KNOTS ( 'NONE', 3,
 ( #2027, #10415, #6364, #28225, #8527, #10830, #19179 ),
 .UNSPECIFIED., .F., .F.,
 ( 4, 3, 4 ),
 ( 0.000000000000000000, 0.006568092053401815289, 0.02506242213020845253 ),
 .UNSPECIFIED. ) ;
#16031 = DIRECTION ( 'NONE',  ( -1.000000000000000000, -0.000000000000000000, -0.000000000000000000 ) ) ;
#16032 = B_SPLINE_CURVE_WITH_KNOTS ( 'NONE', 3,
 ( #5782, #12516, #7661, #27348, #5629, #8089 ),
 .UNSPECIFIED., .F., .F.,
 ( 4, 2, 4 ),
 ( 1.965608005753612659E-17, 0.0006311571484586163058, 0.001262314296917213096 ),
 .UNSPECIFIED. ) ;
#16033 = CARTESIAN_POINT ( 'NONE',  ( 1.834118845439484335, -132.4921483272732132, 59.18411796427007232 ) ) ;
#16034 = CARTESIAN_POINT ( 'NONE',  ( -8.786685647604896232, 52.67761315067299677, 9.545808661480061019 ) ) ;
#16035 = EDGE_CURVE ( 'NONE', #23403, #11830, #8408, .T. ) ;
#16036 = CARTESIAN_POINT ( 'NONE',  ( 13.36082413113063083, 67.94366799842813975, 137.0038452127802771 ) ) ;
#16037 = CARTESIAN_POINT ( 'NONE',  ( -4.178947244162631414, 11.88256963646738740, -47.46809051147726422 ) ) ;
#16038 = FACE_OUTER_BOUND ( 'NONE', #20967, .T. ) ;
#16039 = ADVANCED_FACE ( 'NONE', ( #251 ), #23309, .F. ) ;
#16040 =( BOUNDED_SURFACE ( )  B_SPLINE_SURFACE ( 3, 1, ( 
 ( #27302, #16369 ),
 ( #27155, #25162 ),
 ( #24748, #542 ),
 ( #22580, #7183 ) ),
 .UNSPECIFIED., .F., .F., .F. ) 
 B_SPLINE_SURFACE_WITH_KNOTS ( ( 4, 4 ),
 ( 2, 2 ),
 ( 0.000000000000000000, 1.000000000000000000 ),
 ( 0.000000000000000000, 1.000000000000000000 ),
 .UNSPECIFIED. ) 
 GEOMETRIC_REPRESENTATION_ITEM ( )  RATIONAL_B_SPLINE_SURFACE ( (
 ( 1.000000000000000000, 1.000000000000000000),
 ( 0.9960225298536222738, 0.9999952330161893110),
 ( 0.9960225298536222738, 0.9999952330161893110),
 ( 1.000000000000000000, 1.000000000000000000) ) ) 
 REPRESENTATION_ITEM ( '' )  SURFACE ( )  );
#16041 = CARTESIAN_POINT ( 'NONE',  ( -90.83090735639699176, 0.000000000000000000, 0.000000000000000000 ) ) ;
#16042 = DIRECTION ( 'NONE',  ( -1.000000000000000000, -0.000000000000000000, -0.000000000000000000 ) ) ;
#16043 = CARTESIAN_POINT ( 'NONE',  ( -1.045287976400365970, 1.530335034934747318, 45.76855895860941814 ) ) ;
#16044 = ADVANCED_FACE ( 'NONE', ( #22868 ), #11514, .T. ) ;
#16045 = ORIENTED_EDGE ( 'NONE', *, *, #19949, .T. ) ;
#16046 = VERTEX_POINT ( 'NONE', #18367 ) ;
#16047 = CARTESIAN_POINT ( 'NONE',  ( -22.34422965417126150, -17.95715691811022552, 33.39267070835840912 ) ) ;
#16049 = CARTESIAN_POINT ( 'NONE',  ( -22.23226125620930560, 7.677408153694024406, -30.68305173820428067 ) ) ;
#16048 = CARTESIAN_POINT ( 'NONE',  ( 25.64708228042119487, 66.39944550735394557, -91.32398912286959103 ) ) ;
#16050 = CARTESIAN_POINT ( 'NONE',  ( -24.53237795827028833, 3.868415699416160258, 33.71192251888858493 ) ) ;
#16051 = CARTESIAN_POINT ( 'NONE',  ( 109.1586059443104944, 0.001740416220250473730, -0.006856640434645987388 ) ) ;
#16052 = CARTESIAN_POINT ( 'NONE',  ( 32.73300124599732186, 0.000000000000000000, 0.000000000000000000 ) ) ;
#16053 = FACE_OUTER_BOUND ( 'NONE', #21946, .T. ) ;
#16054 = EDGE_CURVE ( 'NONE', #10527, #18593, #15643, .T. ) ;
#16055 = ORIENTED_EDGE ( 'NONE', *, *, #21886, .T. ) ;
#16056 = CARTESIAN_POINT ( 'NONE',  ( 109.1589550718175161, -0.004269295012381961116, 0.006257602293702343825 ) ) ;
#16057 = CARTESIAN_POINT ( 'NONE',  ( -10.86508079875774158, -50.67624451685647102, -6.877801422380581009 ) ) ;
#16058 = DIRECTION ( 'NONE',  ( 0.000000000000000000, 0.000000000000000000, 1.000000000000000000 ) ) ;
#16059 = VERTEX_POINT ( 'NONE', #24447 ) ;
#16060 = CARTESIAN_POINT ( 'NONE',  ( -23.79223135445718995, -7.157574570129374258, -32.40779366744832402 ) ) ;
#16061 = ORIENTED_EDGE ( 'NONE', *, *, #14566, .T. ) ;
#16062 = CARTESIAN_POINT ( 'NONE',  ( -1.045287976400351981, -15.59869763335126436, -43.05558670614231431 ) ) ;
#16063 = CARTESIAN_POINT ( 'NONE',  ( 13.84597867724985143, 10.56985607909801850, 146.3210145202068873 ) ) ;
#16064 = CARTESIAN_POINT ( 'NONE',  ( 1.833485406944043827, -132.3460930279895535, 59.50871042846178938 ) ) ;
#16065 = ORIENTED_EDGE ( 'NONE', *, *, #12290, .F. ) ;
#16066 = DIRECTION ( 'NONE',  ( -1.000000000000000000, -0.000000000000000000, -0.000000000000000000 ) ) ;
#16067 = ORIENTED_EDGE ( 'NONE', *, *, #3349, .F. ) ;
#16068 = CARTESIAN_POINT ( 'NONE',  ( 5.340103556456534228, 135.6222865117690617, -57.86178752079183596 ) ) ;
#16069 = VERTEX_POINT ( 'NONE', #6883 ) ;
#16070 = CARTESIAN_POINT ( 'NONE',  ( 10.93730112725978287, -133.3192575531804209, 71.28103789254889477 ) ) ;
#16071 = EDGE_CURVE ( 'NONE', #16310, #5798, #1568, .T. ) ;
#16072 = CARTESIAN_POINT ( 'NONE',  ( 1.834118845439484335, 117.5010238212710050, -85.14950727125739149 ) ) ;
#16073 = CARTESIAN_POINT ( 'NONE',  ( -25.21435515916025594, 1.749597353048488237E-16, -4.373993382621220594E-17 ) ) ;
#16074 = LINE ( 'NONE', #24745, #7437 ) ;
#16075 = EDGE_CURVE ( 'NONE', #22524, #9224, #18366, .T. ) ;
#16076 = VERTEX_POINT ( 'NONE', #9174 ) ;
#16077 = CARTESIAN_POINT ( 'NONE',  ( -24.53237795827028123, -6.738475012719871593, 33.25734978085275628 ) ) ;
#16078 = CARTESIAN_POINT ( 'NONE',  ( -1.031422197589711764, -44.01264471863837713, 12.69107518035547777 ) ) ;
#16079 = CARTESIAN_POINT ( 'NONE',  ( 26.11404676487257603, 98.61392875273364211, 55.62948129436280453 ) ) ;
#16080 = ORIENTED_EDGE ( 'NONE', *, *, #9388, .T. ) ;
#16081 = EDGE_CURVE ( 'NONE', #21691, #8288, #23559, .T. ) ;
#16082 = ORIENTED_EDGE ( 'NONE', *, *, #8466, .F. ) ;
#16083 = ORIENTED_EDGE ( 'NONE', *, *, #2462, .F. ) ;
#16084 = CARTESIAN_POINT ( 'NONE',  ( -8.786685647604892679, -53.04920435127177569, 7.199674155859498548 ) ) ;
#16085 = LINE ( 'NONE', #11632, #9329 ) ;
#16087 = CARTESIAN_POINT ( 'NONE',  ( -55.24271866751342941, -0.009388511352197387999, -0.001425019990782294558 ) ) ;
#16086 = CARTESIAN_POINT ( 'NONE',  ( 109.1592201516379674, 0.003476928926125392744, -0.007051465909551727154 ) ) ;
#16088 = CARTESIAN_POINT ( 'NONE',  ( 30.59138290137886784, -114.2039707400270601, -21.51300488027244739 ) ) ;
#16089 = CARTESIAN_POINT ( 'NONE',  ( 1.833485406944043827, 144.2578170162062747, 15.69895494453433393 ) ) ;
#16090 = DIRECTION ( 'NONE',  ( 0.000000000000000000, 1.000000000000000000, -6.938893903907228378E-16 ) ) ;
#16091 = CARTESIAN_POINT ( 'NONE',  ( -8.786685647604890903, -52.67761315067279781, 9.545808661481174795 ) ) ;
#16092 = VERTEX_POINT ( 'NONE', #14339 ) ;
#16093 = CARTESIAN_POINT ( 'NONE',  ( 109.1721716018069515, -0.005082060336465163246, -0.01629455849719228799 ) ) ;
#16094 = CARTESIAN_POINT ( 'NONE',  ( 5.340103556456485379, -100.3626145793569577, 108.0219267027626984 ) ) ;
#16095 = CARTESIAN_POINT ( 'NONE',  ( 25.64703792032471341, 11.95040607427984725, 112.2770217641848660 ) ) ;
#16096 = PLANE ( 'NONE',  #1368 ) ;
#16097 = CARTESIAN_POINT ( 'NONE',  ( -20.57838717382308147, -27.96569011373078339, 10.78122205917029675 ) ) ;
#16098 = CARTESIAN_POINT ( 'NONE',  ( 2.433796855181205476, -28.83182736670433499, -142.6247129145651229 ) ) ;
#16099 = CONICAL_SURFACE ( 'NONE', #12855, 117.6351876552689504, 0.9945805576725580410 ) ;
#16100 = ORIENTED_EDGE ( 'NONE', *, *, #28034, .F. ) ;
#16101 = CARTESIAN_POINT ( 'NONE',  ( 109.1721716018069515, -0.01699510305643761945, 0.001583175916617738993 ) ) ;
#16102 = CARTESIAN_POINT ( 'NONE',  ( 26.11404676487257603, -45.01677474591340911, -103.8885755249573606 ) ) ;
#16103 = CARTESIAN_POINT ( 'NONE',  ( 1.832998868059858122, -85.72499093308182694, 117.0819875546692543 ) ) ;
#16104 = VERTEX_POINT ( 'NONE', #25455 ) ;
#16105 = ORIENTED_EDGE ( 'NONE', *, *, #28134, .T. ) ;
#16106 = ORIENTED_EDGE ( 'NONE', *, *, #7284, .T. ) ;
#16107 = CARTESIAN_POINT ( 'NONE',  ( 26.11404676487257603, -110.5078194225162918, 24.64483677384812665 ) ) ;
#16108 = CARTESIAN_POINT ( 'NONE',  ( -55.24300891470650754, 0.006048736206179803135, 0.007734635432136488173 ) ) ;
#16109 = VECTOR ( 'NONE', #20588, 1000.000000000000114 ) ;
#16111 = CIRCLE ( 'NONE', #24406, 151.1787379149930359 ) ;
#16110 = CARTESIAN_POINT ( 'NONE',  ( -28.13707043255157103, -21.52861750560933984, 7.802116958609231823 ) ) ;
#16112 = DIRECTION ( 'NONE',  ( -0.7563875759206388771, 0.4122509917856786443, 0.5078650950445640078 ) ) ;
#16113 = CARTESIAN_POINT ( 'NONE',  ( -8.786685647604898008, 38.68584556812353981, 37.00619870957891777 ) ) ;
#16114 = EDGE_CURVE ( 'NONE', #26886, #19738, #5339, .T. ) ;
#16115 = CONICAL_SURFACE ( 'NONE', #18883, 117.6351876552689504, 0.9945805576725580410 ) ;
#16116 = CARTESIAN_POINT ( 'NONE',  ( 109.1586900883932856, -0.0006456433529069550677, 0.007109207791180748720 ) ) ;
#16117 = CARTESIAN_POINT ( 'NONE',  ( -20.20700224038492010, -0.9908225410476447781, 29.58392382092673500 ) ) ;
#16118 = ORIENTED_EDGE ( 'NONE', *, *, #11244, .T. ) ;
#16119 = CIRCLE ( 'NONE', #3723, 151.1787379149930359 ) ;
#16120 = EDGE_CURVE ( 'NONE', #1416, #16414, #23157, .T. ) ;
#16121 = ORIENTED_EDGE ( 'NONE', *, *, #12808, .T. ) ;
#16122 = CARTESIAN_POINT ( 'NONE',  ( 9.884929003653608603, -124.2095058357583213, 85.04731144912473439 ) ) ;
#16123 = CARTESIAN_POINT ( 'NONE',  ( 2.433796855181205476, -31.67151202413066713, 142.0211193075554945 ) ) ;
#16124 = CARTESIAN_POINT ( 'NONE',  ( -1.056502255334265339, 43.40574022158794065, 14.64009593116057317 ) ) ;
#16125 = EDGE_CURVE ( 'NONE', #23136, #17852, #21252, .T. ) ;
#16126 = CARTESIAN_POINT ( 'NONE',  ( 1.833485406944043827, 96.69979900902167458, 108.1939177044929323 ) ) ;
#16127 = CARTESIAN_POINT ( 'NONE',  ( -2.911734481061392987, 2.802366807346851285, 47.57875121082947345 ) ) ;
#16128 = CARTESIAN_POINT ( 'NONE',  ( 1.833485406944043827, -138.1714136985311256, 44.33323125129879116 ) ) ;
#16129 = CARTESIAN_POINT ( 'NONE',  ( 32.73300124599732186, 0.000000000000000000, 0.000000000000000000 ) ) ;
#16130 = ORIENTED_EDGE ( 'NONE', *, *, #17892, .T. ) ;
#16131 = DIRECTION ( 'NONE',  ( 0.000000000000000000, 5.223019709708233256E-21, -1.000000000000000000 ) ) ;
#16132 = CARTESIAN_POINT ( 'NONE',  ( -1.045287976400362417, -1.530335034934427574, -45.76855895860943235 ) ) ;
#16133 = AXIS2_PLACEMENT_3D ( 'NONE', #20324, #616, #24374 ) ;
#16135 = CARTESIAN_POINT ( 'NONE',  ( -1.155001620486259206, 44.25209926692307505, -12.20337535396694051 ) ) ;
#16134 = B_SPLINE_CURVE_WITH_KNOTS ( 'NONE', 3,
 ( #10920, #12783, #21571, #26171, #19550, #17382, #2255, #17246 ),
 .UNSPECIFIED., .F., .F.,
 ( 4, 2, 2, 4 ),
 ( 7.757919228897728493E-18, 0.0002429592666046879546, 0.0004859185332093681571, 0.0009718370664186953313 ),
 .UNSPECIFIED. ) ;
#16136 = CARTESIAN_POINT ( 'NONE',  ( -2.265401668238145483, -39.53028715828216377, 25.45016726748356817 ) ) ;
#16137 = CARTESIAN_POINT ( 'NONE',  ( 25.64681081121879203, -107.5125461021400355, -34.49579773461893950 ) ) ;
#16138 = ORIENTED_EDGE ( 'NONE', *, *, #18278, .F. ) ;
#16139 = DIRECTION ( 'NONE',  ( 0.000000000000000000, 0.000000000000000000, 1.000000000000000000 ) ) ;
#16140 = CIRCLE ( 'NONE', #2801, 117.6351876552689504 ) ;
#16141 = ORIENTED_EDGE ( 'NONE', *, *, #9688, .F. ) ;
#16142 = CIRCLE ( 'NONE', #11535, 12.50000000000000178 ) ;
#16143 = ORIENTED_EDGE ( 'NONE', *, *, #4847, .T. ) ;
#16144 = EDGE_LOOP ( 'NONE', ( #3871, #27935, #18523, #17531 ) ) ;
#16145 = CARTESIAN_POINT ( 'NONE',  ( -55.24300891470650754, 0.009812809446893281523, -0.0003472257464216086005 ) ) ;
#16146 = CARTESIAN_POINT ( 'NONE',  ( -55.24271866751342941, 0.009369360294294836952, -0.001545935011626992572 ) ) ;
#16147 = CARTESIAN_POINT ( 'NONE',  ( 109.1589550718175161, 0.006445391216541647428, -0.003980125429509243432 ) ) ;
#16148 = ADVANCED_FACE ( 'NONE', ( #18668 ), #22015, .T. ) ;
#16149 = CARTESIAN_POINT ( 'NONE',  ( 1.833206310202334155, -14.42724831649452000, 144.3905118062893393 ) ) ;
#16150 = CARTESIAN_POINT ( 'NONE',  ( -8.786685647604890903, 7.199674155858966529, -53.04920435127184675 ) ) ;
#16151 = CARTESIAN_POINT ( 'NONE',  ( 2.263178607246657759, -144.7392885066942938, -13.80342482180235208 ) ) ;
#16152 = CONICAL_SURFACE ( 'NONE', #7908, 117.6351876552689504, 0.9945805576725580410 ) ;
#16153 = CARTESIAN_POINT ( 'NONE',  ( 2.433796855181205476, 1.451562450951669803, -145.5024947199069345 ) ) ;
#16154 = CARTESIAN_POINT ( 'NONE',  ( 109.1586059443104944, -0.006260042619943072088, -0.003294606663354631478 ) ) ;
#16155 = AXIS2_PLACEMENT_3D ( 'NONE', #24617, #4437, #11209 ) ;
#16156 = CARTESIAN_POINT ( 'NONE',  ( 1.833485406944043827, -30.69200235379031838, 141.8265699653866250 ) ) ;
#16157 = CARTESIAN_POINT ( 'NONE',  ( -20.38016308990357572, -27.81387210821415223, 10.62413300761014945 ) ) ;
#16158 = CARTESIAN_POINT ( 'NONE',  ( 1.834118845439484335, -30.34413640949792423, 141.9019470378987080 ) ) ;
#16159 = CARTESIAN_POINT ( 'NONE',  ( 25.98107933586721074, -55.61918067932663234, -98.51796269673104689 ) ) ;
#16160 = VECTOR ( 'NONE', #22984, 1000.000000000000000 ) ;
#16162 = CARTESIAN_POINT ( 'NONE',  ( 10.93730112725972070, -26.59437931460858451, 148.8212007290659642 ) ) ;
#16161 = CARTESIAN_POINT ( 'NONE',  ( -25.21435515916043713, 6.169479169075932745, 34.05351380035326514 ) ) ;
#16163 = CARTESIAN_POINT ( 'NONE',  ( -1.044557008772710516, -1.643388457097570088, 45.76404748504492659 ) ) ;
#16164 = FACE_OUTER_BOUND ( 'NONE', #2820, .T. ) ;
#16165 = CARTESIAN_POINT ( 'NONE',  ( -55.24728320129491266, -0.01453410071985621575, -0.0006547948648749734972 ) ) ;
#16166 = CARTESIAN_POINT ( 'NONE',  ( 2.430230287190572103, -98.44218333480843341, 107.1617224697460813 ) ) ;
#16167 = CARTESIAN_POINT ( 'NONE',  ( 25.64704443564076186, 83.99864088993871292, -75.45310550990073750 ) ) ;
#16168 = LINE ( 'NONE', #24970, #17106 ) ;
#16169 = VERTEX_POINT ( 'NONE', #25156 ) ;
#16170 = CARTESIAN_POINT ( 'NONE',  ( -20.24399999263414429, 23.20123049637393464, 18.44171895251370330 ) ) ;
#16171 = CARTESIAN_POINT ( 'NONE',  ( -20.57838717382308147, -23.26537097894090778, 18.89542499756525729 ) ) ;
#16172 = ORIENTED_EDGE ( 'NONE', *, *, #9897, .F. ) ;
#16173 = ORIENTED_EDGE ( 'NONE', *, *, #2691, .T. ) ;
#16174 = ORIENTED_EDGE ( 'NONE', *, *, #12117, .T. ) ;
#16175 = CARTESIAN_POINT ( 'NONE',  ( 13.36082413113063083, 94.94363694444052726, 119.8836995922729898 ) ) ;
#16176 = EDGE_CURVE ( 'NONE', #6096, #23697, #18808, .T. ) ;
#16177 = CARTESIAN_POINT ( 'NONE',  ( 10.93730112725945247, 108.9902118373741331, 104.7670965581011302 ) ) ;
#16178 = AXIS2_PLACEMENT_3D ( 'NONE', #6327, #15076, #20642 ) ;
#16179 = ADVANCED_FACE ( 'NONE', ( #18528 ), #7678, .F. ) ;
#16180 = CARTESIAN_POINT ( 'NONE',  ( 32.73300124599737160, -116.5274707358854158, -16.10546300444944023 ) ) ;
#16181 = EDGE_CURVE ( 'NONE', #16536, #1646, #19342, .T. ) ;
#16182 = CARTESIAN_POINT ( 'NONE',  ( 1.833691583653541235, 144.3515375443197115, -14.81406002961166912 ) ) ;
#16183 = CARTESIAN_POINT ( 'NONE',  ( -55.24728320129491266, -0.01137345571547045305, -0.009072670231978460439 ) ) ;
#16184 = CARTESIAN_POINT ( 'NONE',  ( -21.41427618760447160, -29.81030852927061758, 7.777551129310369404 ) ) ;
#16185 = CARTESIAN_POINT ( 'NONE',  ( -1.031422197589711764, 15.60268798220637798, -43.06660437151313658 ) ) ;
#16186 = CARTESIAN_POINT ( 'NONE',  ( -1.583189561560256253, 36.01941156322789794, -29.24830400313178203 ) ) ;
#16187 = CARTESIAN_POINT ( 'NONE',  ( -20.21097721650786738, 9.464413208035470149, 28.05863614620928459 ) ) ;
#16188 = CARTESIAN_POINT ( 'NONE',  ( 109.1589550718175161, 0.006826119083824131080, -0.003284595046935060401 ) ) ;
#16189 = CARTESIAN_POINT ( 'NONE',  ( 25.98107933586740259, 83.34070894055855661, 76.50887835172548535 ) ) ;
#16190 = ORIENTED_EDGE ( 'NONE', *, *, #24162, .F. ) ;
#16191 = EDGE_LOOP ( 'NONE', ( #918, #23867, #8235, #21746 ) ) ;
#16192 = FACE_OUTER_BOUND ( 'NONE', #1347, .T. ) ;
#16193 = CARTESIAN_POINT ( 'NONE',  ( -1.583189561560255143, -36.01941156322808979, -29.24830400313152623 ) ) ;
#16194 = CARTESIAN_POINT ( 'NONE',  ( -8.786685647604890903, -23.24040270374424466, -48.22796981442760256 ) ) ;
#16195 = CARTESIAN_POINT ( 'NONE',  ( 2.108985857320902824, 86.43462668039136076, 116.7869613039522676 ) ) ;
#16196 = ORIENTED_EDGE ( 'NONE', *, *, #5462, .F. ) ;
#16197 = VECTOR ( 'NONE', #25729, 1000.000000000000227 ) ;
#16198 = EDGE_LOOP ( 'NONE', ( #24526, #974, #21071, #24774, #2390, #20726, #19072, #12332, #20520, #9042, #1149, #11050, #7619, #2496, #25747, #6787, #5877, #12055, #11801, #19922, #1122, #742, #26042, #10036, #25779, #15252, #20583, #20414, #14700, #19352, #1628, #20095, #15554, #996, #5001, #18852, #14350, #23845, #13286, #15958, #7968, #10254, #22301, #16863, #18703, #16893, #15899, #3904, #11926, #19766, #25983, #6644, #18313, #28218, #26394, #11062, #4208, #11855, #13228, #3055, #16266, #2876, #10904, #21534 ) ) ;
#16199 = CARTESIAN_POINT ( 'NONE',  ( -90.83090735639699176, 0.000000000000000000, 0.000000000000000000 ) ) ;
#16200 = VECTOR ( 'NONE', #7050, 1000.000000000000000 ) ;
#16201 = CARTESIAN_POINT ( 'NONE',  ( -1.045287976400365970, 45.76855895860946077, 1.530335034933974381 ) ) ;
#16202 = CARTESIAN_POINT ( 'NONE',  ( -1.058197053496161555, -38.06270006878834522, 25.48582931365511328 ) ) ;
#16203 = ORIENTED_EDGE ( 'NONE', *, *, #3094, .F. ) ;
#16204 = CARTESIAN_POINT ( 'NONE',  ( 25.64700659047696618, -97.89757946487048912, 56.25842064176056567 ) ) ;
#16205 = CARTESIAN_POINT ( 'NONE',  ( 2.433796855181233454, 116.8607839509068498, -86.69855925933855190 ) ) ;
#16206 = ADVANCED_FACE ( 'NONE', ( #3544 ), #23038, .T. ) ;
#16207 = CARTESIAN_POINT ( 'NONE',  ( -4.473127245936431073, -31.51789735524165081, 37.94261489385753094 ) ) ;
#16208 = ORIENTED_EDGE ( 'NONE', *, *, #14907, .F. ) ;
#16209 = CARTESIAN_POINT ( 'NONE',  ( -55.24390624410018802, -0.001811362924359030029, -0.01027195578987783083 ) ) ;
#16210 = EDGE_CURVE ( 'NONE', #546, #8144, #5277, .T. ) ;
#16211 = ADVANCED_FACE ( 'NONE', ( #23724 ), #10587, .F. ) ;
#16212 = ORIENTED_EDGE ( 'NONE', *, *, #15351, .F. ) ;
#16213 = CARTESIAN_POINT ( 'NONE',  ( 32.73300124599739291, -105.8473486001047235, -51.32617430725011332 ) ) ;
#16214 = ORIENTED_EDGE ( 'NONE', *, *, #5701, .F. ) ;
#16215 = B_SPLINE_CURVE_WITH_KNOTS ( 'NONE', 3,
 ( #21264, #19239, #1543, #10349, #14916, #19111, #28012 ),
 .UNSPECIFIED., .F., .F.,
 ( 4, 3, 4 ),
 ( 0.000000000000000000, 0.009512539173626361963, 0.02506242213020844212 ),
 .UNSPECIFIED. ) ;
#16217 =( BOUNDED_SURFACE ( )  B_SPLINE_SURFACE ( 3, 1, ( 
 ( #20784, #18632 ),
 ( #9864, #7717 ),
 ( #27405, #14298 ),
 ( #16471, #25261 ) ),
 .UNSPECIFIED., .F., .F., .F. ) 
 B_SPLINE_SURFACE_WITH_KNOTS ( ( 4, 4 ),
 ( 2, 2 ),
 ( 0.000000000000000000, 1.000000000000000000 ),
 ( 0.000000000000000000, 1.000000000000000000 ),
 .UNSPECIFIED. ) 
 GEOMETRIC_REPRESENTATION_ITEM ( )  RATIONAL_B_SPLINE_SURFACE ( (
 ( 1.000000000000000000, 1.000000000000000000),
 ( 0.9934239774497837239, 0.8357310067453919133),
 ( 0.9934239774497837239, 0.8357310067453919133),
 ( 1.000000000000000000, 1.000000000000000000) ) ) 
 REPRESENTATION_ITEM ( '' )  SURFACE ( )  );
#16216 = VECTOR ( 'NONE', #23625, 999.9999999999998863 ) ;
#16218 = CARTESIAN_POINT ( 'NONE',  ( 10.93730112725990011, -115.5857507957697976, -97.44200844886394464 ) ) ;
#16219 = CIRCLE ( 'NONE', #7033, 117.6351876552689504 ) ;
#16220 = B_SPLINE_CURVE_WITH_KNOTS ( 'NONE', 3,
 ( #7079, #26346, #17703, #15251, #2737, #9078, #15838, #288, #24491, #24342 ),
 .UNSPECIFIED., .F., .F.,
 ( 4, 3, 3, 4 ),
 ( 0.001530725384384964971, 0.001531419946797918505, 0.002296279302920153399, 0.003061450627205758099 ),
 .UNSPECIFIED. ) ;
#16221 = CARTESIAN_POINT ( 'NONE',  ( 28.37603512858449051, 109.6581134439367560, 33.74339723237822852 ) ) ;
#16222 = CARTESIAN_POINT ( 'NONE',  ( -55.24300891470650754, 0.009225237711101738972, -0.003362556190412665288 ) ) ;
#16223 = CARTESIAN_POINT ( 'NONE',  ( -55.25297051322618813, 0.01466904165775564234, -0.002853887643044135131 ) ) ;
#16224 = ORIENTED_EDGE ( 'NONE', *, *, #8461, .T. ) ;
#16225 = CARTESIAN_POINT ( 'NONE',  ( 30.59138290137876481, 49.72302320601791337, 105.0379801549009784 ) ) ;
#16226 = CARTESIAN_POINT ( 'NONE',  ( -20.57838717382308502, 25.16001208503106668, -16.28767523336130196 ) ) ;
#16227 = VERTEX_POINT ( 'NONE', #10883 ) ;
#16228 = VERTEX_POINT ( 'NONE', #21820 ) ;
#16229 = EDGE_LOOP ( 'NONE', ( #22669, #3764, #26117, #4517 ) ) ;
#16230 = CARTESIAN_POINT ( 'NONE',  ( 25.86096068574579832, -90.87263912324372939, -67.25583614083940631 ) ) ;
#16231 = DIRECTION ( 'NONE',  ( 1.000000000000000000, -6.938893903907226837E-18, 1.734723475976806709E-18 ) ) ;
#16233 = CARTESIAN_POINT ( 'NONE',  ( 2.430230287190581429, -142.0258656395019443, -31.67257033707648262 ) ) ;
#16232 = CARTESIAN_POINT ( 'NONE',  ( 109.1624594426973260, -0.01102230012606011597, 0.01154818537150955997 ) ) ;
#16234 = CARTESIAN_POINT ( 'NONE',  ( 19.66333377628726353, 46.81583828063228481, -129.5498775999577958 ) ) ;
#16235 = CARTESIAN_POINT ( 'NONE',  ( -28.41354790283022069, 21.64275480268759821, 8.345538364876851745 ) ) ;
#16236 = CARTESIAN_POINT ( 'NONE',  ( -23.77929240705206837, 32.66578242509746133, -15.74261278740683778 ) ) ;
#16237 = CARTESIAN_POINT ( 'NONE',  ( 21.16825799904898986, -135.3612955721067692, 4.416019842157926867 ) ) ;
#16238 = EDGE_LOOP ( 'NONE', ( #24556, #19452, #570, #19102 ) ) ;
#16239 = CARTESIAN_POINT ( 'NONE',  ( -20.20700224038492721, -29.58392382092674211, -0.9908225410477480288 ) ) ;
#16240 = CARTESIAN_POINT ( 'NONE',  ( -1.464342487929867209, -16.57334911911542363, -43.13914623307952922 ) ) ;
#16241 = CARTESIAN_POINT ( 'NONE',  ( 32.73300124599732186, 0.000000000000000000, 0.000000000000000000 ) ) ;
#16242 = CARTESIAN_POINT ( 'NONE',  ( -28.41354790283022069, -23.16239616762929998, 1.249099604787319295 ) ) ;
#16243 = CARTESIAN_POINT ( 'NONE',  ( 109.1586900883932856, -0.004277182003220988613, 0.005715190711488708428 ) ) ;
#16244 = B_SPLINE_CURVE_WITH_KNOTS ( 'NONE', 3,
 ( #13695, #7245, #4927, #22650, #2921, #9831, #18600 ),
 .UNSPECIFIED., .F., .F.,
 ( 4, 3, 4 ),
 ( 5.683119316658233806E-16, 0.02816610861753246833, 0.04000277880656280538 ),
 .UNSPECIFIED. ) ;
#16245 = CARTESIAN_POINT ( 'NONE',  ( 109.1587776205901861, 0.007151389024635753690, -0.001605238040368390639 ) ) ;
#16246 = ORIENTED_EDGE ( 'NONE', *, *, #15493, .F. ) ;
#16247 = CARTESIAN_POINT ( 'NONE',  ( 109.1592201516379674, -0.002720803050361364321, 0.007376275279030867701 ) ) ;
#16248 =( GEOMETRIC_REPRESENTATION_CONTEXT ( 3 ) GLOBAL_UNCERTAINTY_ASSIGNED_CONTEXT ( ( #26936 ) ) GLOBAL_UNIT_ASSIGNED_CONTEXT ( ( #22572, #9170, #20238 ) ) REPRESENTATION_CONTEXT ( 'NONE', 'WORKASPACE' ) );
#16249 = CIRCLE ( 'NONE', #3837, 53.53553390275978785 ) ;
#16250 = EDGE_CURVE ( 'NONE', #16696, #25619, #7026, .T. ) ;
#16251 = CARTESIAN_POINT ( 'NONE',  ( -20.37983603106074071, 16.25728007463443703, 24.94323704205420000 ) ) ;
#16252 = CARTESIAN_POINT ( 'NONE',  ( -1.155001620486248992, 12.20337535396741124, 44.25209926692296136 ) ) ;
#16253 = ADVANCED_FACE ( 'NONE', ( #10751 ), #12425, .F. ) ;
#16254 = B_SPLINE_CURVE_WITH_KNOTS ( 'NONE', 3,
 ( #4505, #19623, #19490, #19762, #17320, #26526 ),
 .UNSPECIFIED., .F., .F.,
 ( 4, 2, 4 ),
 ( 0.000000000000000000, 0.0004335151646191504364, 0.0008670303292383008727 ),
 .UNSPECIFIED. ) ;
#16255 = ORIENTED_EDGE ( 'NONE', *, *, #6141, .T. ) ;
#16256 = ORIENTED_EDGE ( 'NONE', *, *, #16700, .F. ) ;
#16257 = EDGE_CURVE ( 'NONE', #11422, #10623, #8302, .T. ) ;
#16258 = B_SPLINE_CURVE_WITH_KNOTS ( 'NONE', 3,
 ( #12253, #14550, #8099, #19291, #21593, #1453 ),
 .UNSPECIFIED., .F., .F.,
 ( 4, 2, 4 ),
 ( 0.000000000000000000, 0.0004335184443140242989, 0.0008670368886280485979 ),
 .UNSPECIFIED. ) ;
#16259 = CARTESIAN_POINT ( 'NONE',  ( -2.904412668506652473, -17.42365698954667863, 44.35433137608958276 ) ) ;
#16260 = CARTESIAN_POINT ( 'NONE',  ( -20.20700224038492010, 27.82980252387833886, 10.08426345511560207 ) ) ;
#16261 = ADVANCED_FACE ( 'NONE', ( #24131 ), #18297, .F. ) ;
#16262 = FACE_OUTER_BOUND ( 'NONE', #9165, .T. ) ;
#16263 =( BOUNDED_SURFACE ( )  B_SPLINE_SURFACE ( 3, 1, ( 
 ( #20222, #518 ),
 ( #9314, #18072 ),
 ( #16794, #10452 ),
 ( #3254, #21083 ) ),
 .UNSPECIFIED., .F., .F., .F. ) 
 B_SPLINE_SURFACE_WITH_KNOTS ( ( 4, 4 ),
 ( 2, 2 ),
 ( 0.000000000000000000, 1.000000000000000000 ),
 ( 0.000000000000000000, 1.000000000000000000 ),
 .UNSPECIFIED. ) 
 GEOMETRIC_REPRESENTATION_ITEM ( )  RATIONAL_B_SPLINE_SURFACE ( (
 ( 1.000000000000000000, 1.000000000000000000),
 ( 0.9956975270656955868, 0.8568959468854907557),
 ( 0.9956975270656955868, 0.8568959468854907557),
 ( 1.000000000000000000, 1.000000000000000000) ) ) 
 REPRESENTATION_ITEM ( '' )  SURFACE ( )  );
#16264 = FACE_OUTER_BOUND ( 'NONE', #25201, .T. ) ;
#16265 = CARTESIAN_POINT ( 'NONE',  ( 10.93730112725945247, 108.9902118373741331, 104.7670965581011302 ) ) ;
#16266 = ORIENTED_EDGE ( 'NONE', *, *, #7985, .T. ) ;
#16267 = CARTESIAN_POINT ( 'NONE',  ( -1.239374126674604337, 28.97829083655491544, 35.79060836339782270 ) ) ;
#16268 = CARTESIAN_POINT ( 'NONE',  ( 1.833721034905632097, 44.50273803002120587, -138.1171912769426058 ) ) ;
#16269 = DIRECTION ( 'NONE',  ( 0.7637818620346802367, -0.2198041754873842346, 0.6068965246771050870 ) ) ;
#16270 = ORIENTED_EDGE ( 'NONE', *, *, #25718, .T. ) ;
#16271 = ORIENTED_EDGE ( 'NONE', *, *, #18083, .F. ) ;
#16272 = CARTESIAN_POINT ( 'NONE',  ( -18.41936578851709427, -38.22933728004704790, -18.42310649277614232 ) ) ;
#16273 = CARTESIAN_POINT ( 'NONE',  ( 28.37599760073042177, 114.7183216384031397, 1.794331790579828390 ) ) ;
#16274 = FACE_OUTER_BOUND ( 'NONE', #11889, .T. ) ;
#16275 = CARTESIAN_POINT ( 'NONE',  ( -9.156249394959713683, -38.17928057392020236, -38.89149400288393821 ) ) ;
#16276 = CARTESIAN_POINT ( 'NONE',  ( -55.24390624410018802, -0.001451500391950358120, -0.01032895241567008057 ) ) ;
#16277 = CARTESIAN_POINT ( 'NONE',  ( -1.619063947482201282, 16.67502769180561728, -43.26576862488438735 ) ) ;
#16278 = ORIENTED_EDGE ( 'NONE', *, *, #14398, .T. ) ;
#16279 = LINE ( 'NONE', #25075, #13217 ) ;
#16280 = CARTESIAN_POINT ( 'NONE',  ( -15.02187109954785704, -33.49412687891593521, -32.04062513125103351 ) ) ;
#16281 = FACE_OUTER_BOUND ( 'NONE', #26911, .T. ) ;
#16282 = DIRECTION ( 'NONE',  ( 0.000000000000000000, 5.223019709707975211E-21, -1.000000000000000000 ) ) ;
#16283 = CARTESIAN_POINT ( 'NONE',  ( 25.64699802086725455, -107.3112355540543206, 35.11755197949801754 ) ) ;
#16284 = ORIENTED_EDGE ( 'NONE', *, *, #9464, .T. ) ;
#16285 = CARTESIAN_POINT ( 'NONE',  ( 25.64681081121879203, -75.86069728269045243, 83.63051021305875565 ) ) ;
#16286 = ORIENTED_EDGE ( 'NONE', *, *, #9132, .T. ) ;
#16287 = EDGE_CURVE ( 'NONE', #23109, #22524, #23858, .T. ) ;
#16288 = ORIENTED_EDGE ( 'NONE', *, *, #25584, .T. ) ;
#16289 = ORIENTED_EDGE ( 'NONE', *, *, #9411, .F. ) ;
#16290 = DIRECTION ( 'NONE',  ( -1.000000000000000000, -0.000000000000000000, -0.000000000000000000 ) ) ;
#16291 = EDGE_CURVE ( 'NONE', #378, #23697, #21358, .T. ) ;
#16292 = CARTESIAN_POINT ( 'NONE',  ( 2.430230287190581429, -109.1043569252020689, 96.28466919684062475 ) ) ;
#16293 = CARTESIAN_POINT ( 'NONE',  ( 16.75465622695671186, 127.9746229614483752, 62.05388459345925867 ) ) ;
#16294 = B_SPLINE_CURVE_WITH_KNOTS ( 'NONE', 3,
 ( #6325, #13072, #2398, #21857, #21715, #4564, #12780, #17664 ),
 .UNSPECIFIED., .F., .F.,
 ( 4, 2, 2, 4 ),
 ( 0.000000000000000000, 0.002761524886576660186, 0.005523049773153320373, 0.01104609954630662340 ),
 .UNSPECIFIED. ) ;
#16295 = CARTESIAN_POINT ( 'NONE',  ( 109.1778270068192853, 0.008646067828078115095, -0.003465086990427118391 ) ) ;
#16296 = LINE ( 'NONE', #7826, #12430 ) ;
#16297 = DIRECTION ( 'NONE',  ( 0.000000000000000000, 0.000000000000000000, 1.000000000000000000 ) ) ;
#16298 = CARTESIAN_POINT ( 'NONE',  ( 1.833485406944043827, 132.3460930279890704, 59.50871042846269177 ) ) ;
#16299 = B_SPLINE_CURVE_WITH_KNOTS ( 'NONE', 3,
 ( #16909, #3805, #21223, #10438, #3515, #27705, #8273, #16778 ),
 .UNSPECIFIED., .F., .F.,
 ( 4, 2, 2, 4 ),
 ( 7.757919228897728493E-18, 0.0002429592666046734262, 0.0004859185332093391005, 0.0009718370664186894766 ),
 .UNSPECIFIED. ) ;
#16300 = CARTESIAN_POINT ( 'NONE',  ( 109.1586900883932856, -0.007088091345229661187, 0.0008465529156634868553 ) ) ;
#16301 =( BOUNDED_SURFACE ( )  B_SPLINE_SURFACE ( 3, 1, ( 
 ( #26686, #17769 ),
 ( #22093, #22537 ),
 ( #24266, #20069 ),
 ( #22248, #13732 ) ),
 .UNSPECIFIED., .F., .F., .F. ) 
 B_SPLINE_SURFACE_WITH_KNOTS ( ( 4, 4 ),
 ( 2, 2 ),
 ( 0.000000000000000000, 1.000000000000000000 ),
 ( 0.000000000000000000, 1.000000000000000000 ),
 .UNSPECIFIED. ) 
 GEOMETRIC_REPRESENTATION_ITEM ( )  RATIONAL_B_SPLINE_SURFACE ( (
 ( 1.000000000000000000, 1.000000000000000000),
 ( 0.9934239774497838349, 0.8357310067453913582),
 ( 0.9934239774497838349, 0.8357310067453913582),
 ( 1.000000000000000000, 1.000000000000000000) ) ) 
 REPRESENTATION_ITEM ( '' )  SURFACE ( )  );
#16302 = CARTESIAN_POINT ( 'NONE',  ( -8.786685647604898008, 38.68584556812353981, 37.00619870957891777 ) ) ;
#16303 = CARTESIAN_POINT ( 'NONE',  ( 25.64703792032473828, -75.66285916808242007, -83.80974623566366688 ) ) ;
#16304 = CARTESIAN_POINT ( 'NONE',  ( -1.259972190295307604, -25.19627397134270197, 38.49631882650675152 ) ) ;
#16305 = CARTESIAN_POINT ( 'NONE',  ( 109.1592201516379674, -0.005631912476303850730, 0.005485778713202916178 ) ) ;
#16306 = CARTESIAN_POINT ( 'NONE',  ( -55.25297051322618813, 0.01093108995495213273, 0.01019003092403696770 ) ) ;
#16307 = CARTESIAN_POINT ( 'NONE',  ( 25.86096068574580542, 112.3259320600845115, 12.80894308910771962 ) ) ;
#16308 = CARTESIAN_POINT ( 'NONE',  ( 2.063896406836609909, 84.29612368209309636, -118.3103904147673404 ) ) ;
#16309 = CARTESIAN_POINT ( 'NONE',  ( 32.73300124599736449, -114.2056417606550127, 28.19767303745571496 ) ) ;
#16310 = VERTEX_POINT ( 'NONE', #26800 ) ;
#16311 = CARTESIAN_POINT ( 'NONE',  ( 1.833485406944043827, -14.63699153649261575, -144.3694338680886347 ) ) ;
#16312 = VERTEX_POINT ( 'NONE', #18010 ) ;
#16313 = DIRECTION ( 'NONE',  ( 1.000000000000000000, -6.938893903907226837E-18, 1.734723475976806709E-18 ) ) ;
#16314 = CARTESIAN_POINT ( 'NONE',  ( -19.53423201713129842, 1.355459634611817431E-16, -3.388649086529543578E-17 ) ) ;
#16315 = ORIENTED_EDGE ( 'NONE', *, *, #16120, .F. ) ;
#16316 = ADVANCED_FACE ( 'NONE', ( #18159 ), #28384, .F. ) ;
#16317 = ORIENTED_EDGE ( 'NONE', *, *, #11370, .T. ) ;
#16318 = ORIENTED_EDGE ( 'NONE', *, *, #4445, .F. ) ;
#16319 = EDGE_CURVE ( 'NONE', #7007, #14740, #15420, .T. ) ;
#16320 = EDGE_CURVE ( 'NONE', #5123, #25702, #6310, .T. ) ;
#16321 = ORIENTED_EDGE ( 'NONE', *, *, #18184, .T. ) ;
#16322 = CARTESIAN_POINT ( 'NONE',  ( 2.430230287190581429, 60.50928654924932459, -132.3371620660944643 ) ) ;
#16323 = CARTESIAN_POINT ( 'NONE',  ( -23.79248802219731118, -28.61009539422396131, -16.82188324679470881 ) ) ;
#16324 = CARTESIAN_POINT ( 'NONE',  ( -55.25297051322618813, -0.01093108995494780980, 0.01019003092403480623 ) ) ;
#16325 = CARTESIAN_POINT ( 'NONE',  ( -4.473127245936434626, 37.94261489385718988, -31.51789735524207003 ) ) ;
#16326 = CARTESIAN_POINT ( 'NONE',  ( -1.323439229708141651, -2.317790194800056547, -46.01398008004440499 ) ) ;
#16327 = CARTESIAN_POINT ( 'NONE',  ( 2.433796855181233454, 71.49415740225254012, -126.7346379669248222 ) ) ;
#16328 = CARTESIAN_POINT ( 'NONE',  ( -1.044557008772713624, 28.22896138707370994, -36.05793264791354602 ) ) ;
#16329 = FACE_OUTER_BOUND ( 'NONE', #3932, .T. ) ;
#16330 = CARTESIAN_POINT ( 'NONE',  ( 2.108393763691172484, -86.43392821214661126, 116.7869873529606224 ) ) ;
#16331 = CARTESIAN_POINT ( 'NONE',  ( -1.050231094221204087, -14.39477892760331024, -43.47885872350351377 ) ) ;
#16332 = CARTESIAN_POINT ( 'NONE',  ( -1.045287976400362417, 37.92705037016796155, 25.66401692419947977 ) ) ;
#16333 = ORIENTED_EDGE ( 'NONE', *, *, #20304, .T. ) ;
#16334 = VERTEX_POINT ( 'NONE', #26649 ) ;
#16336 = DIRECTION ( 'NONE',  ( -0.7563875759206389882, 0.1685564395263298709, -0.6320336713238514648 ) ) ;
#16335 = CARTESIAN_POINT ( 'NONE',  ( -1.019300379054419947, -35.83762006677421397, -28.53917295602885318 ) ) ;
#16337 = CARTESIAN_POINT ( 'NONE',  ( -7.711401346138392121, -21.83927363365067364, -47.70038152767084227 ) ) ;
#16338 = CARTESIAN_POINT ( 'NONE',  ( 26.11404676487259024, -108.0249973236465308, -33.91085499298486639 ) ) ;
#16339 = CARTESIAN_POINT ( 'NONE',  ( 2.433796855181205476, -71.49415740224986848, -126.7346379669263001 ) ) ;
#16340 = EDGE_CURVE ( 'NONE', #9431, #6438, #3242, .T. ) ;
#16341 = ORIENTED_EDGE ( 'NONE', *, *, #7357, .F. ) ;
#16342 = CARTESIAN_POINT ( 'NONE',  ( 25.98107933586698337, 98.51796269673161532, -55.61918067932647602 ) ) ;
#16343 = CARTESIAN_POINT ( 'NONE',  ( 25.87036335909428431, -35.87755773825644923, -107.2165474610298332 ) ) ;
#16344 = CARTESIAN_POINT ( 'NONE',  ( -55.24271866751342941, -0.008488649505342596782, -0.004256484107795601053 ) ) ;
#16345 = ORIENTED_EDGE ( 'NONE', *, *, #1078, .F. ) ;
#16346 = B_SPLINE_CURVE_WITH_KNOTS ( 'NONE', 3,
 ( #17104, #8609, #26832, #20205, #8478, #28176 ),
 .UNSPECIFIED., .F., .F.,
 ( 4, 2, 4 ),
 ( 4.770489558936219510E-18, 0.0006311636237756751162, 0.001262327247551345245 ),
 .UNSPECIFIED. ) ;
#16347 = EDGE_CURVE ( 'NONE', #195, #8387, #17301, .T. ) ;
#16348 = B_SPLINE_CURVE_WITH_KNOTS ( 'NONE', 3,
 ( #17242, #19821, #17378, #11193, #26167, #10916, #17662, #26440 ),
 .UNSPECIFIED., .F., .F.,
 ( 4, 2, 2, 4 ),
 ( 6.938893903907228378E-18, 0.0002429588503611288571, 0.0004859177007222507754, 0.0009718354014444767226 ),
 .UNSPECIFIED. ) ;
#16349 = B_SPLINE_CURVE_WITH_KNOTS ( 'NONE', 3,
 ( #28118, #10722, #19487, #28251, #8552, #17317, #4224, #15145 ),
 .UNSPECIFIED., .F., .F.,
 ( 4, 2, 2, 4 ),
 ( 6.938893903907228378E-18, 0.0002429588503611293450, 0.0004859177007222517512, 0.0009718354014444924435 ),
 .UNSPECIFIED. ) ;
#16350 = CARTESIAN_POINT ( 'NONE',  ( 2.263178607246663976, 116.7985473178714955, -86.59154415224485035 ) ) ;
#16351 = DIRECTION ( 'NONE',  ( 0.000000000000000000, 5.223019709707975211E-21, -1.000000000000000000 ) ) ;
#16352 = APPLICATION_CONTEXT ( 'automotive_design' ) ;
#16353 = ORIENTED_EDGE ( 'NONE', *, *, #17831, .F. ) ;
#16354 = CARTESIAN_POINT ( 'NONE',  ( -20.57838717382308147, -27.96569011373093971, -10.78122205916989529 ) ) ;
#16355 = ORIENTED_EDGE ( 'NONE', *, *, #15679, .F. ) ;
#16356 = B_SPLINE_CURVE_WITH_KNOTS ( 'NONE', 3,
 ( #9231, #24214, #17989, #26775, #7088, #13245, #24355 ),
 .UNSPECIFIED., .F., .F.,
 ( 4, 3, 4 ),
 ( 1.309687503460226953E-17, 0.009512539173626405331, 0.02506242213020846293 ),
 .UNSPECIFIED. ) ;
#16357 = CARTESIAN_POINT ( 'NONE',  ( -20.24419206586952313, 7.929973069813410547, -28.55732805495818383 ) ) ;
#16358 = CARTESIAN_POINT ( 'NONE',  ( 2.430230287190572103, -116.8646894862406072, -86.70145658344777928 ) ) ;
#16359 = ORIENTED_EDGE ( 'NONE', *, *, #9716, .T. ) ;
#16360 = SHAPE_DEFINITION_REPRESENTATION ( #10845, #747 ) ;
#16361 = CARTESIAN_POINT ( 'NONE',  ( -1.583189561560256253, 38.94740041318330981, 25.21827308671188916 ) ) ;
#16362 = CARTESIAN_POINT ( 'NONE',  ( -9.156249394959706578, 38.17928057391991103, -38.89149400288420111 ) ) ;
#16363 = CARTESIAN_POINT ( 'NONE',  ( -20.37983603106074426, 29.73529213200291821, 1.508851015062683487 ) ) ;
#16364 = ORIENTED_EDGE ( 'NONE', *, *, #16012, .F. ) ;
#16365 = B_SPLINE_CURVE_WITH_KNOTS ( 'NONE', 3,
 ( #3015, #844, #13791, #18111 ),
 .UNSPECIFIED., .F., .F.,
 ( 4, 4 ),
 ( 3.469446951953614189E-18, 0.008383560773332722482 ),
 .UNSPECIFIED. ) ;
#16366 = CARTESIAN_POINT ( 'NONE',  ( 8.186469829614351212, -145.3272524103320222, -34.43598812953259625 ) ) ;
#16368 = CARTESIAN_POINT ( 'NONE',  ( 6.224689322667630975, 18.02516478984339088, -146.9579047224767692 ) ) ;
#16367 = DIRECTION ( 'NONE',  ( -0.000000000000000000, -1.000000000000000000, -3.469446951953603342E-16 ) ) ;
#16369 = CARTESIAN_POINT ( 'NONE',  ( 1.832998868059890096, 141.8272129421612817, -30.69214149073874864 ) ) ;
#16370 = ORIENTED_EDGE ( 'NONE', *, *, #17892, .F. ) ;
#16371 = ORIENTED_EDGE ( 'NONE', *, *, #21749, .F. ) ;
#16372 = ORIENTED_EDGE ( 'NONE', *, *, #7381, .T. ) ;
#16373 = CARTESIAN_POINT ( 'NONE',  ( -20.90916690077964546, -17.17795951644681907, -35.64494649500676360 ) ) ;
#16374 = CARTESIAN_POINT ( 'NONE',  ( -20.20997486282891131, -0.3303599360441825672, -29.60348406988234871 ) ) ;
#16376 = CARTESIAN_POINT ( 'NONE',  ( 10.93730112725969938, 56.95489579269752767, 140.0398180619111770 ) ) ;
#16375 = CARTESIAN_POINT ( 'NONE',  ( 109.1721716018069515, -0.01567407524361265347, 0.006757465437533703538 ) ) ;
#16377 = CARTESIAN_POINT ( 'NONE',  ( -22.23342874802668234, 29.33662284748876914, 11.82490389046284029 ) ) ;
#16378 = CARTESIAN_POINT ( 'NONE',  ( 1.833485406944043827, -132.3460930279887293, -59.50871042846357994 ) ) ;
#16379 = CARTESIAN_POINT ( 'NONE',  ( -25.21435515916043002, 31.17620025257588523, -15.02493970636157705 ) ) ;
#16380 = CARTESIAN_POINT ( 'NONE',  ( -1.619063947482201282, -44.80407745103776307, 11.94059994246206635 ) ) ;
#16381 = EDGE_CURVE ( 'NONE', #14740, #26927, #19704, .T. ) ;
#16382 = EDGE_LOOP ( 'NONE', ( #6392, #17964, #2196, #5800 ) ) ;
#16383 = CARTESIAN_POINT ( 'NONE',  ( 109.1624594426973260, -0.01033277910988589232, -0.01216903288310119090 ) ) ;
#16384 = CARTESIAN_POINT ( 'NONE',  ( -7.733045908741323693, -35.49239760110648945, 38.67583825854190138 ) ) ;
#16385 = CARTESIAN_POINT ( 'NONE',  ( -1.050230346682680560, 14.15335421912582170, -43.55729751025868524 ) ) ;
#16386 = CARTESIAN_POINT ( 'NONE',  ( 109.1592201516379674, -0.007845213074654437332, 0.0005146241775982539042 ) ) ;
#16387 = EDGE_CURVE ( 'NONE', #607, #19834, #1164, .T. ) ;
#16388 =( BOUNDED_SURFACE ( )  B_SPLINE_SURFACE ( 3, 1, ( 
 ( #23693, #4220 ),
 ( #8547, #3804 ),
 ( #3944, #13002 ),
 ( #21792, #17180 ) ),
 .UNSPECIFIED., .F., .F., .F. ) 
 B_SPLINE_SURFACE_WITH_KNOTS ( ( 4, 4 ),
 ( 2, 2 ),
 ( 0.000000000000000000, 1.000000000000000000 ),
 ( 0.000000000000000000, 1.000000000000000000 ),
 .UNSPECIFIED. ) 
 GEOMETRIC_REPRESENTATION_ITEM ( )  RATIONAL_B_SPLINE_SURFACE ( (
 ( 1.000000000000000000, 1.000000000000000000),
 ( 0.6386103224230302855, 0.9954351624131538845),
 ( 0.6386103224230302855, 0.9954351624131538845),
 ( 1.000000000000000000, 1.000000000000000000) ) ) 
 REPRESENTATION_ITEM ( '' )  SURFACE ( )  );
#16389 = CARTESIAN_POINT ( 'NONE',  ( -23.79248802219728987, 22.01156985585204851, 24.83956736572385893 ) ) ;
#16390 = CARTESIAN_POINT ( 'NONE',  ( 94.22246935314088034, -69.99999999999998579, -6.938893903907228378E-15 ) ) ;
#16391 = VECTOR ( 'NONE', #6331, 1000.000000000000000 ) ;
#16392 = VERTEX_POINT ( 'NONE', #318 ) ;
#16393 = B_SPLINE_CURVE_WITH_KNOTS ( 'NONE', 3,
 ( #15324, #28147, #19648, #26272, #28420, #3975 ),
 .UNSPECIFIED., .F., .F.,
 ( 4, 2, 4 ),
 ( 2.024876365526581719E-17, 0.0006311636237756984265, 0.001262327247551376687 ),
 .UNSPECIFIED. ) ;
#16394 = CONICAL_SURFACE ( 'NONE', #5561, 111.9614997405030152, 0.5880026024245678107 ) ;
#16395 = CARTESIAN_POINT ( 'NONE',  ( 2.263178607246687957, 28.85718361841115254, -142.5035407554792073 ) ) ;
#16396 = CARTESIAN_POINT ( 'NONE',  ( 10.93730112725977932, -115.5857507957709913, 97.44200844886238144 ) ) ;
#16397 = CARTESIAN_POINT ( 'NONE',  ( 32.73300124599739291, -3.836798148478013371, -117.5726003567929610 ) ) ;
#16398 =( BOUNDED_SURFACE ( )  B_SPLINE_SURFACE ( 3, 1, ( 
 ( #26207, #25945 ),
 ( #14986, #10686 ),
 ( #27048, #2896 ),
 ( #6935, #16275 ) ),
 .UNSPECIFIED., .F., .F., .F. ) 
 B_SPLINE_SURFACE_WITH_KNOTS ( ( 4, 4 ),
 ( 2, 2 ),
 ( 0.000000000000000000, 1.000000000000000000 ),
 ( 0.000000000000000000, 1.000000000000000000 ),
 .UNSPECIFIED. ) 
 GEOMETRIC_REPRESENTATION_ITEM ( )  RATIONAL_B_SPLINE_SURFACE ( (
 ( 1.000000000000000000, 1.000000000000000000),
 ( 0.7789835883360576307, 0.9689951854195403280),
 ( 0.7789835883360576307, 0.9689951854195403280),
 ( 1.000000000000000000, 1.000000000000000000) ) ) 
 REPRESENTATION_ITEM ( '' )  SURFACE ( )  );
#16399 = ORIENTED_EDGE ( 'NONE', *, *, #166, .F. ) ;
#16400 = VERTEX_POINT ( 'NONE', #13558 ) ;
#16401 = CARTESIAN_POINT ( 'NONE',  ( -1.045287976400383290, 28.14015102489806708, -36.12803364096618708 ) ) ;
#16402 = EDGE_CURVE ( 'NONE', #3497, #4240, #2891, .T. ) ;
#16403 = CARTESIAN_POINT ( 'NONE',  ( -10.86508079875812705, -45.04061326950857591, 24.22249093393325836 ) ) ;
#16404 = CARTESIAN_POINT ( 'NONE',  ( 109.1592201516379674, -0.002134489919774417484, -0.007566779963318545632 ) ) ;
#16405 = B_SPLINE_CURVE_WITH_KNOTS ( 'NONE', 3,
 ( #16213, #24737, #18085, #24870, #14050, #22421, #11902 ),
 .UNSPECIFIED., .F., .F.,
 ( 4, 3, 4 ),
 ( 0.000000000000000000, 0.02398743853561349781, 0.04000277880656220864 ),
 .UNSPECIFIED. ) ;
#16406 = CARTESIAN_POINT ( 'NONE',  ( 2.433796855181233454, 126.7346379669255754, 71.49415740225120430 ) ) ;
#16407 = CARTESIAN_POINT ( 'NONE',  ( -20.57838717382308147, 23.26537097894132344, 18.89542499756474569 ) ) ;
#16408 = ORIENTED_EDGE ( 'NONE', *, *, #11295, .T. ) ;
#16409 = CARTESIAN_POINT ( 'NONE',  ( 2.263178113027075611, -144.7392881653025256, 13.80342493153463579 ) ) ;
#16410 = B_SPLINE_CURVE_WITH_KNOTS ( 'NONE', 3,
 ( #14126, #322, #9111, #27052 ),
 .UNSPECIFIED., .F., .F.,
 ( 4, 4 ),
 ( 0.000000000000000000, 0.01077107196513872947 ),
 .UNSPECIFIED. ) ;
#16411 = B_SPLINE_CURVE_WITH_KNOTS ( 'NONE', 3,
 ( #15246, #2281, #4749, #22318 ),
 .UNSPECIFIED., .F., .F.,
 ( 4, 4 ),
 ( 1.904170172768910460E-16, 0.001982023823822945917 ),
 .UNSPECIFIED. ) ;
#16412 = CARTESIAN_POINT ( 'NONE',  ( -55.24271866751342941, -0.009369360294294061531, 0.001545935011626861600 ) ) ;
#16413 = CARTESIAN_POINT ( 'NONE',  ( 1.831572820252009626, 71.69925593429985611, -126.1609924456722354 ) ) ;
#16414 = VERTEX_POINT ( 'NONE', #6816 ) ;
#16415 = EDGE_CURVE ( 'NONE', #11326, #19279, #15711, .T. ) ;
#16416 = ORIENTED_EDGE ( 'NONE', *, *, #2844, .F. ) ;
#16417 = CARTESIAN_POINT ( 'NONE',  ( -55.25719721206881729, -0.01079965405819445674, 0.002847566758684036761 ) ) ;
#16418 = EDGE_CURVE ( 'NONE', #24434, #21106, #24871, .T. ) ;
#16419 = CARTESIAN_POINT ( 'NONE',  ( 32.73300124599731475, 117.5726003567930178, 3.836798148479249715 ) ) ;
#16420 = CARTESIAN_POINT ( 'NONE',  ( 32.73300124599738581, -72.21147546950486174, -92.86301839380092815 ) ) ;
#16421 = CARTESIAN_POINT ( 'NONE',  ( -1.048994561756786625, 13.42228657661184954, 43.78680886990926524 ) ) ;
#16422 = CARTESIAN_POINT ( 'NONE',  ( 1.833485406944057594, 141.8265699653871366, -30.69200235378795227 ) ) ;
#16423 = CARTESIAN_POINT ( 'NONE',  ( -1.259920593601971950, 2.243284667987781589, -45.95412615877140894 ) ) ;
#16424 = CARTESIAN_POINT ( 'NONE',  ( 109.1586900883932856, -0.006561743627145281976, -0.002810909342002382467 ) ) ;
#16425 = ORIENTED_EDGE ( 'NONE', *, *, #1562, .T. ) ;
#16426 = CARTESIAN_POINT ( 'NONE',  ( -55.24198130335446422, -0.001391250620104931938, 0.009190321388308853381 ) ) ;
#16427 = DIRECTION ( 'NONE',  ( -1.000000000000000000, -0.000000000000000000, -0.000000000000000000 ) ) ;
#16428 = CARTESIAN_POINT ( 'NONE',  ( -1.045287976400362417, -1.530335034934427574, -45.76855895860943235 ) ) ;
#16429 = EDGE_CURVE ( 'NONE', #10703, #14998, #17961, .T. ) ;
#16430 = CARTESIAN_POINT ( 'NONE',  ( 2.063896406836609909, -57.85593781835507343, 133.2511741302118651 ) ) ;
#16431 = CARTESIAN_POINT ( 'NONE',  ( -20.20700224038492721, 27.82980252387819675, -10.08426345511598932 ) ) ;
#16432 = EDGE_CURVE ( 'NONE', #1301, #17827, #15065, .T. ) ;
#16433 = EDGE_LOOP ( 'NONE', ( #4344, #9206, #9425, #7168 ) ) ;
#16434 = CARTESIAN_POINT ( 'NONE',  ( 25.64670758986457599, 22.98827151089287568, 110.5460908981863071 ) ) ;
#16435 = CARTESIAN_POINT ( 'NONE',  ( -24.53239521893646824, -30.86654523348673962, -14.09666242510777145 ) ) ;
#16436 = ORIENTED_EDGE ( 'NONE', *, *, #4413, .F. ) ;
#16437 = ORIENTED_EDGE ( 'NONE', *, *, #27725, .T. ) ;
#16438 = VERTEX_POINT ( 'NONE', #6188 ) ;
#16439 =( BOUNDED_SURFACE ( )  B_SPLINE_SURFACE ( 3, 1, ( 
 ( #7792, #18709 ),
 ( #12502, #5620 ),
 ( #7943, #27907 ),
 ( #12235, #27480 ) ),
 .UNSPECIFIED., .F., .F., .F. ) 
 B_SPLINE_SURFACE_WITH_KNOTS ( ( 4, 4 ),
 ( 2, 2 ),
 ( 0.000000000000000000, 1.000000000000000000 ),
 ( 0.000000000000000000, 1.000000000000000000 ),
 .UNSPECIFIED. ) 
 GEOMETRIC_REPRESENTATION_ITEM ( )  RATIONAL_B_SPLINE_SURFACE ( (
 ( 1.000000000000000000, 1.000000000000000000),
 ( 0.9960225298536222738, 0.9999952330161893110),
 ( 0.9960225298536222738, 0.9999952330161893110),
 ( 1.000000000000000000, 1.000000000000000000) ) ) 
 REPRESENTATION_ITEM ( '' )  SURFACE ( )  );
#16440 = CARTESIAN_POINT ( 'NONE',  ( -55.24390624410018802, 0.01032895241566708991, 0.001451500391952845713 ) ) ;
#16441 = CARTESIAN_POINT ( 'NONE',  ( 2.433796855181205476, -138.8296532063090751, 43.58222566461595449 ) ) ;
#16442 = CARTESIAN_POINT ( 'NONE',  ( 109.1592201516379674, 0.007748443302128555504, -0.001331853079208340871 ) ) ;
#16443 = B_SPLINE_CURVE_WITH_KNOTS ( 'NONE', 3,
 ( #18294, #9410, #11843, #9986, #11703, #13991, #5067, #7252 ),
 .UNSPECIFIED., .F., .F.,
 ( 4, 2, 2, 4 ),
 ( 0.000000000000000000, 0.0002429588503611235717, 0.0004859177007222471433, 0.0009718354014444888656 ),
 .UNSPECIFIED. ) ;
#16444 = CARTESIAN_POINT ( 'NONE',  ( 2.108393763691192024, -98.16799842733318826, 107.1124103264145901 ) ) ;
#16445 = CARTESIAN_POINT ( 'NONE',  ( 2.430230287190581429, 142.6294793592101655, -28.83279105684287913 ) ) ;
#16446 = CARTESIAN_POINT ( 'NONE',  ( -20.21097721712959583, 24.14932359587290023, -17.13687106192352161 ) ) ;
#16447 = CARTESIAN_POINT ( 'NONE',  ( -1.045287976400365970, 45.76855895860943235, -1.530335034934267258 ) ) ;
#16448 = EDGE_CURVE ( 'NONE', #213, #19162, #23507, .T. ) ;
#16449 = CARTESIAN_POINT ( 'NONE',  ( -20.20612092514784308, -27.77903665678158873, 10.22177639105890279 ) ) ;
#16450 = CARTESIAN_POINT ( 'NONE',  ( -20.21097721650787449, -28.05863614620931656, 9.464413208035370673 ) ) ;
#16451 = CARTESIAN_POINT ( 'NONE',  ( 55.49584447822657296, -72.12568090333337523, -7.849835876629073006 ) ) ;
#16452 = ADVANCED_FACE ( 'NONE', ( #23888 ), #14449, .F. ) ;
#16453 = CARTESIAN_POINT ( 'NONE',  ( 6.224689322667647851, -12.92299475787058860, 147.4941644018827844 ) ) ;
#16454 = CARTESIAN_POINT ( 'NONE',  ( 55.79472521941426777, 37.00555938668347977, -62.63970324008221979 ) ) ;
#16455 = CARTESIAN_POINT ( 'NONE',  ( 26.11404676487259024, -22.43340081644844020, 110.9778746459746372 ) ) ;
#16456 = CARTESIAN_POINT ( 'NONE',  ( -1.044556982611274831, 36.05793013899099719, -28.22896456560681600 ) ) ;
#16457 = VERTEX_POINT ( 'NONE', #3873 ) ;
#16458 = FACE_OUTER_BOUND ( 'NONE', #12717, .T. ) ;
#16459 = ORIENTED_EDGE ( 'NONE', *, *, #2691, .F. ) ;
#16460 = CARTESIAN_POINT ( 'NONE',  ( -55.24300891470648622, -0.002702093572889207890, -0.009439835024157681651 ) ) ;
#16461 = DIRECTION ( 'NONE',  ( 1.000000000000000000, -6.938893903907226837E-18, 1.734723475976806709E-18 ) ) ;
#16462 = B_SPLINE_CURVE_WITH_KNOTS ( 'NONE', 3,
 ( #27782, #5771, #18712, #27909 ),
 .UNSPECIFIED., .F., .F.,
 ( 4, 4 ),
 ( 3.481441887456309019E-16, 0.01077107486149842842 ),
 .UNSPECIFIED. ) ;
#16463 = EDGE_LOOP ( 'NONE', ( #1141, #21805, #15658, #8666 ) ) ;
#16464 = ORIENTED_EDGE ( 'NONE', *, *, #2042, .F. ) ;
#16465 = VERTEX_POINT ( 'NONE', #23755 ) ;
#16466 = CARTESIAN_POINT ( 'NONE',  ( 32.73300124599732186, 0.000000000000000000, 0.000000000000000000 ) ) ;
#16467 = CARTESIAN_POINT ( 'NONE',  ( 1.893872463202064260, 86.08597552419035992, -116.8661275359689427 ) ) ;
#16468 = CARTESIAN_POINT ( 'NONE',  ( 109.1587776205901861, -0.001605238040368415576, -0.007151389024635748486 ) ) ;
#16469 = AXIS2_PLACEMENT_3D ( 'NONE', #8790, #4597, #4891 ) ;
#16470 =( BOUNDED_SURFACE ( )  B_SPLINE_SURFACE ( 3, 1, ( 
 ( #8383, #26200 ),
 ( #21750, #22170 ),
 ( #23795, #17415 ),
 ( #15526, #10948 ) ),
 .UNSPECIFIED., .F., .F., .F. ) 
 B_SPLINE_SURFACE_WITH_KNOTS ( ( 4, 4 ),
 ( 2, 2 ),
 ( 0.000000000000000000, 1.000000000000000000 ),
 ( 0.000000000000000000, 1.000000000000000000 ),
 .UNSPECIFIED. ) 
 GEOMETRIC_REPRESENTATION_ITEM ( )  RATIONAL_B_SPLINE_SURFACE ( (
 ( 1.000000000000000000, 1.000000000000000000),
 ( 0.7789835883360578528, 0.9689951854195403280),
 ( 0.7789835883360578528, 0.9689951854195403280),
 ( 1.000000000000000000, 1.000000000000000000) ) ) 
 REPRESENTATION_ITEM ( '' )  SURFACE ( )  );
#16471 = CARTESIAN_POINT ( 'NONE',  ( -55.24271866751342941, -0.006671293903668846365, 0.006757859501006202411 ) ) ;
#16472 = DIRECTION ( 'NONE',  ( 0.7637818620346800147, -0.3965875333584803486, 0.5092696688508683289 ) ) ;
#16473 = CARTESIAN_POINT ( 'NONE',  ( -1.583189561560255143, 16.68617981233701997, -43.29471907393748609 ) ) ;
#16474 = CARTESIAN_POINT ( 'NONE',  ( -1.113427685306993320, 25.34053733836532274, -38.22586258295203265 ) ) ;
#16475 = EDGE_CURVE ( 'NONE', #10330, #21420, #26161, .T. ) ;
#16476 = FACE_OUTER_BOUND ( 'NONE', #22546, .T. ) ;
#16477 = CARTESIAN_POINT ( 'NONE',  ( 109.1587776205901861, 0.006944419901758130259, -0.002343968083398764550 ) ) ;
#16478 = CARTESIAN_POINT ( 'NONE',  ( -20.21097721712959583, -17.67178718142840665, 23.76068428613700334 ) ) ;
#16480 = EDGE_LOOP ( 'NONE', ( #2434, #2069, #917, #606 ) ) ;
#16479 = EDGE_CURVE ( 'NONE', #709, #18117, #28250, .T. ) ;
#16481 = VERTEX_POINT ( 'NONE', #6048 ) ;
#16482 = DIRECTION ( 'NONE',  ( -1.000000000000000000, -0.000000000000000000, -0.000000000000000000 ) ) ;
#16484 = CARTESIAN_POINT ( 'NONE',  ( 25.64670758986456889, 75.92149922855311672, -83.57526425215419863 ) ) ;
#16483 = CARTESIAN_POINT ( 'NONE',  ( 1.833838850855486147, 85.22139087169075822, 117.4485666028820958 ) ) ;
#16485 = EDGE_CURVE ( 'NONE', #22401, #15242, #3913, .T. ) ;
#16486 = CARTESIAN_POINT ( 'NONE',  ( 2.433796855181219243, -28.83182736670634583, 142.6247129145647534 ) ) ;
#16487 = ORIENTED_EDGE ( 'NONE', *, *, #11300, .T. ) ;
#16488 = EDGE_LOOP ( 'NONE', ( #23734, #1603, #18376, #24401 ) ) ;
#16489 = CARTESIAN_POINT ( 'NONE',  ( -4.780792508754313275, -25.98388465890110410, -42.16805077400949386 ) ) ;
#16490 = CARTESIAN_POINT ( 'NONE',  ( 25.64660436782551400, -35.44263474731867092, -107.2041192742819078 ) ) ;
#16491 = CARTESIAN_POINT ( 'NONE',  ( 30.59138290137920890, 115.2623146671594441, -14.83088430729453400 ) ) ;
#16492 = VERTEX_POINT ( 'NONE', #8747 ) ;
#16493 = FACE_OUTER_BOUND ( 'NONE', #16512, .T. ) ;
#16494 = DIRECTION ( 'NONE',  ( -0.7563875759206388771, 0.6104009704506910827, -0.2351350468682930628 ) ) ;
#16495 = CIRCLE ( 'NONE', #10531, 53.53553390275978785 ) ;
#16496 = VERTEX_POINT ( 'NONE', #6597 ) ;
#16497 = CIRCLE ( 'NONE', #9138, 34.60786435723138510 ) ;
#16498 = VERTEX_POINT ( 'NONE', #12774 ) ;
#16499 = CARTESIAN_POINT ( 'NONE',  ( 2.433796855181205476, 138.8296532063094162, -43.58222566461498815 ) ) ;
#16500 = ORIENTED_EDGE ( 'NONE', *, *, #716, .F. ) ;
#16501 = CARTESIAN_POINT ( 'NONE',  ( -1.044557008772712070, -43.01636061108997922, -15.70482370518800153 ) ) ;
#16502 = CARTESIAN_POINT ( 'NONE',  ( 2.430230287190589422, 28.83279105684624000, -142.6294793592095118 ) ) ;
#16503 = ORIENTED_EDGE ( 'NONE', *, *, #5422, .T. ) ;
#16504 = APPLICATION_PROTOCOL_DEFINITION ( 'draft international standard', 'automotive_design', 1998, #5692 ) ;
#16505 = EDGE_CURVE ( 'NONE', #7217, #13496, #11518, .T. ) ;
#16506 = CARTESIAN_POINT ( 'NONE',  ( 28.37603512858453669, 100.2461737936630612, 55.80522682147307734 ) ) ;
#16507 =( BOUNDED_SURFACE ( )  B_SPLINE_SURFACE ( 3, 1, ( 
 ( #982, #7623 ),
 ( #25040, #27163 ),
 ( #23305, #20843 ),
 ( #18972, #16233 ) ),
 .UNSPECIFIED., .F., .F., .F. ) 
 B_SPLINE_SURFACE_WITH_KNOTS ( ( 4, 4 ),
 ( 2, 2 ),
 ( 0.000000000000000000, 1.000000000000000000 ),
 ( 0.000000000000000000, 1.000000000000000000 ),
 .UNSPECIFIED. ) 
 GEOMETRIC_REPRESENTATION_ITEM ( )  RATIONAL_B_SPLINE_SURFACE ( (
 ( 1.000000000000000000, 1.000000000000000000),
 ( 0.9956975270656955868, 0.8568959468854907557),
 ( 0.9956975270656955868, 0.8568959468854907557),
 ( 1.000000000000000000, 1.000000000000000000) ) ) 
 REPRESENTATION_ITEM ( '' )  SURFACE ( )  );
#16508 = CARTESIAN_POINT ( 'NONE',  ( 1.894214914920971937, -117.9869255019025900, -84.54370816135696032 ) ) ;
#16509 = CARTESIAN_POINT ( 'NONE',  ( 25.64670758986458310, -46.37945960491945385, 102.9458331681483685 ) ) ;
#16510 = CARTESIAN_POINT ( 'NONE',  ( 28.37644542392825997, 116.9383271603247891, 42.25924161793936662 ) ) ;
#16511 = EDGE_CURVE ( 'NONE', #20724, #21385, #26226, .T. ) ;
#16512 = EDGE_LOOP ( 'NONE', ( #28324, #26425, #24346, #25255 ) ) ;
#16513 = B_SPLINE_CURVE_WITH_KNOTS ( 'NONE', 3,
 ( #23181, #21411, #16683, #23313, #25477, #5751, #28159 ),
 .UNSPECIFIED., .F., .F.,
 ( 4, 3, 4 ),
 ( 0.000000000000000000, 0.02398743853561352210, 0.04000277880656218088 ),
 .UNSPECIFIED. ) ;
#16514 = CARTESIAN_POINT ( 'NONE',  ( -1.049817751779889008, -14.63752841325019105, 43.39729912094394848 ) ) ;
#16515 = LINE ( 'NONE', #25302, #9309 ) ;
#16516 = CARTESIAN_POINT ( 'NONE',  ( -20.24419206586951603, 23.20105925399726132, -18.44224248888881590 ) ) ;
#16517 = ORIENTED_EDGE ( 'NONE', *, *, #1389, .T. ) ;
#16518 = ORIENTED_EDGE ( 'NONE', *, *, #3934, .F. ) ;
#16519 = ORIENTED_EDGE ( 'NONE', *, *, #25015, .F. ) ;
#16520 = CARTESIAN_POINT ( 'NONE',  ( -1.019300379054419725, -2.023851374322995778, -45.76814864815089123 ) ) ;
#16521 = CARTESIAN_POINT ( 'NONE',  ( 2.433796855181233454, 60.50726454507903895, 132.3327394885233446 ) ) ;
#16523 = CARTESIAN_POINT ( 'NONE',  ( 13.84597867724970044, -135.8932891738221542, 55.26821062125512896 ) ) ;
#16522 = CARTESIAN_POINT ( 'NONE',  ( 9.884929003653626367, -78.87917189084822667, -128.2151425008049728 ) ) ;
#16524 = CARTESIAN_POINT ( 'NONE',  ( 2.108985857320903712, 133.2480631238193496, 57.92316197981703851 ) ) ;
#16525 = CARTESIAN_POINT ( 'NONE',  ( 1.831572820252009626, -126.1609924456724912, -71.69925593429942978 ) ) ;
#16526 = EDGE_LOOP ( 'NONE', ( #15552, #20667, #4852, #16923 ) ) ;
#16527 = CARTESIAN_POINT ( 'NONE',  ( 25.64708010899965629, -83.87281825978668337, 75.59303792846597503 ) ) ;
#16528 = CARTESIAN_POINT ( 'NONE',  ( 24.22246935314087324, 0.000000000000000000, 0.000000000000000000 ) ) ;
#16529 = ORIENTED_EDGE ( 'NONE', *, *, #12316, .T. ) ;
#16530 = CARTESIAN_POINT ( 'NONE',  ( 2.433796855181219243, 133.5135467655526043, -57.85512797797757401 ) ) ;
#16531 = CARTESIAN_POINT ( 'NONE',  ( -1.050229599974477734, 14.39582765040461254, -43.47850826583058392 ) ) ;
#16532 = CARTESIAN_POINT ( 'NONE',  ( 9.884929003653626367, 97.56484214660780196, -114.6392083957107815 ) ) ;
#16533 = CARTESIAN_POINT ( 'NONE',  ( -55.25297051322618813, -0.007247191603128547155, 0.01306918787467270006 ) ) ;
#16534 = CARTESIAN_POINT ( 'NONE',  ( -20.20700224038492010, 24.51628800869071867, 16.58740185276683832 ) ) ;
#16535 = CARTESIAN_POINT ( 'NONE',  ( 2.430230287190592531, -133.5180086894987710, -57.85706160874279647 ) ) ;
#16536 = VERTEX_POINT ( 'NONE', #6316 ) ;
#16537 = CARTESIAN_POINT ( 'NONE',  ( 32.73300124599732186, 0.000000000000000000, 0.000000000000000000 ) ) ;
#16538 = CARTESIAN_POINT ( 'NONE',  ( 1.833485406944057594, -30.69200235378832176, -141.8265699653870513 ) ) ;
#16539 = CARTESIAN_POINT ( 'NONE',  ( 32.73300124599736449, -116.5274707358856574, 16.10546300444784507 ) ) ;
#16540 = ORIENTED_EDGE ( 'NONE', *, *, #5300, .F. ) ;
#16541 = CARTESIAN_POINT ( 'NONE',  ( -1.058473599757816963, 25.48501014712399737, -38.06357893967437889 ) ) ;
#16542 = ORIENTED_EDGE ( 'NONE', *, *, #24663, .T. ) ;
#16543 = CARTESIAN_POINT ( 'NONE',  ( -1.031422197589716205, 28.14735071801744581, -36.13727897780137965 ) ) ;
#16544 = EDGE_CURVE ( 'NONE', #9793, #2416, #11327, .T. ) ;
#16545 = EDGE_CURVE ( 'NONE', #5021, #24828, #382, .T. ) ;
#16546 = CARTESIAN_POINT ( 'NONE',  ( 32.73300124599740002, 110.6325518752278896, -39.98094346392192477 ) ) ;
#16547 = B_SPLINE_CURVE_WITH_KNOTS ( 'NONE', 3,
 ( #23006, #8166, #27439, #7749 ),
 .UNSPECIFIED., .F., .F.,
 ( 4, 4 ),
 ( 0.000000000000000000, 0.008383560773332738095 ),
 .UNSPECIFIED. ) ;
#16548 = CARTESIAN_POINT ( 'NONE',  ( 21.16825799904901473, 63.85626241912904533, -119.4343305756972597 ) ) ;
#16549 = ORIENTED_EDGE ( 'NONE', *, *, #13129, .T. ) ;
#16550 = FACE_OUTER_BOUND ( 'NONE', #6268, .T. ) ;
#16551 = EDGE_CURVE ( 'NONE', #22112, #17196, #4167, .T. ) ;
#16552 = CARTESIAN_POINT ( 'NONE',  ( -9.156249394959713683, 53.90509764945130655, -8.027840202794127578 ) ) ;
#16553 = CARTESIAN_POINT ( 'NONE',  ( 2.063896406836609909, 71.46753739786191773, -126.4736179849640365 ) ) ;
#16554 = ORIENTED_EDGE ( 'NONE', *, *, #10235, .F. ) ;
#16555 = EDGE_LOOP ( 'NONE', ( #17793, #4590, #19577, #6537 ) ) ;
#16556 = CARTESIAN_POINT ( 'NONE',  ( -1.046935749539996685, -43.14401153755477480, -15.35946454248379034 ) ) ;
#16557 = B_SPLINE_CURVE_WITH_KNOTS ( 'NONE', 3,
 ( #5621, #6055, #12366, #23196, #21001, #14810, #1286, #3587, #12236, #14940 ),
 .UNSPECIFIED., .F., .F.,
 ( 4, 3, 3, 4 ),
 ( 3.469446951953614189E-17, 0.0002669559177086236468, 0.0005339118354151006817, 0.001067817517169172489 ),
 .UNSPECIFIED. ) ;
#16558 = CARTESIAN_POINT ( 'NONE',  ( 32.73300124599736449, -66.00340565729409548, 97.37344512919831629 ) ) ;
#16559 = CARTESIAN_POINT ( 'NONE',  ( 109.1586900883932856, -0.006960773163852201732, 0.001582822706032804708 ) ) ;
#16560 = AXIS2_PLACEMENT_3D ( 'NONE', #19504, #17333, #6413 ) ;
#16561 = CARTESIAN_POINT ( 'NONE',  ( 26.11404676487257603, -102.9690087468804762, 47.08215554553482463 ) ) ;
#16562 = CARTESIAN_POINT ( 'NONE',  ( -8.786685647604898008, 38.68584556812353981, 37.00619870957891777 ) ) ;
#16563 = CARTESIAN_POINT ( 'NONE',  ( -1.619063947482197729, 46.30105812165548684, -2.489035965910316506 ) ) ;
#16564 = CARTESIAN_POINT ( 'NONE',  ( -25.21435515916043002, 30.48034229288640162, -16.39063784838753790 ) ) ;
#16565 = ORIENTED_EDGE ( 'NONE', *, *, #748, .F. ) ;
#16566 = DIRECTION ( 'NONE',  ( 0.000000000000000000, 0.000000000000000000, 1.000000000000000000 ) ) ;
#16567 = CARTESIAN_POINT ( 'NONE',  ( -8.786685647604887350, -38.68584556812326980, -37.00619870957918778 ) ) ;
#16568 = CARTESIAN_POINT ( 'NONE',  ( -20.47566262905010248, -23.19796652405687709, -18.81547655725238499 ) ) ;
#16569 = B_SPLINE_CURVE_WITH_KNOTS ( 'NONE', 3,
 ( #12865, #13294, #1930, #23982, #4668, #6275, #15026, #28402, #6551, #26537 ),
 .UNSPECIFIED., .F., .F.,
 ( 4, 2, 2, 2, 4 ),
 ( 2.913600445039318278E-16, 0.0003346187017559116412, 0.0006692374035115318488, 0.001003856105267152219, 0.001338474807022772481 ),
 .UNSPECIFIED. ) ;
#16570 = CARTESIAN_POINT ( 'NONE',  ( -20.24399999263414429, -16.36687688782875938, -24.70869149526196651 ) ) ;
#16571 =( BOUNDED_SURFACE ( )  B_SPLINE_SURFACE ( 3, 1, ( 
 ( #17278, #14565 ),
 ( #3622, #12398 ),
 ( #12543, #23798 ),
 ( #12960, #23659 ) ),
 .UNSPECIFIED., .F., .F., .F. ) 
 B_SPLINE_SURFACE_WITH_KNOTS ( ( 4, 4 ),
 ( 2, 2 ),
 ( 0.000000000000000000, 1.000000000000000000 ),
 ( 0.000000000000000000, 1.000000000000000000 ),
 .UNSPECIFIED. ) 
 GEOMETRIC_REPRESENTATION_ITEM ( )  RATIONAL_B_SPLINE_SURFACE ( (
 ( 1.000000000000000000, 1.000000000000000000),
 ( 0.6386103224230302855, 0.9954351624131538845),
 ( 0.6386103224230302855, 0.9954351624131538845),
 ( 1.000000000000000000, 1.000000000000000000) ) ) 
 REPRESENTATION_ITEM ( '' )  SURFACE ( )  );
#16572 = VERTEX_POINT ( 'NONE', #24440 ) ;
#16573 = CARTESIAN_POINT ( 'NONE',  ( 25.64692872815578184, -75.79105864157443762, 83.69378511050537384 ) ) ;
#16574 = CARTESIAN_POINT ( 'NONE',  ( 24.01988960052043609, 115.5642432877701822, -61.78678588189911380 ) ) ;
#16575 = ORIENTED_EDGE ( 'NONE', *, *, #4600, .T. ) ;
#16576 = ORIENTED_EDGE ( 'NONE', *, *, #10741, .T. ) ;
#16577 = ORIENTED_EDGE ( 'NONE', *, *, #22975, .T. ) ;
#16578 = EDGE_CURVE ( 'NONE', #21771, #5523, #13840, .T. ) ;
#16579 = CIRCLE ( 'NONE', #10591, 34.60786435723138510 ) ;
#16580 = AXIS2_PLACEMENT_3D ( 'NONE', #2114, #8614, #1838 ) ;
#16581 = CARTESIAN_POINT ( 'NONE',  ( 25.64681081121879203, -110.3564950173080206, -23.88203588908195130 ) ) ;
#16582 = CARTESIAN_POINT ( 'NONE',  ( -55.25719721206881729, -0.01079965405819445674, 0.002847566758684036761 ) ) ;
#16583 = AXIS2_PLACEMENT_3D ( 'NONE', #17377, #28447, #28314 ) ;
#16584 = EDGE_CURVE ( 'NONE', #7936, #3978, #15928, .T. ) ;
#16585 = CARTESIAN_POINT ( 'NONE',  ( 109.1592201516379674, 0.0005146241775982810093, 0.007845213074654433863 ) ) ;
#16586 = CARTESIAN_POINT ( 'NONE',  ( 55.79472521941428198, -21.78881894124752350, 69.41463258328505503 ) ) ;
#16587 = EDGE_CURVE ( 'NONE', #12739, #16046, #27101, .T. ) ;
#16588 = CARTESIAN_POINT ( 'NONE',  ( -25.21435515916043713, -34.05351380035337883, -6.169479169075319014 ) ) ;
#16589 = ORIENTED_EDGE ( 'NONE', *, *, #5871, .T. ) ;
#16590 = LINE ( 'NONE', #9681, #17552 ) ;
#16591 = CARTESIAN_POINT ( 'NONE',  ( 25.64699802086722968, 84.06830990999330311, 75.37548011155753613 ) ) ;
#16592 = CARTESIAN_POINT ( 'NONE',  ( -8.786685647604890903, 25.35688121747502066, -47.14957014837363403 ) ) ;
#16593 = LINE ( 'NONE', #23238, #569 ) ;
#16594 = CARTESIAN_POINT ( 'NONE',  ( 25.87036335909427009, -110.3794299719621677, 24.47383578007097782 ) ) ;
#16595 = CARTESIAN_POINT ( 'NONE',  ( 32.73300124599739291, -103.7392577722171865, -55.46353551262117776 ) ) ;
#16596 = CIRCLE ( 'NONE', #8788, 117.6351876552689504 ) ;
#16597 = VECTOR ( 'NONE', #22304, 1000.000000000000000 ) ;
#16598 = CARTESIAN_POINT ( 'NONE',  ( 26.28373643307413232, -22.43832507403739385, 125.5716026420346196 ) ) ;
#16599 = AXIS2_PLACEMENT_3D ( 'NONE', #15983, #13536, #22335 ) ;
#16600 = CARTESIAN_POINT ( 'NONE',  ( -1.583189561560253589, -25.21827308671203127, 38.94740041318322454 ) ) ;
#16601 = CARTESIAN_POINT ( 'NONE',  ( 26.11404676487257603, -84.89295829319543429, 74.91683232330944975 ) ) ;
#16602 = CARTESIAN_POINT ( 'NONE',  ( -9.156249394959713683, 9.022661520477768704, -53.74753343182706544 ) ) ;
#16603 = CARTESIAN_POINT ( 'NONE',  ( -2.911734481061402757, -25.69892591260238746, 40.13920818157105685 ) ) ;
#16604 = ORIENTED_EDGE ( 'NONE', *, *, #12995, .F. ) ;
#16605 = DIRECTION ( 'NONE',  ( -0.5914120900931443270, -0.5455001977188012052, -0.5938529060132713422 ) ) ;
#16607 = VECTOR ( 'NONE', #6322, 1000.000000000000000 ) ;
#16606 =( BOUNDED_SURFACE ( )  B_SPLINE_SURFACE ( 3, 1, ( 
 ( #11856, #11565 ),
 ( #911, #9696 ),
 ( #334, #18174 ),
 ( #22519, #2491 ) ),
 .UNSPECIFIED., .F., .F., .F. ) 
 B_SPLINE_SURFACE_WITH_KNOTS ( ( 4, 4 ),
 ( 2, 2 ),
 ( 0.000000000000000000, 1.000000000000000000 ),
 ( 0.000000000000000000, 1.000000000000000000 ),
 .UNSPECIFIED. ) 
 GEOMETRIC_REPRESENTATION_ITEM ( )  RATIONAL_B_SPLINE_SURFACE ( (
 ( 1.000000000000000000, 1.000000000000000000),
 ( 0.6386103224230316178, 0.9954351624131538845),
 ( 0.6386103224230316178, 0.9954351624131538845),
 ( 1.000000000000000000, 1.000000000000000000) ) ) 
 REPRESENTATION_ITEM ( '' )  SURFACE ( )  );
#16608 = VERTEX_POINT ( 'NONE', #16177 ) ;
#16609 = CARTESIAN_POINT ( 'NONE',  ( 2.263178607246653318, -16.59120332983045998, -144.4462811785178076 ) ) ;
#16610 = CARTESIAN_POINT ( 'NONE',  ( 94.22246935314088034, 90.00000000000005684, -12.50000000000000888 ) ) ;
#16611 = ORIENTED_EDGE ( 'NONE', *, *, #2942, .F. ) ;
#16612 = B_SPLINE_CURVE_WITH_KNOTS ( 'NONE', 3,
 ( #15048, #26008, #23870, #1956, #10761, #9149, #24006 ),
 .UNSPECIFIED., .F., .F.,
 ( 4, 3, 4 ),
 ( 3.469446951953614189E-18, 0.009512539173626381045, 0.02506242213020843518 ),
 .UNSPECIFIED. ) ;
#16613 = ORIENTED_EDGE ( 'NONE', *, *, #14722, .F. ) ;
#16614 = ORIENTED_EDGE ( 'NONE', *, *, #22034, .T. ) ;
#16615 = ADVANCED_FACE ( 'NONE', ( #24984 ), #17384, .F. ) ;
#16616 = EDGE_CURVE ( 'NONE', #23443, #20437, #27253, .T. ) ;
#16617 = EDGE_CURVE ( 'NONE', #11082, #21644, #14561, .T. ) ;
#16618 = B_SPLINE_CURVE_WITH_KNOTS ( 'NONE', 3,
 ( #19571, #26468, #2273, #4447 ),
 .UNSPECIFIED., .F., .F.,
 ( 4, 4 ),
 ( 0.000000000000000000, 0.008383560773332720747 ),
 .UNSPECIFIED. ) ;
#16619 = VECTOR ( 'NONE', #27795, 1000.000000000000000 ) ;
#16620 = CARTESIAN_POINT ( 'NONE',  ( -16.86833981943424376, -30.57013526701942041, -31.95666732167553548 ) ) ;
#16621 = EDGE_CURVE ( 'NONE', #25689, #22240, #4248, .T. ) ;
#16622 = CONICAL_SURFACE ( 'NONE', #13856, 117.6351876552689504, 0.9945805576725580410 ) ;
#16623 = CARTESIAN_POINT ( 'NONE',  ( -8.786685647604890903, -48.22796981442785835, -23.24040270374372952 ) ) ;
#16624 = CARTESIAN_POINT ( 'NONE',  ( -1.259972190295307604, -2.243354636026084759, -45.95417440459613800 ) ) ;
#16625 = CARTESIAN_POINT ( 'NONE',  ( -1.045287976400383290, 28.14015102489806708, -36.12803364096618708 ) ) ;
#16626 = CARTESIAN_POINT ( 'NONE',  ( -1.048172774974290622, -15.11899685083854727, -43.23017713506519755 ) ) ;
#16627 = DIRECTION ( 'NONE',  ( -0.5946245182733607137, -0.7637359336799420806, 0.2512550613902148622 ) ) ;
#16628 = ORIENTED_EDGE ( 'NONE', *, *, #19568, .F. ) ;
#16629 = EDGE_LOOP ( 'NONE', ( #12102, #25068, #5564, #4632 ) ) ;
#16630 = CARTESIAN_POINT ( 'NONE',  ( 2.063896406836605024, 1.344106060022389526, -145.2631347824382431 ) ) ;
#16632 = CARTESIAN_POINT ( 'NONE',  ( -1.539763995773685945, 25.17088606276602647, 38.84665165401036546 ) ) ;
#16631 = CARTESIAN_POINT ( 'NONE',  ( 109.1586900883932856, 0.002810909342011597319, 0.006561743627143340821 ) ) ;
#16633 = CARTESIAN_POINT ( 'NONE',  ( -20.20612091757416451, -8.058516044219402374, -28.48192249925589792 ) ) ;
#16634 = CARTESIAN_POINT ( 'NONE',  ( -25.21435515916043002, 30.48034229288640162, -16.39063784838753790 ) ) ;
#16635 = VERTEX_POINT ( 'NONE', #27966 ) ;
#16636 = VERTEX_POINT ( 'NONE', #19195 ) ;
#16637 = CARTESIAN_POINT ( 'NONE',  ( -6.588769196390752647, -26.02756986588571309, -44.25609997968896892 ) ) ;
#16638 = CARTESIAN_POINT ( 'NONE',  ( 1.831572820252008738, 144.2101521542830369, 16.14965423926257770 ) ) ;
#16639 = B_SPLINE_CURVE_WITH_KNOTS ( 'NONE', 3,
 ( #11396, #17582, #180, #21917 ),
 .UNSPECIFIED., .F., .F.,
 ( 4, 4 ),
 ( 0.000000000000000000, 0.008383560773332715543 ),
 .UNSPECIFIED. ) ;
#16640 = CARTESIAN_POINT ( 'NONE',  ( 24.01988960052061373, -127.2243989116373371, -31.41104197353454452 ) ) ;
#16641 = ORIENTED_EDGE ( 'NONE', *, *, #13874, .F. ) ;
#16642 = DIRECTION ( 'NONE',  ( 1.000000000000000000, -6.938893903907226837E-18, 1.734723475976806709E-18 ) ) ;
#16643 = CARTESIAN_POINT ( 'NONE',  ( -20.57838717382308147, -29.92853265176832878, -1.611677988432255848 ) ) ;
#16644 = ORIENTED_EDGE ( 'NONE', *, *, #19326, .F. ) ;
#16645 = AXIS2_PLACEMENT_3D ( 'NONE', #2786, #25106, #13717 ) ;
#16646 = VERTEX_POINT ( 'NONE', #6248 ) ;
#16647 = EDGE_CURVE ( 'NONE', #10945, #26104, #12423, .T. ) ;
#16648 =( BOUNDED_SURFACE ( )  B_SPLINE_SURFACE ( 3, 1, ( 
 ( #24570, #11584 ),
 ( #7422, #13304 ),
 ( #2961, #7147 ),
 ( #647, #7001 ) ),
 .UNSPECIFIED., .F., .F., .F. ) 
 B_SPLINE_SURFACE_WITH_KNOTS ( ( 4, 4 ),
 ( 2, 2 ),
 ( 0.000000000000000000, 1.000000000000000000 ),
 ( 0.000000000000000000, 1.000000000000000000 ),
 .UNSPECIFIED. ) 
 GEOMETRIC_REPRESENTATION_ITEM ( )  RATIONAL_B_SPLINE_SURFACE ( (
 ( 1.000000000000000000, 1.000000000000000000),
 ( 0.9934239774497837239, 0.8357310067453919133),
 ( 0.9934239774497837239, 0.8357310067453919133),
 ( 1.000000000000000000, 1.000000000000000000) ) ) 
 REPRESENTATION_ITEM ( '' )  SURFACE ( )  );
#16649 = CARTESIAN_POINT ( 'NONE',  ( 10.93730112726003156, 119.3442956573285443, -92.80059208661575099 ) ) ;
#16650 = VERTEX_POINT ( 'NONE', #7853 ) ;
#16651 = PRODUCT ( 'MAT-025', 'MAT-025', '', ( #16655 ) ) ;
#16652 = ADVANCED_FACE ( 'NONE', ( #14724 ), #15360, .F. ) ;
#16653 = CARTESIAN_POINT ( 'NONE',  ( 109.1586059443104944, 0.006971743774738786009, -0.001198897580748364746 ) ) ;
#16654 = CARTESIAN_POINT ( 'NONE',  ( -25.21435515916043713, 30.48034229288662544, 16.39063784838709736 ) ) ;
#16655 = PRODUCT_CONTEXT ( 'NONE', #9950, 'mechanical' ) ;
#16657 = AXIS2_PLACEMENT_3D ( 'NONE', #4037, #23919, #27805 ) ;
#16656 = CARTESIAN_POINT ( 'NONE',  ( -7.078251931573400491, 34.59014398252916322, -38.93060825814240644 ) ) ;
#16658 = B_SPLINE_CURVE_WITH_KNOTS ( 'NONE', 3,
 ( #25017, #12045, #22715, #22857 ),
 .UNSPECIFIED., .F., .F.,
 ( 4, 4 ),
 ( 3.469446951953614189E-18, 0.008383560773332732891 ),
 .UNSPECIFIED. ) ;
#16659 = DIRECTION ( 'NONE',  ( 0.000000000000000000, 5.223019709707975211E-21, -1.000000000000000000 ) ) ;
#16660 = CARTESIAN_POINT ( 'NONE',  ( 2.063896406836605024, 141.8093313989361093, 31.51663808384605403 ) ) ;
#16661 = CARTESIAN_POINT ( 'NONE',  ( 1.833809397773843219, -107.7184108265657443, -97.22957127128945842 ) ) ;
#16662 = ORIENTED_EDGE ( 'NONE', *, *, #24916, .T. ) ;
#16663 = AXIS2_PLACEMENT_3D ( 'NONE', #23405, #10443, #16785 ) ;
#16664 = CARTESIAN_POINT ( 'NONE',  ( 21.16825799904903960, -4.416019842157457909, -135.3612955721066839 ) ) ;
#16666 = FACE_OUTER_BOUND ( 'NONE', #1394, .T. ) ;
#16665 = CARTESIAN_POINT ( 'NONE',  ( -1.583189561560255143, 38.94740041318295454, -25.21827308671246470 ) ) ;
#16667 = CARTESIAN_POINT ( 'NONE',  ( -20.20700224038492721, 23.35150625415659320, -18.19058640100232438 ) ) ;
#16668 = ORIENTED_EDGE ( 'NONE', *, *, #15962, .T. ) ;
#16669 = VECTOR ( 'NONE', #17669, 1000.000000000000114 ) ;
#16670 = VERTEX_POINT ( 'NONE', #23683 ) ;
#16671 = VERTEX_POINT ( 'NONE', #1762 ) ;
#16672 = CARTESIAN_POINT ( 'NONE',  ( 10.93730112725994097, -51.37919228020192008, -142.1801301103790536 ) ) ;
#16673 = CARTESIAN_POINT ( 'NONE',  ( 1.832998868059890096, -138.1720401012263721, -44.33343224355374446 ) ) ;
#16675 = CARTESIAN_POINT ( 'NONE',  ( 26.11404676487259024, 102.9690087468808031, -47.08215554553414961 ) ) ;
#16674 = CARTESIAN_POINT ( 'NONE',  ( 16.75465622695653067, 112.2763423369180771, 87.30527857298483241 ) ) ;
#16676 = CARTESIAN_POINT ( 'NONE',  ( -1.049819825607597235, -43.39756533277870432, 14.63675055554426407 ) ) ;
#16677 = CARTESIAN_POINT ( 'NONE',  ( -1.259920593601969729, -12.06711544331594865, -44.39818421957811978 ) ) ;
#16678 = EDGE_LOOP ( 'NONE', ( #281, #11432, #7448, #743 ) ) ;
#16679 = CARTESIAN_POINT ( 'NONE',  ( 2.263178113027040084, 71.48082833565062799, 126.6115605262340438 ) ) ;
#16680 = CARTESIAN_POINT ( 'NONE',  ( 55.79472521941426777, -14.41365263906501681, -71.31192372336690255 ) ) ;
#16681 = VERTEX_POINT ( 'NONE', #10559 ) ;
#16682 = DIRECTION ( 'NONE',  ( 1.000000000000000000, -6.938893903907226837E-18, 1.734723475976806709E-18 ) ) ;
#16683 = CARTESIAN_POINT ( 'NONE',  ( 24.01988960052063504, -23.05141021591188277, -129.0012934948649672 ) ) ;
#16684 = CARTESIAN_POINT ( 'NONE',  ( 25.86096068574580897, -67.25583614083905104, 90.87263912324389992 ) ) ;
#16685 = CARTESIAN_POINT ( 'NONE',  ( 1.831572820252009626, 116.8148281295980695, -86.09108691067652330 ) ) ;
#16686 = B_SPLINE_CURVE_WITH_KNOTS ( 'NONE', 3,
 ( #18107, #25045, #9780, #18549 ),
 .UNSPECIFIED., .F., .F.,
 ( 4, 4 ),
 ( 0.000000000000000000, 0.008383560773332712074 ),
 .UNSPECIFIED. ) ;
#16687 = CARTESIAN_POINT ( 'NONE',  ( 32.73300124599732186, 0.000000000000000000, 0.000000000000000000 ) ) ;
#16688 = CARTESIAN_POINT ( 'NONE',  ( -55.25719721206881729, 0.0006290797159209853082, -0.01115102788683027674 ) ) ;
#16689 = CARTESIAN_POINT ( 'NONE',  ( 10.93730112725978287, -125.1380233598484182, 84.82621002473399585 ) ) ;
#16690 = ORIENTED_EDGE ( 'NONE', *, *, #10334, .T. ) ;
#16691 = DIRECTION ( 'NONE',  ( 0.5946245182733607137, -0.1700465163848307315, 0.7858154137795702043 ) ) ;
#16692 = CARTESIAN_POINT ( 'NONE',  ( 8.186469777910600598, 122.8338388711459430, 84.95702201436446899 ) ) ;
#16693 = CARTESIAN_POINT ( 'NONE',  ( -4.178947244162637631, 47.46809051147737080, 11.88256963646688824 ) ) ;
#16694 = EDGE_CURVE ( 'NONE', #13886, #14659, #27142, .T. ) ;
#16695 = AXIS2_PLACEMENT_3D ( 'NONE', #14531, #1435, #10243 ) ;
#16696 = VERTEX_POINT ( 'NONE', #19742 ) ;
#16697 = CARTESIAN_POINT ( 'NONE',  ( -1.050231094221226291, 36.90262059116464854, -27.12595454131517769 ) ) ;
#16698 =( BOUNDED_SURFACE ( )  B_SPLINE_SURFACE ( 3, 1, ( 
 ( #15571, #26523 ),
 ( #17875, #2336 ),
 ( #328, #19621 ),
 ( #28390, #8692 ) ),
 .UNSPECIFIED., .F., .F., .F. ) 
 B_SPLINE_SURFACE_WITH_KNOTS ( ( 4, 4 ),
 ( 2, 2 ),
 ( 0.000000000000000000, 1.000000000000000000 ),
 ( 0.000000000000000000, 1.000000000000000000 ),
 .UNSPECIFIED. ) 
 GEOMETRIC_REPRESENTATION_ITEM ( )  RATIONAL_B_SPLINE_SURFACE ( (
 ( 1.000000000000000000, 1.000000000000000000),
 ( 0.9593753223639863714, 0.9995975284513187731),
 ( 0.9593753223639863714, 0.9995975284513187731),
 ( 1.000000000000000000, 1.000000000000000000) ) ) 
 REPRESENTATION_ITEM ( '' )  SURFACE ( )  );
#16699 = ADVANCED_FACE ( 'NONE', ( #6382 ), #13524, .F. ) ;
#16700 = EDGE_CURVE ( 'NONE', #26952, #18945, #2146, .T. ) ;
#16701 = CARTESIAN_POINT ( 'NONE',  ( 9.884929003653608603, 128.2151425008041201, 78.87917189084957670 ) ) ;
#16702 = CARTESIAN_POINT ( 'NONE',  ( 25.64660436782548203, -102.9120797476511484, 46.45435812945208198 ) ) ;
#16703 = CARTESIAN_POINT ( 'NONE',  ( 109.1589550718174877, -0.002874971999843706130, -0.007008495014548460529 ) ) ;
#16704 = CARTESIAN_POINT ( 'NONE',  ( -2.265401668238152588, 45.46007138824041505, -11.98901689611057009 ) ) ;
#16705 = CARTESIAN_POINT ( 'NONE',  ( -23.79248802219730052, -13.25839849636379597, -30.42578156345381046 ) ) ;
#16706 = CARTESIAN_POINT ( 'NONE',  ( 1.833838850093439943, 141.9387673160886152, 30.17001281793409717 ) ) ;
#16707 = B_SPLINE_CURVE_WITH_KNOTS ( 'NONE', 3,
 ( #3632, #27955, #23522, #5956 ),
 .UNSPECIFIED., .F., .F.,
 ( 4, 4 ),
 ( 3.214625617059125298E-16, 0.01077107486149843710 ),
 .UNSPECIFIED. ) ;
#16708 = LINE ( 'NONE', #19141, #24482 ) ;
#16709 = CARTESIAN_POINT ( 'NONE',  ( -8.786685647604890903, -48.22796981442753150, 23.24040270374441874 ) ) ;
#16710 = LINE ( 'NONE', #19005, #8572 ) ;
#16711 = VERTEX_POINT ( 'NONE', #17439 ) ;
#16712 = ORIENTED_EDGE ( 'NONE', *, *, #18851, .T. ) ;
#16713 = CARTESIAN_POINT ( 'NONE',  ( 1.833750490713687009, -30.43107162405965482, 141.8829662951652040 ) ) ;
#16714 = CARTESIAN_POINT ( 'NONE',  ( 1.833485406944043827, 107.4794113447409529, 97.49333871408727248 ) ) ;
#16715 = CARTESIAN_POINT ( 'NONE',  ( 26.28373643307411811, -17.46364395087380572, -126.3595147275200219 ) ) ;
#16716 = FACE_OUTER_BOUND ( 'NONE', #14310, .T. ) ;
#16717 = CARTESIAN_POINT ( 'NONE',  ( 2.433796855181219243, 107.1581411821798895, -98.43889364293755762 ) ) ;
#16718 = VECTOR ( 'NONE', #14429, 1000.000000000000114 ) ;
#16719 = CARTESIAN_POINT ( 'NONE',  ( -1.050231094221194983, -45.79908322896422135, 0.2545420581353859402 ) ) ;
#16720 = ORIENTED_EDGE ( 'NONE', *, *, #20176, .F. ) ;
#16721 = CARTESIAN_POINT ( 'NONE',  ( 32.73300124599732186, 0.000000000000000000, 0.000000000000000000 ) ) ;
#16722 = CARTESIAN_POINT ( 'NONE',  ( 13.36082413113063083, 148.1362653801007809, -37.97423473099148339 ) ) ;
#16723 = AXIS2_PLACEMENT_3D ( 'NONE', #13664, #7501, #11808 ) ;
#16724 = CARTESIAN_POINT ( 'NONE',  ( -1.046936909428682672, -37.78538189376526901, -25.87632113675147849 ) ) ;
#16725 = CARTESIAN_POINT ( 'NONE',  ( -20.57838717382308147, -28.96176188950224528, -7.715628353033566533 ) ) ;
#16726 = CARTESIAN_POINT ( 'NONE',  ( 13.84597867724975906, -144.4146018799364981, 25.80666409311521647 ) ) ;
#16727 = EDGE_CURVE ( 'NONE', #20281, #23165, #10846, .T. ) ;
#16728 = VERTEX_POINT ( 'NONE', #24371 ) ;
#16729 = CARTESIAN_POINT ( 'NONE',  ( -9.156249394959713683, -9.022661520477402775, 53.74753343182710807 ) ) ;
#16730 = B_SPLINE_CURVE_WITH_KNOTS ( 'NONE', 3,
 ( #10707, #10560, #26094, #19475, #6383, #12993 ),
 .UNSPECIFIED., .F., .F.,
 ( 4, 2, 4 ),
 ( 3.178475462313071774E-16, 0.003576372551511121031, 0.007152745103021923741 ),
 .UNSPECIFIED. ) ;
#16732 = CARTESIAN_POINT ( 'NONE',  ( 1.832998868059858122, -29.64765804470168931, 142.0492247521721936 ) ) ;
#16731 = B_SPLINE_CURVE_WITH_KNOTS ( 'NONE', 3,
 ( #19176, #18748, #1472, #14427, #25676, #27524 ),
 .UNSPECIFIED., .F., .F.,
 ( 4, 2, 4 ),
 ( 4.906538933386797396E-18, 0.0004335184443140297200, 0.0008670368886280544526 ),
 .UNSPECIFIED. ) ;
#16733 = ORIENTED_EDGE ( 'NONE', *, *, #8098, .T. ) ;
#16734 = ADVANCED_FACE ( 'NONE', ( #15275 ), #19413, .F. ) ;
#16735 = B_SPLINE_CURVE_WITH_KNOTS ( 'NONE', 3,
 ( #25762, #16971, #21144, #6054, #14809, #23618 ),
 .UNSPECIFIED., .F., .F.,
 ( 4, 2, 4 ),
 ( 0.000000000000000000, 0.0004335151646191501111, 0.0008670303292383002222 ),
 .UNSPECIFIED. ) ;
#16736 = ORIENTED_EDGE ( 'NONE', *, *, #18184, .F. ) ;
#16737 = CIRCLE ( 'NONE', #4297, 111.9614997405030152 ) ;
#16738 = EDGE_LOOP ( 'NONE', ( #9244, #18816, #1236, #17538 ) ) ;
#16739 = CARTESIAN_POINT ( 'NONE',  ( -55.24728320129491266, 0.01214321324517175435, -0.008013189884952098135 ) ) ;
#16740 = FACE_OUTER_BOUND ( 'NONE', #23402, .T. ) ;
#16741 = FACE_OUTER_BOUND ( 'NONE', #28257, .T. ) ;
#16742 = CARTESIAN_POINT ( 'NONE',  ( -20.24399999263415140, -1.282322917263260198, 29.60996018918694617 ) ) ;
#16743 = CARTESIAN_POINT ( 'NONE',  ( -1.045287976400365970, 1.530335034934747318, 45.76855895860941814 ) ) ;
#16744 = DIRECTION ( 'NONE',  ( 0.000000000000000000, 0.000000000000000000, 1.000000000000000000 ) ) ;
#16745 = CARTESIAN_POINT ( 'NONE',  ( -20.21097721712959583, 17.67178718142858429, -23.76068428613687189 ) ) ;
#16746 =( BOUNDED_SURFACE ( )  B_SPLINE_SURFACE ( 3, 1, ( 
 ( #8554, #26109 ),
 ( #17456, #13284 ),
 ( #26245, #331 ),
 ( #9121, #2194 ) ),
 .UNSPECIFIED., .F., .F., .F. ) 
 B_SPLINE_SURFACE_WITH_KNOTS ( ( 4, 4 ),
 ( 2, 2 ),
 ( 0.000000000000000000, 1.000000000000000000 ),
 ( 0.000000000000000000, 1.000000000000000000 ),
 .UNSPECIFIED. ) 
 GEOMETRIC_REPRESENTATION_ITEM ( )  RATIONAL_B_SPLINE_SURFACE ( (
 ( 1.000000000000000000, 1.000000000000000000),
 ( 0.7789835883360578528, 0.9689951854195403280),
 ( 0.7789835883360578528, 0.9689951854195403280),
 ( 1.000000000000000000, 1.000000000000000000) ) ) 
 REPRESENTATION_ITEM ( '' )  SURFACE ( )  );
#16747 = CARTESIAN_POINT ( 'NONE',  ( 1.833809397773843219, -85.14934054436398014, -117.5007887865417331 ) ) ;
#16749 = AXIS2_PLACEMENT_3D ( 'NONE', #27992, #12732, #12591 ) ;
#16748 = CARTESIAN_POINT ( 'NONE',  ( 10.93730112725932635, 0.000000000000000000, 0.000000000000000000 ) ) ;
#16750 = CARTESIAN_POINT ( 'NONE',  ( 13.84597867724977149, -77.45414123936289741, 124.5889929031783936 ) ) ;
#16751 = CARTESIAN_POINT ( 'NONE',  ( 109.1592201516379674, -0.007302213399779945366, 0.002913740842108614778 ) ) ;
#16752 = EDGE_CURVE ( 'NONE', #5056, #26248, #8690, .T. ) ;
#16753 = CARTESIAN_POINT ( 'NONE',  ( -55.24198130335446422, 0.008310594958153458625, -0.004163123460802744397 ) ) ;
#16754 = CARTESIAN_POINT ( 'NONE',  ( 10.93730112725990367, -149.7554878793147566, -20.69552240458495973 ) ) ;
#16755 = CARTESIAN_POINT ( 'NONE',  ( 25.64707127832796019, 6.059145946834079367E-17, -112.9112343549835487 ) ) ;
#16756 = CARTESIAN_POINT ( 'NONE',  ( 109.1587776205901577, -0.005390665547499397595, -0.004965871434389434319 ) ) ;
#16757 = CARTESIAN_POINT ( 'NONE',  ( 10.93730112726006354, 150.7858122213665126, -10.89264110824830034 ) ) ;
#16758 = CARTESIAN_POINT ( 'NONE',  ( 10.93730112725972425, -42.00474393596362432, 145.2260730187398678 ) ) ;
#16759 = EDGE_CURVE ( 'NONE', #16899, #5490, #18887, .T. ) ;
#16760 = ORIENTED_EDGE ( 'NONE', *, *, #1696, .T. ) ;
#16761 = CARTESIAN_POINT ( 'NONE',  ( 26.11404676487259024, 45.01677474591551942, -103.8885755249565079 ) ) ;
#16762 = EDGE_CURVE ( 'NONE', #26863, #3886, #26225, .T. ) ;
#16763 = VERTEX_POINT ( 'NONE', #16441 ) ;
#16764 = CARTESIAN_POINT ( 'NONE',  ( -20.20700224038492010, 8.199606986804733211, 28.44216453106527709 ) ) ;
#16765 = CARTESIAN_POINT ( 'NONE',  ( 55.49584447822657296, -70.91003759562305220, -15.34602024131360487 ) ) ;
#16766 = EDGE_LOOP ( 'NONE', ( #5000, #27721, #18099, #13690 ) ) ;
#16767 = B_SPLINE_CURVE_WITH_KNOTS ( 'NONE', 3,
 ( #20195, #484, #9277, #18177 ),
 .UNSPECIFIED., .F., .F.,
 ( 4, 4 ),
 ( 2.501853776554200607E-17, 0.008383560773332712074 ),
 .UNSPECIFIED. ) ;
#16768 = ORIENTED_EDGE ( 'NONE', *, *, #4511, .F. ) ;
#16769 = ORIENTED_EDGE ( 'NONE', *, *, #16114, .T. ) ;
#16770 = CARTESIAN_POINT ( 'NONE',  ( 1.833809397773846328, -141.9756687985004930, 29.99591688577042703 ) ) ;
#16771 = CARTESIAN_POINT ( 'NONE',  ( -23.79248802219722592, -32.40806545715335574, -7.157555990716774730 ) ) ;
#16772 = CARTESIAN_POINT ( 'NONE',  ( -20.24419206586952313, 1.282847120831654530, 29.61012937815439017 ) ) ;
#16773 = CARTESIAN_POINT ( 'NONE',  ( -1.619063947482197729, -25.20140673341345305, 38.92136151114934961 ) ) ;
#16774 = B_SPLINE_CURVE_WITH_KNOTS ( 'NONE', 3,
 ( #8075, #10628, #1974, #4138, #12498, #19397, #3870 ),
 .UNSPECIFIED., .F., .F.,
 ( 4, 3, 4 ),
 ( 0.000000000000000000, 0.02398743853561352557, 0.04000277880656219476 ),
 .UNSPECIFIED. ) ;
#16775 = CARTESIAN_POINT ( 'NONE',  ( -1.045287976400365970, 1.530335034934747318, 45.76855895860941814 ) ) ;
#16776 = CARTESIAN_POINT ( 'NONE',  ( 5.340103556456385903, 28.39990973640068717, 144.6887562347050959 ) ) ;
#16777 = CARTESIAN_POINT ( 'NONE',  ( 25.64703792032472052, 56.58441811305608127, 97.70949518026519343 ) ) ;
#16778 = CARTESIAN_POINT ( 'NONE',  ( 25.64681081121879203, -112.3352186517029878, -11.38886654529789233 ) ) ;
#16779 =( BOUNDED_SURFACE ( )  B_SPLINE_SURFACE ( 3, 1, ( 
 ( #4946, #11719 ),
 ( #2790, #15889 ),
 ( #26823, #24831 ),
 ( #9424, #5087 ) ),
 .UNSPECIFIED., .F., .F., .F. ) 
 B_SPLINE_SURFACE_WITH_KNOTS ( ( 4, 4 ),
 ( 2, 2 ),
 ( 0.000000000000000000, 1.000000000000000000 ),
 ( 0.000000000000000000, 1.000000000000000000 ),
 .UNSPECIFIED. ) 
 GEOMETRIC_REPRESENTATION_ITEM ( )  RATIONAL_B_SPLINE_SURFACE ( (
 ( 1.000000000000000000, 1.000000000000000000),
 ( 0.9934239774497837239, 0.8357310067453919133),
 ( 0.9934239774497837239, 0.8357310067453919133),
 ( 1.000000000000000000, 1.000000000000000000) ) ) 
 REPRESENTATION_ITEM ( '' )  SURFACE ( )  );
#16780 = ADVANCED_FACE ( 'NONE', ( #750 ), #21271, .F. ) ;
#16781 = EDGE_LOOP ( 'NONE', ( #25790, #21948, #7852, #15967 ) ) ;
#16782 = ORIENTED_EDGE ( 'NONE', *, *, #2844, .T. ) ;
#16783 = CARTESIAN_POINT ( 'NONE',  ( 1.833206308920053429, -29.44113170198447094, -142.0914675761167132 ) ) ;
#16784 = ADVANCED_FACE ( 'NONE', ( #27217 ), #2859, .F. ) ;
#16786 = DIRECTION ( 'NONE',  ( -0.5914120900931443270, -0.1754905759872788518, -0.7870418015781065479 ) ) ;
#16785 = DIRECTION ( 'NONE',  ( 0.000000000000000000, 5.223019709707975211E-21, -1.000000000000000000 ) ) ;
#16787 = CARTESIAN_POINT ( 'NONE',  ( 26.11404676487257603, -107.3263591096432776, 36.06104232266415721 ) ) ;
#16788 = CARTESIAN_POINT ( 'NONE',  ( 26.04756280548354397, 10.72497307632943730, -112.6689254848258059 ) ) ;
#16789 = CARTESIAN_POINT ( 'NONE',  ( 26.11404676487257603, 92.25884714080498838, -65.63269960453146723 ) ) ;
#16790 = EDGE_LOOP ( 'NONE', ( #5758, #16942, #7374, #26260 ) ) ;
#16791 = CARTESIAN_POINT ( 'NONE',  ( 1.833485406944043827, 137.8414413349092058, -45.34878176254091642 ) ) ;
#16792 = ADVANCED_FACE ( 'NONE', ( #9252 ), #22364, .F. ) ;
#16793 = CARTESIAN_POINT ( 'NONE',  ( -1.058197053496162887, 36.00048521498994347, 28.32422455455037991 ) ) ;
#16794 = CARTESIAN_POINT ( 'NONE',  ( 109.1589550718175161, 0.001014448720249546245, 0.007507020724820358780 ) ) ;
#16795 = ORIENTED_EDGE ( 'NONE', *, *, #26728, .T. ) ;
#16796 = B_SPLINE_CURVE_WITH_KNOTS ( 'NONE', 3,
 ( #8935, #22604, #22898, #27026, #11798, #18249 ),
 .UNSPECIFIED., .F., .F.,
 ( 4, 2, 4 ),
 ( 4.286557520396696095E-16, 0.003576372551511235957, 0.007152745103022043437 ),
 .UNSPECIFIED. ) ;
#16797 = ORIENTED_EDGE ( 'NONE', *, *, #22975, .F. ) ;
#16798 = LINE ( 'NONE', #16925, #17644 ) ;
#16799 = EDGE_CURVE ( 'NONE', #17966, #14867, #25226, .T. ) ;
#16800 = EDGE_LOOP ( 'NONE', ( #11324, #2463, #22457, #14864 ) ) ;
#16801 = ORIENTED_EDGE ( 'NONE', *, *, #22872, .F. ) ;
#16802 = CARTESIAN_POINT ( 'NONE',  ( 1.833809397773859429, 96.96506043213450710, 107.9565774559014670 ) ) ;
#16803 = ORIENTED_EDGE ( 'NONE', *, *, #9635, .T. ) ;
#16804 = CARTESIAN_POINT ( 'NONE',  ( -1.539763995773687055, -43.19716353142342768, -16.63252574783026816 ) ) ;
#16805 = CARTESIAN_POINT ( 'NONE',  ( -25.21435515916025594, 1.749597353048488237E-16, -4.373993382621220594E-17 ) ) ;
#16806 = CARTESIAN_POINT ( 'NONE',  ( 1.832998868059858122, 58.53348008137825076, -132.7810136645732371 ) ) ;
#16807 = CARTESIAN_POINT ( 'NONE',  ( 55.49584447822657296, -29.75369869230999242, 66.16986612640766907 ) ) ;
#16808 = CARTESIAN_POINT ( 'NONE',  ( 25.69398547355838502, -107.1830796521256843, 35.60637981494814142 ) ) ;
#16809 = CARTESIAN_POINT ( 'NONE',  ( 25.70243777736188306, -46.60897284577234956, 102.8829101922929681 ) ) ;
#16810 = CARTESIAN_POINT ( 'NONE',  ( -20.24399999263414784, 29.60996018918694617, 1.282322917263571282 ) ) ;
#16811 = ORIENTED_EDGE ( 'NONE', *, *, #8812, .T. ) ;
#16812 = CARTESIAN_POINT ( 'NONE',  ( -28.41354790283022069, 14.62505768302827036, 18.00456980371883731 ) ) ;
#16814 = CARTESIAN_POINT ( 'NONE',  ( 13.36082413113061307, 22.28175172543762272, -151.2941478187905489 ) ) ;
#16813 = CARTESIAN_POINT ( 'NONE',  ( 55.49584447822657296, -58.85239198729215104, 42.42793568432939111 ) ) ;
#16815 = CARTESIAN_POINT ( 'NONE',  ( -8.786685647604890903, 23.24040270374391426, -48.22796981442777309 ) ) ;
#16816 = VERTEX_POINT ( 'NONE', #612 ) ;
#16817 = ORIENTED_EDGE ( 'NONE', *, *, #14563, .F. ) ;
#16818 = CARTESIAN_POINT ( 'NONE',  ( -1.045287976400365970, -25.66401692419961833, 37.92705037016786918 ) ) ;
#16819 = CARTESIAN_POINT ( 'NONE',  ( -25.21435515916043713, -34.05351380035328646, 6.169479169075816394 ) ) ;
#16820 = EDGE_CURVE ( 'NONE', #3533, #6430, #12462, .T. ) ;
#16822 = CARTESIAN_POINT ( 'NONE',  ( 2.433796855181233454, 137.9325382748291418, -46.34326152018600453 ) ) ;
#16821 = FACE_OUTER_BOUND ( 'NONE', #13761, .T. ) ;
#16823 = CARTESIAN_POINT ( 'NONE',  ( -20.20612092514784308, -8.058517256680906016, 28.48192215759674184 ) ) ;
#16824 = CARTESIAN_POINT ( 'NONE',  ( 1.833691583653511259, -132.4191286035302539, -59.34641645332771986 ) ) ;
#16825 = ORIENTED_EDGE ( 'NONE', *, *, #676, .F. ) ;
#16826 = DIRECTION ( 'NONE',  ( -0.5914120900931443270, -0.4101107478122021921, -0.6942916636548178699 ) ) ;
#16827 = CARTESIAN_POINT ( 'NONE',  ( -1.539763995773674177, 38.84665165401067810, -25.17088606276561080 ) ) ;
#16828 = VECTOR ( 'NONE', #25394, 1000.000000000000000 ) ;
#16829 = ORIENTED_EDGE ( 'NONE', *, *, #24422, .T. ) ;
#16830 = CARTESIAN_POINT ( 'NONE',  ( -15.02187109954783217, 40.82269973458240031, -21.95370994985588098 ) ) ;
#16831 = CARTESIAN_POINT ( 'NONE',  ( -20.24419206586952313, 1.282847120831654530, 29.61012937815439017 ) ) ;
#16832 = CARTESIAN_POINT ( 'NONE',  ( -1.048994561756806831, 14.87838255483256233, -43.31369460697981566 ) ) ;
#16833 = DIRECTION ( 'NONE',  ( 1.000000000000000000, 0.000000000000000000, 0.000000000000000000 ) ) ;
#16834 = ADVANCED_FACE ( 'NONE', ( #22938 ), #1418, .T. ) ;
#16835 = CARTESIAN_POINT ( 'NONE',  ( -20.20700224038492721, 24.51628800869048419, -16.58740185276719359 ) ) ;
#16836 = CARTESIAN_POINT ( 'NONE',  ( -2.904412668506670681, 40.16685646686207889, -25.64203923793588302 ) ) ;
#16837 = CARTESIAN_POINT ( 'NONE',  ( 13.36082413113063083, -142.1654513177084311, -56.35051087435107320 ) ) ;
#16838 = ORIENTED_EDGE ( 'NONE', *, *, #22996, .F. ) ;
#16839 = CARTESIAN_POINT ( 'NONE',  ( 13.84597867724975195, -35.16314962059933436, 142.4258194868991438 ) ) ;
#16840 =( BOUNDED_SURFACE ( )  B_SPLINE_SURFACE ( 3, 1, ( 
 ( #11751, #2528 ),
 ( #805, #20085 ),
 ( #18347, #15771 ),
 ( #27130, #13611 ) ),
 .UNSPECIFIED., .F., .F., .F. ) 
 B_SPLINE_SURFACE_WITH_KNOTS ( ( 4, 4 ),
 ( 2, 2 ),
 ( 0.000000000000000000, 1.000000000000000000 ),
 ( 0.000000000000000000, 1.000000000000000000 ),
 .UNSPECIFIED. ) 
 GEOMETRIC_REPRESENTATION_ITEM ( )  RATIONAL_B_SPLINE_SURFACE ( (
 ( 1.000000000000000000, 1.000000000000000000),
 ( 0.9956975270656954757, 0.8568959468854893125),
 ( 0.9956975270656954757, 0.8568959468854893125),
 ( 1.000000000000000000, 1.000000000000000000) ) ) 
 REPRESENTATION_ITEM ( '' )  SURFACE ( )  );
#16841 = VERTEX_POINT ( 'NONE', #24675 ) ;
#16842 = CARTESIAN_POINT ( 'NONE',  ( 13.36082413113061307, -37.97423473099395608, 148.1362653801001841 ) ) ;
#16843 = CARTESIAN_POINT ( 'NONE',  ( -1.046936909428679119, -45.77873603877005593, 1.275306677858721649 ) ) ;
#16844 = CARTESIAN_POINT ( 'NONE',  ( -24.53239521893646824, 3.868435622621471115, -33.71193723315172264 ) ) ;
#16845 = CARTESIAN_POINT ( 'NONE',  ( 109.1778270068192853, -0.005755170886745476951, 0.007323887274071875716 ) ) ;
#16846 = DIRECTION ( 'NONE',  ( -0.5946245182733607137, 0.6948076064830713827, -0.4045541647807359142 ) ) ;
#16847 = B_SPLINE_CURVE_WITH_KNOTS ( 'NONE', 3,
 ( #13979, #1037, #3471, #7525, #5488, #12257, #27211, #14250, #16573, #16285 ),
 .UNSPECIFIED., .F., .F.,
 ( 4, 3, 3, 4 ),
 ( 0.000000000000000000, 0.0002669560319015770256, 0.0005492286108966617283, 0.0008315040496093522703 ),
 .UNSPECIFIED. ) ;
#16848 = CARTESIAN_POINT ( 'NONE',  ( 26.04756280548354042, 74.90181827458462749, -84.84709444968828507 ) ) ;
#16849 = DIRECTION ( 'NONE',  ( -0.5914120900931443270, 0.2415416038593066195, -0.7693434820005511376 ) ) ;
#16850 = CARTESIAN_POINT ( 'NONE',  ( -28.41354790283022069, -22.41474081378005323, -5.969609727607934957 ) ) ;
#16851 = CARTESIAN_POINT ( 'NONE',  ( -1.539763995773684835, -46.22267697748605997, -2.469814354917328370 ) ) ;
#16852 = ORIENTED_EDGE ( 'NONE', *, *, #23364, .F. ) ;
#16853 = ORIENTED_EDGE ( 'NONE', *, *, #20662, .T. ) ;
#16854 = ORIENTED_EDGE ( 'NONE', *, *, #9276, .T. ) ;
#16855 = CARTESIAN_POINT ( 'NONE',  ( 32.73300124599734318, 89.94078864464067635, 75.82012867748514395 ) ) ;
#16856 = DIRECTION ( 'NONE',  ( 1.000000000000000000, -6.938893903907226837E-18, 1.734723475976806709E-18 ) ) ;
#16857 = EDGE_CURVE ( 'NONE', #26, #26730, #16244, .T. ) ;
#16858 = CARTESIAN_POINT ( 'NONE',  ( 109.1721716018069657, -0.005082060336469301429, 0.01629455849720095120 ) ) ;
#16859 = CARTESIAN_POINT ( 'NONE',  ( 25.64692872815578539, -83.69378511050511804, -75.79105864157472183 ) ) ;
#16860 = FACE_OUTER_BOUND ( 'NONE', #13949, .T. ) ;
#16861 = CARTESIAN_POINT ( 'NONE',  ( 1.832998868059890096, -141.8272129421606564, -30.69214149074156595 ) ) ;
#16862 = CARTESIAN_POINT ( 'NONE',  ( -55.24728320129491266, -0.0006547948648744401781, 0.01453410071985650025 ) ) ;
#16863 = ORIENTED_EDGE ( 'NONE', *, *, #12230, .T. ) ;
#16864 = CARTESIAN_POINT ( 'NONE',  ( 16.75465622695658396, 108.7410129416647493, -91.67104679059791295 ) ) ;
#16865 = CARTESIAN_POINT ( 'NONE',  ( -55.24390624410018802, 0.007245494385991800047, -0.007503127514277958821 ) ) ;
#16866 = CARTESIAN_POINT ( 'NONE',  ( 32.73300124599737160, -75.82012867748541396, 89.94078864464039214 ) ) ;
#16867 = EDGE_CURVE ( 'NONE', #28198, #14392, #7868, .T. ) ;
#16868 = EDGE_CURVE ( 'NONE', #8004, #7205, #6615, .T. ) ;
#16869 = FACE_BOUND ( 'NONE', #7610, .T. ) ;
#16870 = EDGE_LOOP ( 'NONE', ( #20831, #6376, #25755, #27054 ) ) ;
#16871 = CARTESIAN_POINT ( 'NONE',  ( 109.1586059443104944, -0.001740416220259453526, -0.006856640434643066981 ) ) ;
#16872 = CARTESIAN_POINT ( 'NONE',  ( 25.81918753295379076, -97.41320410180124156, 57.31966094783169297 ) ) ;
#16873 = ORIENTED_EDGE ( 'NONE', *, *, #7209, .F. ) ;
#16874 = ORIENTED_EDGE ( 'NONE', *, *, #17304, .T. ) ;
#16875 = ORIENTED_EDGE ( 'NONE', *, *, #28350, .T. ) ;
#16876 = VECTOR ( 'NONE', #14532, 1000.000000000000114 ) ;
#16877 = CARTESIAN_POINT ( 'NONE',  ( 25.64703792032470631, -110.4746717456747689, -23.32999623362237784 ) ) ;
#16878 = ADVANCED_FACE ( 'NONE', ( #3769 ), #10433, .F. ) ;
#16879 = CARTESIAN_POINT ( 'NONE',  ( 1.832998868059890096, -0.5339089137737788038, -145.1092030902949830 ) ) ;
#16880 = EDGE_CURVE ( 'NONE', #18117, #22173, #24459, .T. ) ;
#16881 = CARTESIAN_POINT ( 'NONE',  ( -12.94347594948484037, 33.69581619287875895, -35.22469990145616237 ) ) ;
#16882 = ORIENTED_EDGE ( 'NONE', *, *, #15897, .T. ) ;
#16883 = CARTESIAN_POINT ( 'NONE',  ( 1.833838850093452821, 59.02145475724827151, -132.5643663243751860 ) ) ;
#16884 = CARTESIAN_POINT ( 'NONE',  ( 109.1624594426973118, 0.01358749486988782354, -0.008380433676412963467 ) ) ;
#16885 = ADVANCED_FACE ( 'NONE', ( #16740 ), #5084, .T. ) ;
#16886 = CARTESIAN_POINT ( 'NONE',  ( -1.048172774974290178, -1.020161070261438097, -45.78636862970792265 ) ) ;
#16887 = CARTESIAN_POINT ( 'NONE',  ( 1.834118845439484335, 72.70910183320742703, -125.5799175751962196 ) ) ;
#16888 = FACE_OUTER_BOUND ( 'NONE', #2546, .T. ) ;
#16889 = CARTESIAN_POINT ( 'NONE',  ( 109.1586059443104944, -0.003774052605966671768, -0.005983234375914136226 ) ) ;
#16890 = CARTESIAN_POINT ( 'NONE',  ( 109.1592201516379674, -0.004368284148529054563, -0.006536841731953389224 ) ) ;
#16891 = CARTESIAN_POINT ( 'NONE',  ( -21.41427618760457818, -16.60878262545437778, -25.94789270595500597 ) ) ;
#16892 = CARTESIAN_POINT ( 'NONE',  ( -7.078251931573406708, 47.71415099571806451, -20.86696228105241602 ) ) ;
#16893 = ORIENTED_EDGE ( 'NONE', *, *, #11159, .T. ) ;
#16894 = EDGE_LOOP ( 'NONE', ( #16371, #3993, #27573, #9130 ) ) ;
#16895 = CARTESIAN_POINT ( 'NONE',  ( -8.259864102781673267, -52.60025989855198247, 6.590267880897466846 ) ) ;
#16896 = DIRECTION ( 'NONE',  ( -1.000000000000000000, -0.000000000000000000, -0.000000000000000000 ) ) ;
#16897 = ORIENTED_EDGE ( 'NONE', *, *, #23129, .T. ) ;
#16898 = ORIENTED_EDGE ( 'NONE', *, *, #28160, .T. ) ;
#16899 = VERTEX_POINT ( 'NONE', #10118 ) ;
#16900 = CARTESIAN_POINT ( 'NONE',  ( -20.20612092514784308, 16.46550332780526915, -24.59769888281538996 ) ) ;
#16901 = ADVANCED_FACE ( 'NONE', ( #19033 ), #25316, .F. ) ;
#16902 = CARTESIAN_POINT ( 'NONE',  ( 6.224689322667647851, 28.26953958630820551, -145.3353551538638158 ) ) ;
#16903 = EDGE_CURVE ( 'NONE', #27586, #9124, #10406, .T. ) ;
#16904 = LINE ( 'NONE', #21789, #25863 ) ;
#16905 = CARTESIAN_POINT ( 'NONE',  ( 55.49584447822657296, -48.74506217377846440, -53.73688382046314871 ) ) ;
#16906 = EDGE_CURVE ( 'NONE', #17251, #10554, #21180, .T. ) ;
#16907 = CARTESIAN_POINT ( 'NONE',  ( 25.64681081121880624, 102.9795863647034935, -46.30456157731225630 ) ) ;
#16908 = CARTESIAN_POINT ( 'NONE',  ( -1.464342487929844783, -44.64187261869788870, -11.94843286121900228 ) ) ;
#16909 = CARTESIAN_POINT ( 'NONE',  ( 26.11404676487259024, -112.7148551500679616, -10.71016160607683432 ) ) ;
#16910 = VECTOR ( 'NONE', #25210, 1000.000000000000000 ) ;
#16911 = ORIENTED_EDGE ( 'NONE', *, *, #17732, .T. ) ;
#16912 = ORIENTED_EDGE ( 'NONE', *, *, #1840, .F. ) ;
#16913 = CARTESIAN_POINT ( 'NONE',  ( -1.049819825607597235, -26.50610175068240792, 37.34982882986871999 ) ) ;
#16915 = CARTESIAN_POINT ( 'NONE',  ( -8.786685647604890903, -37.00619870957905277, 38.68584556812340480 ) ) ;
#16914 = CARTESIAN_POINT ( 'NONE',  ( 5.340103579038172121, -13.12023871299826538, 146.8647350263016733 ) ) ;
#16916 = CARTESIAN_POINT ( 'NONE',  ( 25.64708228042121974, -103.1335618347708589, -45.96113332231442428 ) ) ;
#16917 = CARTESIAN_POINT ( 'NONE',  ( -20.21097721712959938, 9.464413111084745367, -28.05863618200111986 ) ) ;
#16918 = CARTESIAN_POINT ( 'NONE',  ( 25.65782528836483323, 112.3587790429871376, -11.22838748007500342 ) ) ;
#16919 = ORIENTED_EDGE ( 'NONE', *, *, #23129, .F. ) ;
#16920 = CARTESIAN_POINT ( 'NONE',  ( 109.1587776205901861, -8.330235398541230849E-05, -0.007328861771499511728 ) ) ;
#16921 = CARTESIAN_POINT ( 'NONE',  ( 26.11404676487257603, -36.06104232266378062, -107.3263591096434197 ) ) ;
#16922 = CARTESIAN_POINT ( 'NONE',  ( -1.583189561560255143, 29.24830400313165413, -36.01941156322797610 ) ) ;
#16923 = ORIENTED_EDGE ( 'NONE', *, *, #17053, .F. ) ;
#16924 = VERTEX_POINT ( 'NONE', #27513 ) ;
#16925 = CARTESIAN_POINT ( 'NONE',  ( 55.79472521941426777, 62.63970324008261059, 37.00555938668281897 ) ) ;
#16926 = ORIENTED_EDGE ( 'NONE', *, *, #21752, .T. ) ;
#16927 = VERTEX_POINT ( 'NONE', #10274 ) ;
#16928 = CARTESIAN_POINT ( 'NONE',  ( 1.833485406944057594, -85.72460230293616235, -117.0814567582553281 ) ) ;
#16929 = EDGE_CURVE ( 'NONE', #20088, #20677, #17602, .T. ) ;
#16930 = ORIENTED_EDGE ( 'NONE', *, *, #22408, .F. ) ;
#16931 = CARTESIAN_POINT ( 'NONE',  ( 109.1587776205901577, -0.003736572840486988237, 0.006305329297952406813 ) ) ;
#16932 = CARTESIAN_POINT ( 'NONE',  ( -1.619063947482197729, -44.80407745103793360, -11.94059994246142331 ) ) ;
#16933 = ADVANCED_FACE ( 'NONE', ( #7822 ), #27136, .F. ) ;
#16934 = CARTESIAN_POINT ( 'NONE',  ( 25.98552792386798060, -107.2612904323492415, 35.98568266743475874 ) ) ;
#16935 = DIRECTION ( 'NONE',  ( 0.000000000000000000, -1.000000000000000000, 0.000000000000000000 ) ) ;
#16936 = ADVANCED_FACE ( 'NONE', ( #23796 ), #28230, .F. ) ;
#16937 = CARTESIAN_POINT ( 'NONE',  ( -20.57838717382308147, 7.715628353034087894, 28.96176188950209962 ) ) ;
#16939 = CARTESIAN_POINT ( 'NONE',  ( -1.046935749540010674, 43.93230528057182482, -12.93334586714193790 ) ) ;
#16938 = DIRECTION ( 'NONE',  ( -0.5946245182733608248, -0.7999021332774018944, -0.08110646981859884197 ) ) ;
#16940 = CARTESIAN_POINT ( 'NONE',  ( -1.155001620486255209, 28.62773628245669499, -35.88346938217563320 ) ) ;
#16941 = ORIENTED_EDGE ( 'NONE', *, *, #10957, .F. ) ;
#16942 = ORIENTED_EDGE ( 'NONE', *, *, #27127, .F. ) ;
#16943 = CARTESIAN_POINT ( 'NONE',  ( 26.11404676487256893, 1.130420376098718593, -113.2169081140373663 ) ) ;
#16944 = CARTESIAN_POINT ( 'NONE',  ( -7.733045908741326357, -51.44704017882769875, 10.42750254442592706 ) ) ;
#16945 = DIRECTION ( 'NONE',  ( 1.000000000000000000, -6.938893903907226837E-18, 1.734723475976806709E-18 ) ) ;
#16946 = CARTESIAN_POINT ( 'NONE',  ( 32.73300124599735028, -8.473903470906931190, 117.3295799645429156 ) ) ;
#16947 = ORIENTED_EDGE ( 'NONE', *, *, #9691, .F. ) ;
#16948 = CARTESIAN_POINT ( 'NONE',  ( -20.57838717382308147, 18.89542499756500149, -23.26537097894111383 ) ) ;
#16949 = CONICAL_SURFACE ( 'NONE', #4520, 117.6351876552689504, 0.9945805576725580410 ) ;
#16950 = CARTESIAN_POINT ( 'NONE',  ( 109.1586059443104944, -0.005881369279880122557, -0.003930911098385057520 ) ) ;
#16951 = VERTEX_POINT ( 'NONE', #24202 ) ;
#16952 = CARTESIAN_POINT ( 'NONE',  ( 25.64708010899966695, -112.2870082086266876, 11.85684669924934020 ) ) ;
#16953 = LINE ( 'NONE', #27893, #13251 ) ;
#16954 = CARTESIAN_POINT ( 'NONE',  ( 8.186469777910977186, 71.65198614410387279, -131.0413692044505183 ) ) ;
#16955 = CARTESIAN_POINT ( 'NONE',  ( -1.583189561560252701, -36.01941156322808268, -29.24830400313153334 ) ) ;
#16956 = CARTESIAN_POINT ( 'NONE',  ( -25.21435515916043713, -31.17620025257598471, -15.02493970636134613 ) ) ;
#16957 = ORIENTED_EDGE ( 'NONE', *, *, #21531, .F. ) ;
#16958 = CARTESIAN_POINT ( 'NONE',  ( 109.1778270068192853, -0.005967275455179280735, 0.007152128381196012907 ) ) ;
#16959 = CARTESIAN_POINT ( 'NONE',  ( -8.786685647604890903, -52.67761315067293282, -9.545808661480407409 ) ) ;
#16960 = ORIENTED_EDGE ( 'NONE', *, *, #12506, .F. ) ;
#16961 = PLANE ( 'NONE',  #26647 ) ;
#16962 = VERTEX_POINT ( 'NONE', #4183 ) ;
#16963 = EDGE_CURVE ( 'NONE', #9224, #12584, #23454, .T. ) ;
#16964 = CARTESIAN_POINT ( 'NONE',  ( 109.1624594426973118, 0.01582142368019176168, -0.002129375066974309536 ) ) ;
#16965 = EDGE_CURVE ( 'NONE', #20839, #21026, #11757, .T. ) ;
#16966 = ORIENTED_EDGE ( 'NONE', *, *, #15281, .F. ) ;
#16967 = CARTESIAN_POINT ( 'NONE',  ( -1.259972190295302497, -12.06706380853662530, 44.39825172539707410 ) ) ;
#16968 = CARTESIAN_POINT ( 'NONE',  ( -1.050229599974480843, -43.47850826583062656, -14.39582765040444912 ) ) ;
#16969 = CARTESIAN_POINT ( 'NONE',  ( 2.430230287190589422, 109.1043569252014436, 96.28466919684133529 ) ) ;
#16970 = EDGE_CURVE ( 'NONE', #7524, #27159, #8773, .T. ) ;
#16971 = CARTESIAN_POINT ( 'NONE',  ( -20.47566262905009538, 18.81547655725247381, -23.19796652405680248 ) ) ;
#16972 = CARTESIAN_POINT ( 'NONE',  ( -55.24728320129491266, 0.005114031043466756021, 0.01362040845703047127 ) ) ;
#16973 = CARTESIAN_POINT ( 'NONE',  ( 13.84597867724996689, 145.3211459389820561, 20.08297016719431127 ) ) ;
#16974 = CARTESIAN_POINT ( 'NONE',  ( -1.044557008772710516, -28.22896138707343994, 36.05793264791374497 ) ) ;
#16975 = CARTESIAN_POINT ( 'NONE',  ( 25.64708010899964563, 112.2870082086267871, -11.85684669924855328 ) ) ;
#16976 = CARTESIAN_POINT ( 'NONE',  ( 25.64703792032469920, 34.74993974077101200, -107.4308312803555197 ) ) ;
#16977 = ORIENTED_EDGE ( 'NONE', *, *, #10124, .F. ) ;
#16978 = ORIENTED_EDGE ( 'NONE', *, *, #25998, .T. ) ;
#16979 = CARTESIAN_POINT ( 'NONE',  ( 25.86096068574580187, -97.40497849554850518, -57.38862431273688003 ) ) ;
#16980 = CARTESIAN_POINT ( 'NONE',  ( -1.464342487929851222, 16.57334911911573982, 43.13914623307943685 ) ) ;
#16981 = CARTESIAN_POINT ( 'NONE',  ( -28.13707043255157103, 6.342158660427001493, -22.00298671236742010 ) ) ;
#16982 = DIRECTION ( 'NONE',  ( 0.000000000000000000, 0.000000000000000000, 1.000000000000000000 ) ) ;
#16983 =( BOUNDED_SURFACE ( )  B_SPLINE_SURFACE ( 3, 1, ( 
 ( #9095, #22790 ),
 ( #5346, #23220 ),
 ( #21024, #12121 ),
 ( #22932, #16729 ) ),
 .UNSPECIFIED., .F., .F., .F. ) 
 B_SPLINE_SURFACE_WITH_KNOTS ( ( 4, 4 ),
 ( 2, 2 ),
 ( 0.000000000000000000, 1.000000000000000000 ),
 ( 0.000000000000000000, 1.000000000000000000 ),
 .UNSPECIFIED. ) 
 GEOMETRIC_REPRESENTATION_ITEM ( )  RATIONAL_B_SPLINE_SURFACE ( (
 ( 1.000000000000000000, 1.000000000000000000),
 ( 0.7789835883360576307, 0.9689951854195403280),
 ( 0.7789835883360576307, 0.9689951854195403280),
 ( 1.000000000000000000, 1.000000000000000000) ) ) 
 REPRESENTATION_ITEM ( '' )  SURFACE ( )  );
#16984 = CARTESIAN_POINT ( 'NONE',  ( 1.832998868059858122, 132.7810136645746582, -58.53348008137513858 ) ) ;
#16985 = CARTESIAN_POINT ( 'NONE',  ( -1.048171036023513913, 27.73816396939564299, -36.44209502233717046 ) ) ;
#16986 = ORIENTED_EDGE ( 'NONE', *, *, #10006, .T. ) ;
#16987 = CARTESIAN_POINT ( 'NONE',  ( 2.433796855181205476, 116.8607839509056561, 86.69855925934011509 ) ) ;
#16988 = CARTESIAN_POINT ( 'NONE',  ( 16.05277956358206382, -62.52511797226036094, -128.9466020665980750 ) ) ;
#16989 = CARTESIAN_POINT ( 'NONE',  ( 13.36082413113061307, -41.18148072373512747, -147.2768864064171908 ) ) ;
#16990 = CARTESIAN_POINT ( 'NONE',  ( 25.98552792386800192, 1.078856412010833266, 113.1317367103341098 ) ) ;
#16991 = EDGE_LOOP ( 'NONE', ( #25382, #27212, #28372, #11262 ) ) ;
#16992 = CARTESIAN_POINT ( 'NONE',  ( -20.57838717382308147, 10.78122205917000365, -27.96569011373090063 ) ) ;
#16993 = CARTESIAN_POINT ( 'NONE',  ( -1.048171036023513247, 1.020520027229132598, -45.78635789057864969 ) ) ;
#16994 = ORIENTED_EDGE ( 'NONE', *, *, #13253, .F. ) ;
#16995 = VERTEX_POINT ( 'NONE', #17699 ) ;
#16996 = ORIENTED_EDGE ( 'NONE', *, *, #12959, .T. ) ;
#16997 = ADVANCED_FACE ( 'NONE', ( #2145 ), #5822, .F. ) ;
#16998 = DIRECTION ( 'NONE',  ( -0.5914120900931443270, -0.6570486713847213389, -0.4674599267565414662 ) ) ;
#16999 = DIRECTION ( 'NONE',  ( -1.000000000000000000, -0.000000000000000000, -0.000000000000000000 ) ) ;
#17000 = ADVANCED_FACE ( 'NONE', ( #17144 ), #1600, .F. ) ;
#17001 = CARTESIAN_POINT ( 'NONE',  ( 109.1592201516379674, 0.006536841731962000392, 0.004368284148525281539 ) ) ;
#17002 = EDGE_CURVE ( 'NONE', #4028, #10703, #27915, .T. ) ;
#17003 = CARTESIAN_POINT ( 'NONE',  ( -1.044557008772714513, -12.57891310333380552, -44.03203053429566438 ) ) ;
#17004 = ORIENTED_EDGE ( 'NONE', *, *, #10522, .F. ) ;
#17005 = DIRECTION ( 'NONE',  ( 0.5914120900931444380, -0.4804373588864852551, 0.6476200150380136966 ) ) ;
#17006 = CARTESIAN_POINT ( 'NONE',  ( 2.433796855181233454, 46.34326152018744693, 137.9325382748286870 ) ) ;
#17007 = CARTESIAN_POINT ( 'NONE',  ( -21.41430102051752016, 23.81424706376365918, -19.54553566814595200 ) ) ;
#17008 = CARTESIAN_POINT ( 'NONE',  ( -25.21435515916043713, 34.05351380035342146, 6.169479169075106739 ) ) ;
#17009 = CARTESIAN_POINT ( 'NONE',  ( 1.833485406944043827, 97.49333871408838093, -107.4794113447399297 ) ) ;
#17010 = CARTESIAN_POINT ( 'NONE',  ( -25.21435515916044423, -16.39063784838720395, 30.48034229288656505 ) ) ;
#17011 = DIRECTION ( 'NONE',  ( -0.000000000000000000, -0.000000000000000000, 1.000000000000000000 ) ) ;
#17012 = CYLINDRICAL_SURFACE ( 'NONE', #26777, 80.00000000000000000 ) ;
#17013 = CARTESIAN_POINT ( 'NONE',  ( -55.24271866751342941, 0.004256484107793635611, 0.008488649505346116536 ) ) ;
#17014 = CARTESIAN_POINT ( 'NONE',  ( 25.64681081121879203, 12.21581276189956711, -112.2483031020012305 ) ) ;
#17015 = ORIENTED_EDGE ( 'NONE', *, *, #20068, .F. ) ;
#17016 = ORIENTED_EDGE ( 'NONE', *, *, #9207, .T. ) ;
#17017 = CARTESIAN_POINT ( 'NONE',  ( -1.113427685306987991, 38.22586258295232398, 25.34053733836490707 ) ) ;
#17018 = CONICAL_SURFACE ( 'NONE', #9213, 34.60786435723138510, 0.8559913436420825139 ) ;
#17019 = CARTESIAN_POINT ( 'NONE',  ( -23.79223135445719350, -30.42557260166821109, -13.25822371132282917 ) ) ;
#17020 = EDGE_LOOP ( 'NONE', ( #27248, #16500, #9954, #23769 ) ) ;
#17021 = VECTOR ( 'NONE', #15781, 999.9999999999998863 ) ;
#17022 = ORIENTED_EDGE ( 'NONE', *, *, #96, .F. ) ;
#17023 = VERTEX_POINT ( 'NONE', #21602 ) ;
#17024 = VECTOR ( 'NONE', #15208, 1000.000000000000114 ) ;
#17025 = EDGE_CURVE ( 'NONE', #3564, #21873, #24867, .T. ) ;
#17026 = B_SPLINE_CURVE_WITH_KNOTS ( 'NONE', 3,
 ( #14172, #27718, #16793, #1230, #23140, #3397, #25139, #11887, #12446, #10174 ),
 .UNSPECIFIED., .F., .F.,
 ( 4, 2, 2, 2, 4 ),
 ( 2.976713740813343128E-16, 0.0003346187017559132675, 0.0006692374035115289214, 0.001003856105267144630, 0.001338474807022760121 ),
 .UNSPECIFIED. ) ;
#17027 = CARTESIAN_POINT ( 'NONE',  ( -55.24300891470650754, 0.002702093572893664395, -0.009439835024159005245 ) ) ;
#17028 = EDGE_CURVE ( 'NONE', #13981, #17451, #14738, .T. ) ;
#17029 = CARTESIAN_POINT ( 'NONE',  ( -1.619063947482197729, 2.489035965910159298, -46.30105812165548684 ) ) ;
#17030 = CARTESIAN_POINT ( 'NONE',  ( -25.21435515916025594, 1.749597353048488237E-16, -4.373993382621220594E-17 ) ) ;
#17031 = CARTESIAN_POINT ( 'NONE',  ( -22.34422965417126505, 5.100074259623119666, 37.57019010019537575 ) ) ;
#17032 = LINE ( 'NONE', #19613, #26773 ) ;
#17033 = CIRCLE ( 'NONE', #26682, 34.60786435723138510 ) ;
#17034 = CARTESIAN_POINT ( 'NONE',  ( 30.59138290137916627, 84.53179630244103748, -79.74792615266086671 ) ) ;
#17035 = CARTESIAN_POINT ( 'NONE',  ( 25.98552792386800192, 102.9121737515627188, -47.00040718953673036 ) ) ;
#17036 = CARTESIAN_POINT ( 'NONE',  ( 26.04756280548354397, 113.1727782765313890, -1.110889087302899592 ) ) ;
#17037 = CARTESIAN_POINT ( 'NONE',  ( -20.21097721650786738, -17.13687097598118925, 24.14932365326971464 ) ) ;
#17038 = ORIENTED_EDGE ( 'NONE', *, *, #24952, .T. ) ;
#17039 = VERTEX_POINT ( 'NONE', #17274 ) ;
#17041 = CARTESIAN_POINT ( 'NONE',  ( -25.21435515916043713, -23.92354251275918031, 25.00736669481048224 ) ) ;
#17040 = CARTESIAN_POINT ( 'NONE',  ( 8.186469777910764023, -12.15801985874078284, 148.8557359139591938 ) ) ;
#17042 = CARTESIAN_POINT ( 'NONE',  ( 25.64681081121880624, 23.06870491922473931, -110.5293738517606243 ) ) ;
#17043 = CARTESIAN_POINT ( 'NONE',  ( 2.063896406836605024, -116.7302989755731772, -86.47093297169119808 ) ) ;
#17044 = CARTESIAN_POINT ( 'NONE',  ( 26.11404676487257603, 112.7148551500681890, -10.71016160607451262 ) ) ;
#17045 = B_SPLINE_CURVE_WITH_KNOTS ( 'NONE', 3,
 ( #24423, #26422, #24578, #4692, #2522, #11311 ),
 .UNSPECIFIED., .F., .F.,
 ( 4, 2, 4 ),
 ( 1.491862189340054101E-16, 0.003570751334075637860, 0.007141502668151126533 ),
 .UNSPECIFIED. ) ;
#17046 = VERTEX_POINT ( 'NONE', #21751 ) ;
#17047 = CARTESIAN_POINT ( 'NONE',  ( 25.64692872815577473, 91.53575854059506867, -66.10702795113321883 ) ) ;
#17048 = CARTESIAN_POINT ( 'NONE',  ( -7.711401346138400115, 25.75361633141491424, -45.70592430511727144 ) ) ;
#17049 = CARTESIAN_POINT ( 'NONE',  ( -1.019300379054419725, -28.53917295602924042, -35.83762006677390133 ) ) ;
#17050 = ORIENTED_EDGE ( 'NONE', *, *, #20269, .T. ) ;
#17051 = ORIENTED_EDGE ( 'NONE', *, *, #4056, .T. ) ;
#17052 = DIRECTION ( 'NONE',  ( -1.000000000000000000, 6.938893903907226837E-18, -1.734723475976806709E-18 ) ) ;
#17053 = EDGE_CURVE ( 'NONE', #21599, #3668, #27546, .T. ) ;
#17054 = VERTEX_POINT ( 'NONE', #22615 ) ;
#17055 = EDGE_LOOP ( 'NONE', ( #16797, #6109, #10204, #7949 ) ) ;
#17056 = EDGE_CURVE ( 'NONE', #10267, #15546, #8358, .T. ) ;
#17057 = B_SPLINE_CURVE_WITH_KNOTS ( 'NONE', 3,
 ( #10588, #8437, #17202, #25990, #27572, #6279, #4103, #5721 ),
 .UNSPECIFIED., .F., .F.,
 ( 4, 2, 2, 4 ),
 ( 0.000000000000000000, 0.002761524886576655416, 0.005523049773153310832, 0.01104609954630661646 ),
 .UNSPECIFIED. ) ;
#17058 = AXIS2_PLACEMENT_3D ( 'NONE', #13170, #2086, #22103 ) ;
#17059 = EDGE_CURVE ( 'NONE', #15152, #7370, #16119, .T. ) ;
#17060 = B_SPLINE_CURVE_WITH_KNOTS ( 'NONE', 3,
 ( #16406, #10500, #19000, #28041 ),
 .UNSPECIFIED., .F., .F.,
 ( 4, 4 ),
 ( 3.625240045095802037E-16, 0.01077107486149760443 ),
 .UNSPECIFIED. ) ;
#17061 = EDGE_CURVE ( 'NONE', #10330, #28326, #19783, .T. ) ;
#17062 = LINE ( 'NONE', #1658, #10593 ) ;
#17063 = VECTOR ( 'NONE', #25467, 1000.000000000000227 ) ;
#17064 = ORIENTED_EDGE ( 'NONE', *, *, #13583, .T. ) ;
#17065 = CARTESIAN_POINT ( 'NONE',  ( -55.24271866751342941, 0.001545935011631005204, -0.009369360294295841357 ) ) ;
#17066 = CONTEXT_DEPENDENT_SHAPE_REPRESENTATION ( #10488, #20273 ) ;
#17067 = CARTESIAN_POINT ( 'NONE',  ( 32.73300124599735739, -72.21147546950616913, 92.86301839379999024 ) ) ;
#17068 = B_SPLINE_CURVE_WITH_KNOTS ( 'NONE', 3,
 ( #2576, #11359, #20132, #13656, #22456, #17691 ),
 .UNSPECIFIED., .F., .F.,
 ( 4, 2, 4 ),
 ( 3.476216610979977084E-18, 0.0006311571484585997175, 0.001262314296917196616 ),
 .UNSPECIFIED. ) ;
#17069 = CARTESIAN_POINT ( 'NONE',  ( 25.98552792386800192, -110.8838436908324638, -22.46612985365086246 ) ) ;
#17070 = CARTESIAN_POINT ( 'NONE',  ( 25.73574536432415627, 55.78561308781485195, 98.23578516674979255 ) ) ;
#17071 = CARTESIAN_POINT ( 'NONE',  ( 109.1589550718175161, 0.007571935245608774762, -0.0002241941239326223723 ) ) ;
#17072 = CARTESIAN_POINT ( 'NONE',  ( -1.619063947482197729, -2.489035965909835557, 46.30105812165550816 ) ) ;
#17074 = CARTESIAN_POINT ( 'NONE',  ( -1.058473599757816297, 45.77379534793244886, -1.755404039369589997 ) ) ;
#17073 = CARTESIAN_POINT ( 'NONE',  ( 1.833838850093440165, 85.29337590730699503, -117.3962664098815338 ) ) ;
#17075 = DIRECTION ( 'NONE',  ( -1.000000000000000000, -0.000000000000000000, -0.000000000000000000 ) ) ;
#17076 = ORIENTED_EDGE ( 'NONE', *, *, #28005, .T. ) ;
#17077 = VERTEX_POINT ( 'NONE', #5177 ) ;
#17078 = LINE ( 'NONE', #12335, #17063 ) ;
#17079 = CARTESIAN_POINT ( 'NONE',  ( -1.044557008772710294, 25.56990300677035677, 37.98985164565299755 ) ) ;
#17080 = CIRCLE ( 'NONE', #14781, 151.1787379149930359 ) ;
#17081 = CARTESIAN_POINT ( 'NONE',  ( 1.833485406944057594, 125.4007332306555895, -73.01664920992834595 ) ) ;
#17082 = CARTESIAN_POINT ( 'NONE',  ( 26.04756280548354042, -90.90573670389279926, 67.42001818240436251 ) ) ;
#17083 = ORIENTED_EDGE ( 'NONE', *, *, #7829, .F. ) ;
#17084 = CARTESIAN_POINT ( 'NONE',  ( -20.90916690077964546, -17.17795951644681907, -35.64494649500676360 ) ) ;
#17085 = CARTESIAN_POINT ( 'NONE',  ( 1.834118845439484335, 125.5799175751969727, 72.70910183320610543 ) ) ;
#17086 = ORIENTED_EDGE ( 'NONE', *, *, #9161, .T. ) ;
#17087 = CARTESIAN_POINT ( 'NONE',  ( -55.24271866751342941, 0.001545935011631000867, -0.009369360294295843092 ) ) ;
#17088 = CARTESIAN_POINT ( 'NONE',  ( 1.834118845439484335, 141.9019470378987933, 30.34413640949744106 ) ) ;
#17089 = EDGE_CURVE ( 'NONE', #27834, #4666, #20286, .T. ) ;
#17090 = CARTESIAN_POINT ( 'NONE',  ( 109.1589550718174877, -0.005477029346537810178, -0.005233222325298206822 ) ) ;
#17091 = CARTESIAN_POINT ( 'NONE',  ( 8.186469777910810208, -108.6390983781763708, 102.4860666868859340 ) ) ;
#17092 = CARTESIAN_POINT ( 'NONE',  ( 5.340103556456523570, 111.1041836730292260, -96.93942141425958425 ) ) ;
#17093 = ORIENTED_EDGE ( 'NONE', *, *, #17344, .F. ) ;
#17094 = CARTESIAN_POINT ( 'NONE',  ( -55.24340739397742084, -0.0007387096945734077319, 0.01010924026184317238 ) ) ;
#17095 = EDGE_CURVE ( 'NONE', #19279, #18758, #9005, .T. ) ;
#17096 = ADVANCED_FACE ( 'NONE', ( #16262 ), #4521, .F. ) ;
#17097 = CARTESIAN_POINT ( 'NONE',  ( 2.430230287190592531, 116.8646894862423835, -86.70145658344540607 ) ) ;
#17098 = ORIENTED_EDGE ( 'NONE', *, *, #3773, .T. ) ;
#17099 = CARTESIAN_POINT ( 'NONE',  ( 10.93730112725997294, 36.23586118136742584, -146.7718404940639516 ) ) ;
#17100 = CARTESIAN_POINT ( 'NONE',  ( -1.619063947482197729, -35.99532424477401094, -29.22875152547743838 ) ) ;
#17101 = CARTESIAN_POINT ( 'NONE',  ( -20.20700224038492365, -8.199606986804534259, -28.44216453106533748 ) ) ;
#17102 = CARTESIAN_POINT ( 'NONE',  ( 119.2224693531408803, -90.00000000000000000, 19.99999999999990052 ) ) ;
#17103 = AXIS2_PLACEMENT_3D ( 'NONE', #17933, #2990, #11770 ) ;
#17104 = CARTESIAN_POINT ( 'NONE',  ( 2.433796855181205476, 125.2830755159753977, 74.00833731765604284 ) ) ;
#17105 = CARTESIAN_POINT ( 'NONE',  ( -20.57838717382308147, 23.26537097894132344, 18.89542499756474569 ) ) ;
#17106 = VECTOR ( 'NONE', #5230, 1000.000000000000000 ) ;
#17107 = DIRECTION ( 'NONE',  ( 0.000000000000000000, 5.223019709707975211E-21, -1.000000000000000000 ) ) ;
#17108 = CARTESIAN_POINT ( 'NONE',  ( -22.23226125620943705, -11.82389163795231468, -29.33577758406444858 ) ) ;
#17109 = CARTESIAN_POINT ( 'NONE',  ( -55.24390624410018802, -0.009209468562452135382, -0.004896917417131697002 ) ) ;
#17110 = FACE_OUTER_BOUND ( 'NONE', #3109, .T. ) ;
#17111 = CARTESIAN_POINT ( 'NONE',  ( -22.34422965417123663, -6.759368364654068095, 37.30738373203626423 ) ) ;
#17112 = DIRECTION ( 'NONE',  ( -0.5946245182733607137, 0.5357871896547532486, -0.5994612328333126516 ) ) ;
#17113 = CARTESIAN_POINT ( 'NONE',  ( 2.433796855181219243, -144.8571464219890004, 13.76554153471645847 ) ) ;
#17114 = ORIENTED_EDGE ( 'NONE', *, *, #18432, .F. ) ;
#17115 = EDGE_LOOP ( 'NONE', ( #13575, #26342, #2204, #6740 ) ) ;
#17116 = ORIENTED_EDGE ( 'NONE', *, *, #25018, .T. ) ;
#17117 = CARTESIAN_POINT ( 'NONE',  ( -25.21435515916043713, 34.05351380035342146, 6.169479169075106739 ) ) ;
#17118 = CARTESIAN_POINT ( 'NONE',  ( 10.93730112725983439, -146.7718404940644916, 36.23586118136483236 ) ) ;
#17119 = CARTESIAN_POINT ( 'NONE',  ( 1.834118845439484335, -85.43746956709928497, 117.2918069668798040 ) ) ;
#17120 = B_SPLINE_CURVE_WITH_KNOTS ( 'NONE', 3,
 ( #15378, #25680, #26189, #17542 ),
 .UNSPECIFIED., .F., .F.,
 ( 4, 4 ),
 ( 1.892757412642747523E-16, 0.001982023823822947652 ),
 .UNSPECIFIED. ) ;
#17121 = CARTESIAN_POINT ( 'NONE',  ( 55.79472521941426777, 58.42842213658327921, 43.35047097963469298 ) ) ;
#17122 = CARTESIAN_POINT ( 'NONE',  ( 16.05277956358206737, 141.9568301782832123, -19.61822947415828722 ) ) ;
#17123 = CARTESIAN_POINT ( 'NONE',  ( 109.1586059443104944, 0.007001002073871745619, 0.001014167950280808750 ) ) ;
#17124 = CARTESIAN_POINT ( 'NONE',  ( 2.108393763691180922, 98.16799842733396986, -107.1124103264139364 ) ) ;
#17125 = ORIENTED_EDGE ( 'NONE', *, *, #14451, .F. ) ;
#17126 = FACE_OUTER_BOUND ( 'NONE', #24552, .T. ) ;
#17127 = CARTESIAN_POINT ( 'NONE',  ( -55.24271866751342941, -0.001425019990778742711, -0.009388511352200234680 ) ) ;
#17128 = CARTESIAN_POINT ( 'NONE',  ( 1.831572820252008738, -0.9871191512924697431, 145.1082523917587253 ) ) ;
#17129 = ADVANCED_FACE ( 'NONE', ( #24486 ), #5649, .F. ) ;
#17130 = EDGE_CURVE ( 'NONE', #8996, #5673, #429, .T. ) ;
#17131 = LINE ( 'NONE', #27646, #17163 ) ;
#17132 = AXIS2_PLACEMENT_3D ( 'NONE', #11474, #9609, #20248 ) ;
#17133 = AXIS2_PLACEMENT_3D ( 'NONE', #12481, #5591, #21115 ) ;
#17134 = ORIENTED_EDGE ( 'NONE', *, *, #11089, .T. ) ;
#17136 = ADVANCED_FACE ( 'NONE', ( #25061 ), #8739, .F. ) ;
#17135 = CARTESIAN_POINT ( 'NONE',  ( -6.588769196390753535, -38.42957692275866322, -34.04709086065298607 ) ) ;
#17137 = DIRECTION ( 'NONE',  ( 0.5946245182733607137, 0.8039981203473692828, 0.002950380665393250324 ) ) ;
#17138 = ORIENTED_EDGE ( 'NONE', *, *, #15674, .F. ) ;
#17139 = ADVANCED_FACE ( 'NONE', ( #18257 ), #8568, .F. ) ;
#17140 = ORIENTED_EDGE ( 'NONE', *, *, #1377, .T. ) ;
#17141 = ORIENTED_EDGE ( 'NONE', *, *, #287, .F. ) ;
#17142 = B_SPLINE_CURVE_WITH_KNOTS ( 'NONE', 3,
 ( #12795, #23347, #19012, #19561, #21160, #1445, #10251, #21729 ),
 .UNSPECIFIED., .F., .F.,
 ( 4, 2, 2, 4 ),
 ( 1.551583845779545699E-17, 0.0002429592666046831570, 0.0004859185332093508098, 0.0009718370664186806946 ),
 .UNSPECIFIED. ) ;
#17143 = CARTESIAN_POINT ( 'NONE',  ( 1.832998868059890096, -117.0819875546701070, 85.72499093308064744 ) ) ;
#17144 = FACE_OUTER_BOUND ( 'NONE', #150, .T. ) ;
#17145 = CONICAL_SURFACE ( 'NONE', #11164, 53.53553390275978785, 0.7853981625000051592 ) ;
#17146 = CARTESIAN_POINT ( 'NONE',  ( 1.832998868059858122, -58.53348008137559333, -132.7810136645744024 ) ) ;
#17148 =( BOUNDED_SURFACE ( )  B_SPLINE_SURFACE ( 3, 1, ( 
 ( #4619, #9230 ),
 ( #27053, #591 ),
 ( #9389, #17988 ),
 ( #18140, #6938 ) ),
 .UNSPECIFIED., .F., .F., .F. ) 
 B_SPLINE_SURFACE_WITH_KNOTS ( ( 4, 4 ),
 ( 2, 2 ),
 ( 0.000000000000000000, 1.000000000000000000 ),
 ( 0.000000000000000000, 1.000000000000000000 ),
 .UNSPECIFIED. ) 
 GEOMETRIC_REPRESENTATION_ITEM ( )  RATIONAL_B_SPLINE_SURFACE ( (
 ( 1.000000000000000000, 1.000000000000000000),
 ( 0.6386103224230316178, 0.9954351624131538845),
 ( 0.6386103224230316178, 0.9954351624131538845),
 ( 1.000000000000000000, 1.000000000000000000) ) ) 
 REPRESENTATION_ITEM ( '' )  SURFACE ( )  );
#17147 = VECTOR ( 'NONE', #3874, 1000.000000000000000 ) ;
#17149 = VECTOR ( 'NONE', #13209, 1000.000000000000114 ) ;
#17150 = CARTESIAN_POINT ( 'NONE',  ( 13.36082413113063083, -6.345145185216972905, -152.7944199136427983 ) ) ;
#17151 = ORIENTED_EDGE ( 'NONE', *, *, #13237, .F. ) ;
#17152 = CARTESIAN_POINT ( 'NONE',  ( 2.430230287190581429, -43.58368230469295668, -138.8342928068224467 ) ) ;
#17153 = CARTESIAN_POINT ( 'NONE',  ( -8.786685647604894456, -23.24040270374358030, 48.22796981442792230 ) ) ;
#17154 = B_SPLINE_CURVE_WITH_KNOTS ( 'NONE', 3,
 ( #24347, #8654, #17841, #2154, #15682, #292 ),
 .UNSPECIFIED., .F., .F.,
 ( 4, 2, 4 ),
 ( 1.392007502815792650E-17, 0.0006311571484586138122, 0.001262314296917213963 ),
 .UNSPECIFIED. ) ;
#17155 = CARTESIAN_POINT ( 'NONE',  ( -1.049819078601898825, -0.5100232645223283789, -45.79653735114490587 ) ) ;
#17156 = CARTESIAN_POINT ( 'NONE',  ( -5.986830583229505898, 43.56094206392996426, 26.01297580803277754 ) ) ;
#17157 = FACE_OUTER_BOUND ( 'NONE', #6872, .T. ) ;
#17158 = EDGE_CURVE ( 'NONE', #23320, #12154, #4204, .T. ) ;
#17159 = CARTESIAN_POINT ( 'NONE',  ( 1.832998868059890096, 85.72499093308101692, 117.0819875546698512 ) ) ;
#17160 = CARTESIAN_POINT ( 'NONE',  ( 13.36082413113063083, -117.7941133658631827, -97.52406103376877411 ) ) ;
#17161 = CARTESIAN_POINT ( 'NONE',  ( 109.1721716018069515, -0.01368917435590581710, -0.01019541462303050379 ) ) ;
#17162 = ORIENTED_EDGE ( 'NONE', *, *, #1648, .F. ) ;
#17163 = VECTOR ( 'NONE', #23784, 999.9999999999998863 ) ;
#17164 = ORIENTED_EDGE ( 'NONE', *, *, #14128, .T. ) ;
#17166 = EDGE_CURVE ( 'NONE', #15111, #27426, #4551, .T. ) ;
#17165 = CARTESIAN_POINT ( 'NONE',  ( -1.619063947482197729, 38.92136151114943488, 25.20140673341330739 ) ) ;
#17168 = ORIENTED_EDGE ( 'NONE', *, *, #19225, .T. ) ;
#17167 = CARTESIAN_POINT ( 'NONE',  ( 32.73300124599732186, 0.000000000000000000, 0.000000000000000000 ) ) ;
#17169 = ORIENTED_EDGE ( 'NONE', *, *, #9975, .T. ) ;
#17170 = ORIENTED_EDGE ( 'NONE', *, *, #5128, .F. ) ;
#17171 = CIRCLE ( 'NONE', #16723, 37.50000000000001421 ) ;
#17172 = ORIENTED_EDGE ( 'NONE', *, *, #20174, .F. ) ;
#17173 = FACE_OUTER_BOUND ( 'NONE', #62, .T. ) ;
#17174 =( BOUNDED_SURFACE ( )  B_SPLINE_SURFACE ( 3, 1, ( 
 ( #477, #24825 ),
 ( #9269, #15881 ),
 ( #18029, #26816 ),
 ( #906, #4940 ) ),
 .UNSPECIFIED., .F., .F., .F. ) 
 B_SPLINE_SURFACE_WITH_KNOTS ( ( 4, 4 ),
 ( 2, 2 ),
 ( 0.000000000000000000, 1.000000000000000000 ),
 ( 0.000000000000000000, 1.000000000000000000 ),
 .UNSPECIFIED. ) 
 GEOMETRIC_REPRESENTATION_ITEM ( )  RATIONAL_B_SPLINE_SURFACE ( (
 ( 1.000000000000000000, 1.000000000000000000),
 ( 0.9960225298536222738, 0.9999952330161893110),
 ( 0.9960225298536222738, 0.9999952330161893110),
 ( 1.000000000000000000, 1.000000000000000000) ) ) 
 REPRESENTATION_ITEM ( '' )  SURFACE ( )  );
#17175 = CARTESIAN_POINT ( 'NONE',  ( -20.20700224038492721, 27.82980252387819675, -10.08426345511598932 ) ) ;
#17176 = CARTESIAN_POINT ( 'NONE',  ( -1.619063947482197729, -46.30105812165550105, -2.489035965909997206 ) ) ;
#17177 = CARTESIAN_POINT ( 'NONE',  ( -8.786685647604887350, 53.04920435127183254, 7.199674155859139724 ) ) ;
#17178 = B_SPLINE_CURVE_WITH_KNOTS ( 'NONE', 3,
 ( #20489, #26956, #11287, #22076, #22380, #26532 ),
 .UNSPECIFIED., .F., .F.,
 ( 4, 2, 4 ),
 ( 3.106877759296670001E-17, 0.0006311571484586191248, 0.001262314296917207024 ),
 .UNSPECIFIED. ) ;
#17179 = CARTESIAN_POINT ( 'NONE',  ( -8.786685647604898008, 48.22796981442802178, 23.24040270374343464 ) ) ;
#17180 = CARTESIAN_POINT ( 'NONE',  ( 13.36082413113061307, -143.3553710183985572, -53.25066407421950743 ) ) ;
#17181 = CARTESIAN_POINT ( 'NONE',  ( 99.22246935314079508, 90.00000000000005684, 39.99999999999999289 ) ) ;
#17182 = ORIENTED_EDGE ( 'NONE', *, *, #12447, .T. ) ;
#17183 = ORIENTED_EDGE ( 'NONE', *, *, #16727, .T. ) ;
#17185 = CARTESIAN_POINT ( 'NONE',  ( 1.833838850093517214, 1.355257560975019971E-17, -145.1097630783160923 ) ) ;
#17184 = CARTESIAN_POINT ( 'NONE',  ( -1.619063947482197729, -38.92136151114925724, -25.20140673341360227 ) ) ;
#17186 = ADVANCED_FACE ( 'NONE', ( #5909 ), #13340, .F. ) ;
#17187 = CARTESIAN_POINT ( 'NONE',  ( -12.94347594948487057, -47.96504705787739198, 8.691477019903814494 ) ) ;
#17188 = CARTESIAN_POINT ( 'NONE',  ( 25.87036335909427009, 10.83311869338221278, -112.5399073133627326 ) ) ;
#17189 = CARTESIAN_POINT ( 'NONE',  ( 25.73574536432415627, 112.4329083163019760, -11.00659994954035525 ) ) ;
#17190 = ORIENTED_EDGE ( 'NONE', *, *, #24530, .T. ) ;
#17191 = CARTESIAN_POINT ( 'NONE',  ( -1.583189561560256253, -16.68617981233733261, -43.29471907393735819 ) ) ;
#17192 = MANIFOLD_SOLID_BREP ( 'Boss-Extrude1', #11412 ) ;
#17194 = EDGE_CURVE ( 'NONE', #19755, #20942, #2466, .T. ) ;
#17193 = CARTESIAN_POINT ( 'NONE',  ( -8.786685647604890903, -25.35688121747466184, 47.14957014837381166 ) ) ;
#17195 = CARTESIAN_POINT ( 'NONE',  ( -1.050230346682690108, -37.05182464822001975, -26.92058491724852942 ) ) ;
#17196 = VERTEX_POINT ( 'NONE', #14225 ) ;
#17197 = ORIENTED_EDGE ( 'NONE', *, *, #11335, .F. ) ;
#17198 = ADVANCED_FACE ( 'NONE', ( #20868 ), #19324, .T. ) ;
#17199 = CARTESIAN_POINT ( 'NONE',  ( -2.265401668238153032, -11.98901689611074062, -45.46007138824035820 ) ) ;
#17200 = VERTEX_POINT ( 'NONE', #8752 ) ;
#17201 = EDGE_LOOP ( 'NONE', ( #208, #26853, #18400, #17623 ) ) ;
#17202 = CARTESIAN_POINT ( 'NONE',  ( -7.711401346138401891, 35.51061203065580685, 38.61705198405327621 ) ) ;
#17203 = VERTEX_POINT ( 'NONE', #26166 ) ;
#17204 = CARTESIAN_POINT ( 'NONE',  ( 16.75465622695656265, 138.0797984721905038, 34.09043808962460531 ) ) ;
#17205 = ADVANCED_FACE ( 'NONE', ( #10783 ), #7496, .F. ) ;
#17206 = CARTESIAN_POINT ( 'NONE',  ( 16.75465622695648804, -87.30527857298524452, 112.2763423369178213 ) ) ;
#17207 = CARTESIAN_POINT ( 'NONE',  ( 1.831572820252009626, 14.18623102066960229, -144.4165162501761301 ) ) ;
#17208 = CARTESIAN_POINT ( 'NONE',  ( -1.019300379054419947, 45.76814864815091255, 2.023851374322834573 ) ) ;
#17209 = CARTESIAN_POINT ( 'NONE',  ( -55.24728320129491266, 0.01402509393918583563, -0.003868537197317189515 ) ) ;
#17210 = CARTESIAN_POINT ( 'NONE',  ( 55.49584447822657296, 62.96491934285994319, 36.04376091928565273 ) ) ;
#17211 = ORIENTED_EDGE ( 'NONE', *, *, #3188, .T. ) ;
#17212 = EDGE_CURVE ( 'NONE', #26877, #22293, #21984, .T. ) ;
#17213 = DIRECTION ( 'NONE',  ( 0.7563875759206387661, 0.6320336713238499105, -0.1685564395263362270 ) ) ;
#17214 = CARTESIAN_POINT ( 'NONE',  ( 109.1587776205901861, -0.0008489206734501101009, -0.007280006032835104751 ) ) ;
#17215 = DIRECTION ( 'NONE',  ( 0.000000000000000000, 5.223019709707975211E-21, -1.000000000000000000 ) ) ;
#17216 = ORIENTED_EDGE ( 'NONE', *, *, #3479, .F. ) ;
#17217 = ORIENTED_EDGE ( 'NONE', *, *, #14999, .T. ) ;
#17218 = CARTESIAN_POINT ( 'NONE',  ( 8.186469777910783563, -97.33125097303785367, 113.2805152945353058 ) ) ;
#17219 = CARTESIAN_POINT ( 'NONE',  ( 1.833206310202321943, 117.8322271314364400, 84.68961945193495922 ) ) ;
#17221 = CARTESIAN_POINT ( 'NONE',  ( 25.98107933586715390, -98.51796269673099005, 55.61918067932703025 ) ) ;
#17220 = LINE ( 'NONE', #12892, #7978 ) ;
#17222 = EDGE_CURVE ( 'NONE', #7617, #1094, #22044, .T. ) ;
#17223 = DIRECTION ( 'NONE',  ( 0.000000000000000000, 5.223019709707975211E-21, -1.000000000000000000 ) ) ;
#17224 = B_SPLINE_CURVE_WITH_KNOTS ( 'NONE', 3,
 ( #16302, #20478, #760, #11986, #9545, #11845, #3072 ),
 .UNSPECIFIED., .F., .F.,
 ( 4, 3, 4 ),
 ( 1.201851678989727385E-17, 0.009512539173626329003, 0.02506242213020845599 ),
 .UNSPECIFIED. ) ;
#17225 = CARTESIAN_POINT ( 'NONE',  ( 25.64681081121879203, -91.10197563707990298, 66.70335573067838197 ) ) ;
#17226 = CARTESIAN_POINT ( 'NONE',  ( -24.53239521893647890, -29.54733954334097135, 16.68574937151005599 ) ) ;
#17227 = VERTEX_POINT ( 'NONE', #14937 ) ;
#17228 = CARTESIAN_POINT ( 'NONE',  ( 32.73300124599738581, 16.10546300444979195, -116.5274707358853163 ) ) ;
#17229 = CARTESIAN_POINT ( 'NONE',  ( 109.1586059443104944, -0.006808232911146201889, -0.001921075557418339087 ) ) ;
#17230 = CARTESIAN_POINT ( 'NONE',  ( 109.1586059443104944, -0.007058870754606105975, -0.0004635842312795806770 ) ) ;
#17231 = CARTESIAN_POINT ( 'NONE',  ( 10.93730112725990011, -151.0983828010091656, -4.928439153521871674 ) ) ;
#17232 = CARTESIAN_POINT ( 'NONE',  ( 1.833691583653551005, 117.1866391460185497, 85.58103979054524757 ) ) ;
#17233 = VERTEX_POINT ( 'NONE', #4422 ) ;
#17234 = CARTESIAN_POINT ( 'NONE',  ( 14.74894986621300319, 4.541450660883840889E-15, -37.50000000000001421 ) ) ;
#17235 = CARTESIAN_POINT ( 'NONE',  ( 109.1587776205901577, 0.003057017121591207136, -0.006661366261224509200 ) ) ;
#17236 = ORIENTED_EDGE ( 'NONE', *, *, #13806, .F. ) ;
#17237 = CARTESIAN_POINT ( 'NONE',  ( 32.73300124599732186, 0.000000000000000000, 0.000000000000000000 ) ) ;
#17238 = CARTESIAN_POINT ( 'NONE',  ( 13.36082413113061307, -56.35051087434871420, -142.1654513177093691 ) ) ;
#17239 = CARTESIAN_POINT ( 'NONE',  ( -28.41354790283022069, -12.60397206714818097, 19.47297445639563307 ) ) ;
#17240 = CARTESIAN_POINT ( 'NONE',  ( -20.57838717382308502, 23.26537097894105699, -18.89542499756508320 ) ) ;
#17241 = CARTESIAN_POINT ( 'NONE',  ( -1.323439229708149867, 35.86372896917474407, -28.92147054731853828 ) ) ;
#17242 = CARTESIAN_POINT ( 'NONE',  ( 25.64681081121879203, 46.30456157731467925, -102.9795863647023850 ) ) ;
#17243 = CARTESIAN_POINT ( 'NONE',  ( -20.20700224038492721, 28.44216453106548315, 8.199606986804035103 ) ) ;
#17244 = CARTESIAN_POINT ( 'NONE',  ( 32.73300124599735739, 20.69176323058628597, 115.8010721414084543 ) ) ;
#17245 = CARTESIAN_POINT ( 'NONE',  ( 1.833603222531958288, -132.7445893798462180, 58.61467103263697709 ) ) ;
#17246 = CARTESIAN_POINT ( 'NONE',  ( 25.64681081121879203, 110.5293738517608375, 23.06870491922360245 ) ) ;
#17247 = ADVANCED_FACE ( 'NONE', ( #6601 ), #11052, .T. ) ;
#17248 = CARTESIAN_POINT ( 'NONE',  ( -7.078251931573400491, -11.16394717458712726, -50.86685171665407523 ) ) ;
#17249 = CARTESIAN_POINT ( 'NONE',  ( 9.884929003653608603, -4.203795436553416920, 150.4771565009630194 ) ) ;
#17250 = CARTESIAN_POINT ( 'NONE',  ( 94.22246935314088034, -151.1871800109700246, -12.50000000000000888 ) ) ;
#17251 = VERTEX_POINT ( 'NONE', #25900 ) ;
#17252 = EDGE_CURVE ( 'NONE', #12494, #18677, #1836, .T. ) ;
#17253 = ORIENTED_EDGE ( 'NONE', *, *, #16970, .F. ) ;
#17254 = EDGE_LOOP ( 'NONE', ( #4815, #18661, #2206, #22839 ) ) ;
#17255 = CARTESIAN_POINT ( 'NONE',  ( -1.048994561756789512, -43.78680886990931498, 13.42228657661168789 ) ) ;
#17256 = CARTESIAN_POINT ( 'NONE',  ( -1.323439229708132547, 16.42345129173398632, 43.04565903621268319 ) ) ;
#17257 = CARTESIAN_POINT ( 'NONE',  ( -4.162674018437125589, -31.44946543094270197, 37.46098494546626512 ) ) ;
#17258 = PLANE ( 'NONE',  #2308 ) ;
#17259 = CARTESIAN_POINT ( 'NONE',  ( -1.058473599757830730, 42.99101666105228503, -15.81436910992533029 ) ) ;
#17260 = CARTESIAN_POINT ( 'NONE',  ( 109.1586059443104944, 0.006808232911146188011, 0.001921075557418385491 ) ) ;
#17261 = VERTEX_POINT ( 'NONE', #15486 ) ;
#17262 = CARTESIAN_POINT ( 'NONE',  ( -7.711401346138401891, 52.11446537925913702, -6.030154970217080468 ) ) ;
#17263 = CARTESIAN_POINT ( 'NONE',  ( -20.47566262905009538, -18.81547655725230328, 23.19796652405694459 ) ) ;
#17264 = CARTESIAN_POINT ( 'NONE',  ( -25.21435515916043713, -30.48034229288650820, -16.39063784838731053 ) ) ;
#17265 = CARTESIAN_POINT ( 'NONE',  ( 2.433796855181205476, 46.34326152018925171, -137.9325382748280333 ) ) ;
#17266 = ORIENTED_EDGE ( 'NONE', *, *, #6226, .T. ) ;
#17267 = CARTESIAN_POINT ( 'NONE',  ( 25.64681081121879203, -112.3352186517029878, -11.38886654529789233 ) ) ;
#17268 = B_SPLINE_CURVE_WITH_KNOTS ( 'NONE', 3,
 ( #2908, #16136, #12118, #597, #22929, #9666, #1031, #26921 ),
 .UNSPECIFIED., .F., .F.,
 ( 4, 2, 2, 4 ),
 ( 2.214340075454938295E-16, 0.002761568181852865067, 0.005523136363705506355, 0.01104627272741079066 ),
 .UNSPECIFIED. ) ;
#17269 = CARTESIAN_POINT ( 'NONE',  ( -6.574463467970653952, -11.01561683920017387, 50.12924290857549181 ) ) ;
#17270 = VERTEX_POINT ( 'NONE', #17105 ) ;
#17271 = ORIENTED_EDGE ( 'NONE', *, *, #10124, .T. ) ;
#17272 = ORIENTED_EDGE ( 'NONE', *, *, #23071, .T. ) ;
#17273 = CARTESIAN_POINT ( 'NONE',  ( 109.1589550718175161, -0.002126635388718581179, 0.007270618150635343134 ) ) ;
#17274 = CARTESIAN_POINT ( 'NONE',  ( 32.73300124599737160, -116.5274707358854158, -16.10546300444944023 ) ) ;
#17275 = ADVANCED_FACE ( 'NONE', ( #24029 ), #26237, .T. ) ;
#17276 = EDGE_CURVE ( 'NONE', #12851, #15929, #18636, .T. ) ;
#17277 = CARTESIAN_POINT ( 'NONE',  ( -8.786685647604890903, 37.00619870957935120, -38.68584556812312059 ) ) ;
#17278 = CARTESIAN_POINT ( 'NONE',  ( 109.1592201516379674, -0.007845213074660005795, -0.0005146241775907089413 ) ) ;
#17279 = ORIENTED_EDGE ( 'NONE', *, *, #27857, .T. ) ;
#17280 = EDGE_CURVE ( 'NONE', #14288, #23510, #22416, .T. ) ;
#17281 = B_SPLINE_CURVE_WITH_KNOTS ( 'NONE', 3,
 ( #1768, #23956, #25962, #5974 ),
 .UNSPECIFIED., .F., .F.,
 ( 4, 4 ),
 ( 6.118829799797332275E-16, 0.008383748772660060827 ),
 .UNSPECIFIED. ) ;
#17282 = ORIENTED_EDGE ( 'NONE', *, *, #14422, .T. ) ;
#17283 = CARTESIAN_POINT ( 'NONE',  ( -55.24340739397742794, -0.008612749836242414997, -0.005344433640974251970 ) ) ;
#17284 = CARTESIAN_POINT ( 'NONE',  ( 1.833485406944043827, -44.33323125129830089, -138.1714136985312962 ) ) ;
#17285 = FACE_OUTER_BOUND ( 'NONE', #16781, .T. ) ;
#17286 = CARTESIAN_POINT ( 'NONE',  ( 26.11404676487257603, 110.5078194225164481, -24.64483677384740545 ) ) ;
#17287 = EDGE_CURVE ( 'NONE', #12283, #17615, #4005, .T. ) ;
#17288 = CARTESIAN_POINT ( 'NONE',  ( -8.786685647604890903, -48.22796981442785835, -23.24040270374372952 ) ) ;
#17289 = CARTESIAN_POINT ( 'NONE',  ( 1.833838850093452599, 97.09738119087856489, -107.8375718686129687 ) ) ;
#17290 = CARTESIAN_POINT ( 'NONE',  ( -1.239374126674604337, 35.79060836339854745, 28.97829083655398819 ) ) ;
#17291 = CARTESIAN_POINT ( 'NONE',  ( -1.539763995773690164, -44.72359274866473555, 11.93465967526341842 ) ) ;
#17292 = CARTESIAN_POINT ( 'NONE',  ( 9.884929003653626367, 71.59798461011516224, -132.4189379373563042 ) ) ;
#17293 = DIRECTION ( 'NONE',  ( 0.5914120900931444380, 0.4804373588864810363, -0.6476200150380166942 ) ) ;
#17294 = ORIENTED_EDGE ( 'NONE', *, *, #22339, .F. ) ;
#17295 = EDGE_LOOP ( 'NONE', ( #122, #21317, #20703, #2022, #17164, #14871, #22734, #26314, #9199, #14064, #2314, #9375, #333, #480, #21462, #24197, #48, #14883, #20449, #22792, #19620, #17190, #27277, #26501, #19057, #26997, #5731, #15231, #16408, #18349, #15993, #18073, #11623, #25847, #8338, #26043, #20290, #13207, #15887, #19605, #8027, #23160, #23192, #6826, #14447, #16503, #19994, #14473, #4064, #10384, #9429, #9324, #9097, #2872, #3807, #27298, #25512, #16911, #12155, #9708, #27204, #25821, #5737, #16712 ) ) ;
#17296 = CARTESIAN_POINT ( 'NONE',  ( 2.433796855181233454, -144.8571464219888298, -13.76554153471842312 ) ) ;
#17297 = CARTESIAN_POINT ( 'NONE',  ( -1.049817751779888786, 45.79652915392415480, 0.5106138415328438374 ) ) ;
#17298 = ORIENTED_EDGE ( 'NONE', *, *, #9688, .T. ) ;
#17299 = ORIENTED_EDGE ( 'NONE', *, *, #10565, .T. ) ;
#17300 = ORIENTED_EDGE ( 'NONE', *, *, #12133, .T. ) ;
#17301 = B_SPLINE_CURVE_WITH_KNOTS ( 'NONE', 3,
 ( #13267, #20178, #22052, #20321, #2474, #24095, #6963, #615 ),
 .UNSPECIFIED., .F., .F.,
 ( 4, 2, 2, 4 ),
 ( 6.938893903907228378E-18, 0.0002429588503611284506, 0.0004859177007222499622, 0.0009718354014444875646 ),
 .UNSPECIFIED. ) ;
#17302 =( BOUNDED_SURFACE ( )  B_SPLINE_SURFACE ( 3, 1, ( 
 ( #21197, #17159 ),
 ( #16889, #4054 ),
 ( #23938, #21339 ),
 ( #19596, #6239 ) ),
 .UNSPECIFIED., .F., .F., .F. ) 
 B_SPLINE_SURFACE_WITH_KNOTS ( ( 4, 4 ),
 ( 2, 2 ),
 ( 0.000000000000000000, 1.000000000000000000 ),
 ( 0.000000000000000000, 1.000000000000000000 ),
 .UNSPECIFIED. ) 
 GEOMETRIC_REPRESENTATION_ITEM ( )  RATIONAL_B_SPLINE_SURFACE ( (
 ( 1.000000000000000000, 1.000000000000000000),
 ( 0.9960225298536222738, 0.9999952330161893110),
 ( 0.9960225298536222738, 0.9999952330161893110),
 ( 1.000000000000000000, 1.000000000000000000) ) ) 
 REPRESENTATION_ITEM ( '' )  SURFACE ( )  );
#17303 = EDGE_CURVE ( 'NONE', #14688, #10266, #10914, .T. ) ;
#17304 = EDGE_CURVE ( 'NONE', #17315, #24758, #26521, .T. ) ;
#17305 = CARTESIAN_POINT ( 'NONE',  ( 109.1586059443104944, -0.002622205828279790089, 0.006570129623063761248 ) ) ;
#17306 = CARTESIAN_POINT ( 'NONE',  ( -20.20700224038492721, 29.58392382092673500, 0.9908225410479544193 ) ) ;
#17307 = EDGE_CURVE ( 'NONE', #4802, #2974, #13474, .T. ) ;
#17308 = CARTESIAN_POINT ( 'NONE',  ( 119.2224693531408946, -69.99999999999998579, -19.99999999999998934 ) ) ;
#17309 = B_SPLINE_CURVE_WITH_KNOTS ( 'NONE', 3,
 ( #28335, #24468, #26052, #4733 ),
 .UNSPECIFIED., .F., .F.,
 ( 4, 4 ),
 ( 1.156367566894970741E-16, 0.008383748772659616738 ),
 .UNSPECIFIED. ) ;
#17310 = CARTESIAN_POINT ( 'NONE',  ( -15.02187109954785171, 45.93032478317463330, 6.234056423739666286 ) ) ;
#17311 = DIRECTION ( 'NONE',  ( 0.000000000000000000, 1.000000000000000000, 0.000000000000000000 ) ) ;
#17312 = CARTESIAN_POINT ( 'NONE',  ( -23.79223135445719350, 30.42557260166829636, 13.25822371132262845 ) ) ;
#17313 = CARTESIAN_POINT ( 'NONE',  ( 32.73300124599735739, -62.10906484417306928, 99.90245962373816724 ) ) ;
#17314 = EDGE_LOOP ( 'NONE', ( #25306, #23341, #2150, #1787 ) ) ;
#17315 = VERTEX_POINT ( 'NONE', #15790 ) ;
#17317 = CARTESIAN_POINT ( 'NONE',  ( 25.86096068574580187, -57.38862431273656739, 97.40497849554871834 ) ) ;
#17316 = CARTESIAN_POINT ( 'NONE',  ( 2.430230287190581429, 109.1043569252027083, -96.28466919683992842 ) ) ;
#17318 = CARTESIAN_POINT ( 'NONE',  ( 25.64700659047697329, -103.0567718204599004, -46.13293552475893478 ) ) ;
#17319 = CARTESIAN_POINT ( 'NONE',  ( -1.056502255334264895, -45.80535052436396626, 0.5104472526224692608 ) ) ;
#17320 = CARTESIAN_POINT ( 'NONE',  ( -20.20612091757421069, 10.22177757278315191, -27.77903622052259536 ) ) ;
#17321 = CARTESIAN_POINT ( 'NONE',  ( -1.619063947482201282, 38.92136151114908671, -25.20140673341387227 ) ) ;
#17322 = CARTESIAN_POINT ( 'NONE',  ( 25.64670758986456534, 91.05338785329436746, 66.76959937251481847 ) ) ;
#17323 = VERTEX_POINT ( 'NONE', #18088 ) ;
#17324 = CARTESIAN_POINT ( 'NONE',  ( -8.786685647604896232, -7.199674155858612146, 53.04920435127190359 ) ) ;
#17325 = LINE ( 'NONE', #23705, #20252 ) ;
#17326 = CARTESIAN_POINT ( 'NONE',  ( -1.045287976400379737, -25.66401692420040703, -37.92705037016734337 ) ) ;
#17327 = ORIENTED_EDGE ( 'NONE', *, *, #27023, .F. ) ;
#17328 = ORIENTED_EDGE ( 'NONE', *, *, #20953, .F. ) ;
#17329 = CARTESIAN_POINT ( 'NONE',  ( -55.24198130335446422, -0.001391250620104931938, 0.009190321388308853381 ) ) ;
#17330 = CARTESIAN_POINT ( 'NONE',  ( -25.21435515916043713, -4.655591116594118617, 34.29329011225960500 ) ) ;
#17331 = ORIENTED_EDGE ( 'NONE', *, *, #19990, .T. ) ;
#17332 = B_SPLINE_CURVE_WITH_KNOTS ( 'NONE', 3,
 ( #2749, #20158, #11248, #13680 ),
 .UNSPECIFIED., .F., .F.,
 ( 4, 4 ),
 ( 1.909141801897607538E-16, 0.001982023823822941146 ),
 .UNSPECIFIED. ) ;
#17333 = DIRECTION ( 'NONE',  ( 1.000000000000000000, -6.938893903907226837E-18, 1.734723475976806709E-18 ) ) ;
#17334 =( BOUNDED_SURFACE ( )  B_SPLINE_SURFACE ( 3, 1, ( 
 ( #28357, #12687 ),
 ( #6650, #8655 ),
 ( #15400, #13241 ),
 ( #19870, #160 ) ),
 .UNSPECIFIED., .F., .F., .F. ) 
 B_SPLINE_SURFACE_WITH_KNOTS ( ( 4, 4 ),
 ( 2, 2 ),
 ( 0.000000000000000000, 1.000000000000000000 ),
 ( 0.000000000000000000, 1.000000000000000000 ),
 .UNSPECIFIED. ) 
 GEOMETRIC_REPRESENTATION_ITEM ( )  RATIONAL_B_SPLINE_SURFACE ( (
 ( 1.000000000000000000, 1.000000000000000000),
 ( 0.9934239774497838349, 0.8357310067453913582),
 ( 0.9934239774497838349, 0.8357310067453913582),
 ( 1.000000000000000000, 1.000000000000000000) ) ) 
 REPRESENTATION_ITEM ( '' )  SURFACE ( )  );
#17335 = VERTEX_POINT ( 'NONE', #18222 ) ;
#17336 = CARTESIAN_POINT ( 'NONE',  ( 109.1624594426973260, -0.005372302061310809534, 0.01503296564240495792 ) ) ;
#17337 = EDGE_CURVE ( 'NONE', #5699, #23320, #9373, .T. ) ;
#17338 = CARTESIAN_POINT ( 'NONE',  ( -20.57838717382308147, -10.78122205916981358, 27.96569011373096814 ) ) ;
#17339 = EDGE_CURVE ( 'NONE', #25984, #25988, #24822, .T. ) ;
#17340 = CARTESIAN_POINT ( 'NONE',  ( 32.73300124599732186, 0.000000000000000000, 0.000000000000000000 ) ) ;
#17341 = CARTESIAN_POINT ( 'NONE',  ( -12.82751273423883553, -43.04932478553545394, -23.15139349681293623 ) ) ;
#17342 = CARTESIAN_POINT ( 'NONE',  ( -1.046935749540012450, 15.35946454248395376, -43.14401153755472507 ) ) ;
#17343 = CARTESIAN_POINT ( 'NONE',  ( 109.1592201516379674, 0.007780772729122757865, -0.001127733110588145750 ) ) ;
#17344 = EDGE_CURVE ( 'NONE', #1421, #26154, #24741, .T. ) ;
#17345 = CARTESIAN_POINT ( 'NONE',  ( 1.833485406944043827, 125.4007332306545379, 73.01664920993009389 ) ) ;
#17346 = CARTESIAN_POINT ( 'NONE',  ( -23.79223135445721837, -33.03345552685147624, -3.207301057648224596 ) ) ;
#17347 = CARTESIAN_POINT ( 'NONE',  ( -55.24390624410018802, -0.001451500391952595045, 0.01032895241566660592 ) ) ;
#17348 = ORIENTED_EDGE ( 'NONE', *, *, #28129, .F. ) ;
#17350 = ORIENTED_EDGE ( 'NONE', *, *, #11776, .T. ) ;
#17349 = B_SPLINE_CURVE_WITH_KNOTS ( 'NONE', 3,
 ( #22740, #13782, #5297, #20411, #7190, #22441, #17809, #9619 ),
 .UNSPECIFIED., .F., .F.,
 ( 4, 2, 2, 4 ),
 ( 0.000000000000000000, 0.002761524886576596435, 0.005523049773153192871, 0.01104609954630638054 ),
 .UNSPECIFIED. ) ;
#17351 = CARTESIAN_POINT ( 'NONE',  ( 25.98552792386798771, 83.35136888841337566, -76.50165414343481984 ) ) ;
#17352 = CARTESIAN_POINT ( 'NONE',  ( 1.832998868059890096, -15.69902610990469505, 144.2584710144579958 ) ) ;
#17353 = DIRECTION ( 'NONE',  ( 0.000000000000000000, 5.223019709707975211E-21, -1.000000000000000000 ) ) ;
#17354 = CARTESIAN_POINT ( 'NONE',  ( -20.20700224038492721, 10.08426345511588984, -27.82980252387822517 ) ) ;
#17355 = CARTESIAN_POINT ( 'NONE',  ( 25.64660436782575204, -91.00479974714259868, 66.83584345385861525 ) ) ;
#17356 = CARTESIAN_POINT ( 'NONE',  ( 25.81918753295378366, 90.88802830332049609, -67.18811037444338297 ) ) ;
#17357 = ORIENTED_EDGE ( 'NONE', *, *, #26216, .F. ) ;
#17358 = CARTESIAN_POINT ( 'NONE',  ( -55.24271866751342941, -0.004365563123935077734, -0.008433070970613952902 ) ) ;
#17359 = CARTESIAN_POINT ( 'NONE',  ( 1.832998868059858122, 30.69214149074210241, -141.8272129421605712 ) ) ;
#17360 = CARTESIAN_POINT ( 'NONE',  ( 109.1589550718175161, -0.0002241941239326466313, -0.007571935245608773894 ) ) ;
#17361 = CARTESIAN_POINT ( 'NONE',  ( 32.73300124599739291, 55.46353551262154014, -103.7392577722169875 ) ) ;
#17362 = CARTESIAN_POINT ( 'NONE',  ( -4.473127245936431073, 12.17046501147583548, 47.80062405537787384 ) ) ;
#17363 = B_SPLINE_CURVE_WITH_KNOTS ( 'NONE', 3,
 ( #3739, #23626, #8353, #17113 ),
 .UNSPECIFIED., .F., .F.,
 ( 4, 4 ),
 ( 0.000000000000000000, 0.01077107196513866529 ),
 .UNSPECIFIED. ) ;
#17364 = ORIENTED_EDGE ( 'NONE', *, *, #9336, .T. ) ;
#17365 = CARTESIAN_POINT ( 'NONE',  ( -8.786685647604890903, -25.35688121747466184, 47.14957014837381166 ) ) ;
#17366 = CIRCLE ( 'NONE', #15058, 117.6351876552689504 ) ;
#17367 = CARTESIAN_POINT ( 'NONE',  ( 1.833838850855486591, 15.25659494068298550, -144.3055354793885101 ) ) ;
#17368 = ORIENTED_EDGE ( 'NONE', *, *, #23215, .T. ) ;
#17369 = CARTESIAN_POINT ( 'NONE',  ( 2.108985857320909929, -28.95357181520926204, 142.3791757917252312 ) ) ;
#17370 = EDGE_LOOP ( 'NONE', ( #16025, #26438, #22773, #15939 ) ) ;
#17371 = CARTESIAN_POINT ( 'NONE',  ( 109.1778270068192853, 0.004349865064721243624, -0.008236503545668650075 ) ) ;
#17372 = CARTESIAN_POINT ( 'NONE',  ( 2.430230287190589422, -98.44218333480696970, -107.1617224697474313 ) ) ;
#17373 = EDGE_CURVE ( 'NONE', #22045, #3326, #7335, .T. ) ;
#17374 = ORIENTED_EDGE ( 'NONE', *, *, #22607, .F. ) ;
#17375 = CARTESIAN_POINT ( 'NONE',  ( 25.64681081121879203, 11.38886654529823694, -112.3352186517029594 ) ) ;
#17376 = CARTESIAN_POINT ( 'NONE',  ( 10.93730112725990367, -84.82621002473354110, -125.1380233598488019 ) ) ;
#17377 = CARTESIAN_POINT ( 'NONE',  ( -25.21435515916025594, 1.749597353048488237E-16, -4.373993382621220594E-17 ) ) ;
#17378 = CARTESIAN_POINT ( 'NONE',  ( 25.65782528836481902, 46.45532072021325831, -102.9197507294671254 ) ) ;
#17379 = CARTESIAN_POINT ( 'NONE',  ( 25.64699802086723324, 23.70809581152608558, 110.3941571196681650 ) ) ;
#17380 = LINE ( 'NONE', #6604, #11992 ) ;
#17381 = CARTESIAN_POINT ( 'NONE',  ( -1.619063947482197729, 2.489035965910159298, -46.30105812165548684 ) ) ;
#17382 = CARTESIAN_POINT ( 'NONE',  ( 25.69398547355839924, 110.6264597420659896, 22.75551036951965145 ) ) ;
#17383 = VECTOR ( 'NONE', #19703, 1000.000000000000000 ) ;
#17384 =( BOUNDED_SURFACE ( )  B_SPLINE_SURFACE ( 3, 1, ( 
 ( #3089, #924 ),
 ( #9710, #14295 ),
 ( #1074, #24295 ),
 ( #18482, #23113 ) ),
 .UNSPECIFIED., .F., .F., .F. ) 
 B_SPLINE_SURFACE_WITH_KNOTS ( ( 4, 4 ),
 ( 2, 2 ),
 ( 0.000000000000000000, 1.000000000000000000 ),
 ( 0.000000000000000000, 1.000000000000000000 ),
 .UNSPECIFIED. ) 
 GEOMETRIC_REPRESENTATION_ITEM ( )  RATIONAL_B_SPLINE_SURFACE ( (
 ( 1.000000000000000000, 1.000000000000000000),
 ( 0.9960225298536222738, 0.9999952330161893110),
 ( 0.9960225298536222738, 0.9999952330161893110),
 ( 1.000000000000000000, 1.000000000000000000) ) ) 
 REPRESENTATION_ITEM ( '' )  SURFACE ( )  );
#17385 = CARTESIAN_POINT ( 'NONE',  ( 26.28373643307435614, 88.40064398364036435, 91.96212244992378260 ) ) ;
#17386 = CARTESIAN_POINT ( 'NONE',  ( -1.619063947482194177, 25.20140673341374438, -38.92136151114915066 ) ) ;
#17387 = CONICAL_SURFACE ( 'NONE', #21062, 117.6351876552689504, 0.9945805576725580410 ) ;
#17388 = LINE ( 'NONE', #11339, #18710 ) ;
#17389 = ORIENTED_EDGE ( 'NONE', *, *, #1018, .F. ) ;
#17390 = ORIENTED_EDGE ( 'NONE', *, *, #11224, .T. ) ;
#17391 = CARTESIAN_POINT ( 'NONE',  ( 25.64692232868535626, 103.2819624397967857, 45.62640214192299482 ) ) ;
#17392 = CARTESIAN_POINT ( 'NONE',  ( 109.1586900883932856, 0.002995460350180808098, -0.006479576224403798407 ) ) ;
#17393 = CARTESIAN_POINT ( 'NONE',  ( -28.41354790283022069, 23.16239616762931064, -1.249099604787157425 ) ) ;
#17394 = CARTESIAN_POINT ( 'NONE',  ( 32.73300124599732186, 0.000000000000000000, 0.000000000000000000 ) ) ;
#17395 = CARTESIAN_POINT ( 'NONE',  ( 30.59138290137885718, -84.53179630244041221, 79.74792615266116513 ) ) ;
#17396 = CARTESIAN_POINT ( 'NONE',  ( -1.050230346682680560, 26.92058491724867153, -37.05182464821992028 ) ) ;
#17397 = ORIENTED_EDGE ( 'NONE', *, *, #24094, .F. ) ;
#17398 = CARTESIAN_POINT ( 'NONE',  ( 2.263178113027050742, 132.2496129425960021, 60.41552743271004999 ) ) ;
#17399 = CARTESIAN_POINT ( 'NONE',  ( -2.911734481061402757, -12.03743348210748998, 46.11606034418773703 ) ) ;
#17400 = CARTESIAN_POINT ( 'NONE',  ( -28.13707043255157103, -22.88591869784690402, 0.7675454997509406629 ) ) ;
#17401 = CARTESIAN_POINT ( 'NONE',  ( -1.113427685306989767, -42.96952363574823863, 16.03057832159198171 ) ) ;
#17402 = B_SPLINE_CURVE_WITH_KNOTS ( 'NONE', 3,
 ( #7259, #24246, #11139, #198 ),
 .UNSPECIFIED., .F., .F.,
 ( 4, 4 ),
 ( 0.000000000000000000, 0.01077107196513803732 ),
 .UNSPECIFIED. ) ;
#17403 = ORIENTED_EDGE ( 'NONE', *, *, #8584, .T. ) ;
#17404 = CARTESIAN_POINT ( 'NONE',  ( 25.64703792032470986, -112.3081285890369969, -11.65444440562296080 ) ) ;
#17405 = FACE_OUTER_BOUND ( 'NONE', #2633, .T. ) ;
#17406 = ORIENTED_EDGE ( 'NONE', *, *, #5904, .F. ) ;
#17407 = VERTEX_POINT ( 'NONE', #4989 ) ;
#17408 = EDGE_CURVE ( 'NONE', #27461, #20232, #24875, .T. ) ;
#17409 = VERTEX_POINT ( 'NONE', #26716 ) ;
#17410 = EDGE_CURVE ( 'NONE', #28403, #16995, #11769, .T. ) ;
#17411 = B_SPLINE_CURVE_WITH_KNOTS ( 'NONE', 3,
 ( #2983, #671, #7744, #16499 ),
 .UNSPECIFIED., .F., .F.,
 ( 4, 4 ),
 ( 0.000000000000000000, 0.01077107196513895152 ),
 .UNSPECIFIED. ) ;
#17412 = EDGE_CURVE ( 'NONE', #14332, #15158, #9718, .T. ) ;
#17413 = B_SPLINE_CURVE_WITH_KNOTS ( 'NONE', 3,
 ( #10023, #26977, #22986, #7583, #27417, #24851, #14461, #5546 ),
 .UNSPECIFIED., .F., .F.,
 ( 4, 2, 2, 4 ),
 ( 6.938893903907228378E-18, 0.0002429588503611322453, 0.0004859177007222575517, 0.0009718354014444986234 ),
 .UNSPECIFIED. ) ;
#17414 = CARTESIAN_POINT ( 'NONE',  ( 28.43349137099836099, -34.52178142065613287, 119.3601175884733010 ) ) ;
#17415 = CARTESIAN_POINT ( 'NONE',  ( -4.473127245936431073, -3.196405119333463496, 49.22197550883370809 ) ) ;
#17416 = CARTESIAN_POINT ( 'NONE',  ( -4.162674018437141576, 18.33413805792438112, -45.34593312138888876 ) ) ;
#17417 = CARTESIAN_POINT ( 'NONE',  ( 1.833691583653550561, 72.24637705290489009, 125.8462703805701466 ) ) ;
#17418 =( BOUNDED_SURFACE ( )  B_SPLINE_SURFACE ( 3, 1, ( 
 ( #18308, #16166 ),
 ( #24966, #3212 ),
 ( #13861, #14001 ),
 ( #7699, #25247 ) ),
 .UNSPECIFIED., .F., .F., .F. ) 
 B_SPLINE_SURFACE_WITH_KNOTS ( ( 4, 4 ),
 ( 2, 2 ),
 ( 0.000000000000000000, 1.000000000000000000 ),
 ( 0.000000000000000000, 1.000000000000000000 ),
 .UNSPECIFIED. ) 
 GEOMETRIC_REPRESENTATION_ITEM ( )  RATIONAL_B_SPLINE_SURFACE ( (
 ( 1.000000000000000000, 1.000000000000000000),
 ( 0.6386103224230302855, 0.9954351624131538845),
 ( 0.6386103224230302855, 0.9954351624131538845),
 ( 1.000000000000000000, 1.000000000000000000) ) ) 
 REPRESENTATION_ITEM ( '' )  SURFACE ( )  );
#17419 = CARTESIAN_POINT ( 'NONE',  ( -7.733045908741337016, 47.75066202881826882, 21.80378472388440514 ) ) ;
#17420 = ORIENTED_EDGE ( 'NONE', *, *, #2728, .F. ) ;
#17421 = CARTESIAN_POINT ( 'NONE',  ( -25.21435515916025594, 1.749597353048488237E-16, -4.373993382621220594E-17 ) ) ;
#17422 = CARTESIAN_POINT ( 'NONE',  ( -18.41936578851709783, -18.42310649277602508, 38.22933728004711185 ) ) ;
#17423 = CARTESIAN_POINT ( 'NONE',  ( -1.259972190295302497, -12.06706380853662530, 44.39825172539707410 ) ) ;
#17424 = LINE ( 'NONE', #8251, #521 ) ;
#17425 = CARTESIAN_POINT ( 'NONE',  ( -1.539760825549681966, -35.94320866319468166, 29.16712717142800670 ) ) ;
#17426 = CARTESIAN_POINT ( 'NONE',  ( -1.619063947482201282, -11.94059994246191359, -44.80407745103779860 ) ) ;
#17427 = CARTESIAN_POINT ( 'NONE',  ( -20.37983603106074426, -10.62371319148622284, 27.81368274044722000 ) ) ;
#17428 = B_SPLINE_CURVE_WITH_KNOTS ( 'NONE', 3,
 ( #9582, #3108, #20219, #16338 ),
 .UNSPECIFIED., .F., .F.,
 ( 4, 4 ),
 ( 2.396682302503802907E-16, 0.008383748772659700005 ),
 .UNSPECIFIED. ) ;
#17429 = CARTESIAN_POINT ( 'NONE',  ( 1.833485406944043827, 58.53321471326877656, 132.7804117027889674 ) ) ;
#17430 = ORIENTED_EDGE ( 'NONE', *, *, #23096, .T. ) ;
#17431 = EDGE_CURVE ( 'NONE', #16169, #26958, #7031, .T. ) ;
#17432 = ORIENTED_EDGE ( 'NONE', *, *, #10596, .F. ) ;
#17433 = CARTESIAN_POINT ( 'NONE',  ( 25.69398547355839568, -24.20764173643324213, -110.3177996916217154 ) ) ;
#17434 = CARTESIAN_POINT ( 'NONE',  ( 32.73300124599738581, 28.19767303745763698, -114.2056417606545153 ) ) ;
#17435 = EDGE_LOOP ( 'NONE', ( #9069, #9882, #15964, #18284 ) ) ;
#17436 = ORIENTED_EDGE ( 'NONE', *, *, #12510, .F. ) ;
#17437 = EDGE_LOOP ( 'NONE', ( #15290, #19674, #5491, #23081 ) ) ;
#17438 = EDGE_CURVE ( 'NONE', #17941, #6242, #9248, .T. ) ;
#17439 = CARTESIAN_POINT ( 'NONE',  ( 25.64681081121880624, -45.54494737132293380, 103.3177883989777825 ) ) ;
#17440 = VECTOR ( 'NONE', #5972, 1000.000000000000227 ) ;
#17441 = CARTESIAN_POINT ( 'NONE',  ( 2.430230287190581429, 125.2872625092162338, 74.01081053031141721 ) ) ;
#17442 = CARTESIAN_POINT ( 'NONE',  ( 10.93730112725971360, 36.23586118136525158, 146.7718404940643211 ) ) ;
#17443 = FACE_OUTER_BOUND ( 'NONE', #7342, .T. ) ;
#17444 = CARTESIAN_POINT ( 'NONE',  ( -20.57838717382308147, -25.16001208503093522, 16.28767523336148315 ) ) ;
#17445 = CARTESIAN_POINT ( 'NONE',  ( 25.86096068574581963, 24.48003142199239690, -110.3716997142155947 ) ) ;
#17446 = CARTESIAN_POINT ( 'NONE',  ( -1.031422197589711764, 44.01264471863847660, -12.69107518035516691 ) ) ;
#17447 = CARTESIAN_POINT ( 'NONE',  ( -1.048994561756786625, 37.49601524795411223, -26.29622118251694829 ) ) ;
#17448 = FACE_OUTER_BOUND ( 'NONE', #17618, .T. ) ;
#17449 = ORIENTED_EDGE ( 'NONE', *, *, #19306, .T. ) ;
#17450 =( BOUNDED_SURFACE ( )  B_SPLINE_SURFACE ( 3, 1, ( 
 ( #23399, #27114 ),
 ( #7423, #22834 ),
 ( #3098, #22980 ),
 ( #10015, #25269 ) ),
 .UNSPECIFIED., .F., .F., .F. ) 
 B_SPLINE_SURFACE_WITH_KNOTS ( ( 4, 4 ),
 ( 2, 2 ),
 ( 0.000000000000000000, 1.000000000000000000 ),
 ( 0.000000000000000000, 1.000000000000000000 ),
 .UNSPECIFIED. ) 
 GEOMETRIC_REPRESENTATION_ITEM ( )  RATIONAL_B_SPLINE_SURFACE ( (
 ( 1.000000000000000000, 1.000000000000000000),
 ( 0.9960225298536222738, 0.9999952330161893110),
 ( 0.9960225298536222738, 0.9999952330161893110),
 ( 1.000000000000000000, 1.000000000000000000) ) ) 
 REPRESENTATION_ITEM ( '' )  SURFACE ( )  );
#17451 = VERTEX_POINT ( 'NONE', #7456 ) ;
#17453 = CARTESIAN_POINT ( 'NONE',  ( -1.583189561560252701, 38.94740041318296164, -25.21827308671245760 ) ) ;
#17452 = CARTESIAN_POINT ( 'NONE',  ( -55.24390624410018802, 0.007503127514278223366, 0.007245494385991344682 ) ) ;
#17454 = AXIS2_PLACEMENT_3D ( 'NONE', #19229, #28004, #14906 ) ;
#17455 = CARTESIAN_POINT ( 'NONE',  ( 25.64692232868535626, -103.2819624397965015, -45.62640214192366983 ) ) ;
#17456 = CARTESIAN_POINT ( 'NONE',  ( -55.25297051322618813, -0.007247191603128547155, 0.01306918787467270006 ) ) ;
#17457 = CARTESIAN_POINT ( 'NONE',  ( -1.539763995773687055, -43.19716353142342768, -16.63252574783026816 ) ) ;
#17458 = CARTESIAN_POINT ( 'NONE',  ( -1.323439229708149867, 35.86372896917474407, -28.92147054731853828 ) ) ;
#17459 = B_SPLINE_CURVE_WITH_KNOTS ( 'NONE', 3,
 ( #9805, #5030, #14094, #7219, #24920, #25196, #3034, #24781, #16268, #25065 ),
 .UNSPECIFIED., .F., .F.,
 ( 4, 3, 3, 4 ),
 ( 3.469446951953614805E-17, 0.0002669559177086245683, 0.0005339118354150954775, 0.001067817517169162948 ),
 .UNSPECIFIED. ) ;
#17460 = ORIENTED_EDGE ( 'NONE', *, *, #17408, .F. ) ;
#17461 = CARTESIAN_POINT ( 'NONE',  ( 25.64708010899964208, 97.75667227735169718, -56.50300922386492175 ) ) ;
#17462 = ADVANCED_FACE ( 'NONE', ( #13332 ), #23473, .F. ) ;
#17463 = CARTESIAN_POINT ( 'NONE',  ( -20.20700224038492721, -16.58740185276692358, 24.51628800869065827 ) ) ;
#17464 = CARTESIAN_POINT ( 'NONE',  ( -1.045287976400383290, -36.12803364096628655, -28.14015102489793918 ) ) ;
#17465 = ORIENTED_EDGE ( 'NONE', *, *, #26603, .F. ) ;
#17466 = ORIENTED_EDGE ( 'NONE', *, *, #7596, .F. ) ;
#17467 = ADVANCED_FACE ( 'NONE', ( #7606 ), #17554, .F. ) ;
#17468 = CARTESIAN_POINT ( 'NONE',  ( -1.155031165708871654, -28.62780465193337420, -35.88345263711039479 ) ) ;
#17469 =( BOUNDED_SURFACE ( )  B_SPLINE_SURFACE ( 3, 1, ( 
 ( #25797, #17150 ),
 ( #10279, #5806 ),
 ( #3771, #23371 ),
 ( #25937, #28217 ) ),
 .UNSPECIFIED., .F., .F., .F. ) 
 B_SPLINE_SURFACE_WITH_KNOTS ( ( 4, 4 ),
 ( 2, 2 ),
 ( 0.000000000000000000, 1.000000000000000000 ),
 ( 0.000000000000000000, 1.000000000000000000 ),
 .UNSPECIFIED. ) 
 GEOMETRIC_REPRESENTATION_ITEM ( )  RATIONAL_B_SPLINE_SURFACE ( (
 ( 1.000000000000000000, 1.000000000000000000),
 ( 0.6386103224230316178, 0.9954351624131538845),
 ( 0.6386103224230316178, 0.9954351624131538845),
 ( 1.000000000000000000, 1.000000000000000000) ) ) 
 REPRESENTATION_ITEM ( '' )  SURFACE ( )  );
#17470 = VERTEX_POINT ( 'NONE', #1531 ) ;
#17471 = FACE_OUTER_BOUND ( 'NONE', #19770, .T. ) ;
#17472 = EDGE_LOOP ( 'NONE', ( #2200, #19833, #22176, #4738 ) ) ;
#17473 = EDGE_CURVE ( 'NONE', #26453, #11824, #20958, .T. ) ;
#17474 = B_SPLINE_CURVE_WITH_KNOTS ( 'NONE', 3,
 ( #9634, #22756, #848, #20706, #5456, #13797, #9789 ),
 .UNSPECIFIED., .F., .F.,
 ( 4, 3, 4 ),
 ( 8.845388854693243284E-18, 0.009512539173626379310, 0.02506242213020843518 ),
 .UNSPECIFIED. ) ;
#17475 = ADVANCED_FACE ( 'NONE', ( #3411 ), #11504, .F. ) ;
#17476 = EDGE_LOOP ( 'NONE', ( #18002, #11190, #27986, #21794 ) ) ;
#17477 = AXIS2_PLACEMENT_3D ( 'NONE', #13045, #26011, #6172 ) ;
#17478 = CARTESIAN_POINT ( 'NONE',  ( 1.832998868059858122, 97.49378069860796359, 107.4798986104863303 ) ) ;
#17479 = AXIS2_PLACEMENT_3D ( 'NONE', #28438, #4849, #9319 ) ;
#17480 = B_SPLINE_CURVE_WITH_KNOTS ( 'NONE', 3,
 ( #2123, #17675, #20116, #4304, #26454, #15083, #19557 ),
 .UNSPECIFIED., .F., .F.,
 ( 4, 3, 4 ),
 ( 0.000000000000000000, 0.006568092053401831769, 0.02506242213020820619 ),
 .UNSPECIFIED. ) ;
#17481 = CARTESIAN_POINT ( 'NONE',  ( 19.66333377628702195, -84.55762186019634896, 108.7423656420555886 ) ) ;
#17482 = CARTESIAN_POINT ( 'NONE',  ( 13.36082413113061307, -53.25066407421903847, 143.3553710183987562 ) ) ;
#17483 = AXIS2_PLACEMENT_3D ( 'NONE', #26092, #5355, #13843 ) ;
#17484 = CARTESIAN_POINT ( 'NONE',  ( -1.046935749540006011, 12.93334586714240331, 43.93230528057167561 ) ) ;
#17485 = DIRECTION ( 'NONE',  ( -1.000000000000000000, 6.938893903907226837E-18, -1.734723475976806709E-18 ) ) ;
#17486 = CARTESIAN_POINT ( 'NONE',  ( 9.884929003653608603, 150.4771565009630478, 4.203795436552891118 ) ) ;
#17487 = CARTESIAN_POINT ( 'NONE',  ( 1.832998868059858122, -132.3466930259789933, -59.50898020732644511 ) ) ;
#17488 = CARTESIAN_POINT ( 'NONE',  ( 10.93730112725932635, 0.000000000000000000, 0.000000000000000000 ) ) ;
#17490 = CARTESIAN_POINT ( 'NONE',  ( 5.340103556456345046, 96.93942141426060743, 111.1041836730281034 ) ) ;
#17489 = DIRECTION ( 'NONE',  ( -0.5946245182733607137, -0.8039981203473692828, 0.002950380665382086945 ) ) ;
#17491 = CARTESIAN_POINT ( 'NONE',  ( 2.433796855181233454, 98.43889364293860922, 107.1581411821788947 ) ) ;
#17492 = VERTEX_POINT ( 'NONE', #5864 ) ;
#17493 = EDGE_LOOP ( 'NONE', ( #19924, #9529, #3214, #27031 ) ) ;
#17494 = CARTESIAN_POINT ( 'NONE',  ( 25.64708228042119842, 56.48974615489059659, -97.76433875577585297 ) ) ;
#17495 = CARTESIAN_POINT ( 'NONE',  ( 55.49584447822657296, -66.38758986585135347, 29.26468316696749739 ) ) ;
#17496 = CARTESIAN_POINT ( 'NONE',  ( -1.045287976400365970, 1.530335034933814731, -45.76855895860946788 ) ) ;
#17497 = CARTESIAN_POINT ( 'NONE',  ( -21.81686047589427702, 18.24499610240089353, 33.92779429964183890 ) ) ;
#17498 = CARTESIAN_POINT ( 'NONE',  ( 6.224689322667647851, 76.23997225729267768, 126.9212313063847120 ) ) ;
#17499 = CARTESIAN_POINT ( 'NONE',  ( 1.833206308920099170, -137.7753864329222040, -45.54896581797600419 ) ) ;
#17500 = VERTEX_POINT ( 'NONE', #23427 ) ;
#17501 = VECTOR ( 'NONE', #21231, 999.9999999999998863 ) ;
#17502 = CARTESIAN_POINT ( 'NONE',  ( -55.24390624410018802, 0.001451500391953283731, -0.01032895241566680888 ) ) ;
#17503 = CARTESIAN_POINT ( 'NONE',  ( -1.031422197589711987, -45.78027046666441890, 1.530725436377941673 ) ) ;
#17504 = CARTESIAN_POINT ( 'NONE',  ( -4.178947244162626973, 31.41809272265978947, 37.51424432987617053 ) ) ;
#17505 = EDGE_CURVE ( 'NONE', #4937, #28149, #6254, .T. ) ;
#17506 = ORIENTED_EDGE ( 'NONE', *, *, #22395, .T. ) ;
#17507 = CARTESIAN_POINT ( 'NONE',  ( 109.1721716018069657, -0.008708654716139515445, -0.01467989464939307293 ) ) ;
#17509 = VECTOR ( 'NONE', #24889, 1000.000000000000000 ) ;
#17508 =( BOUNDED_SURFACE ( )  B_SPLINE_SURFACE ( 3, 1, ( 
 ( #663, #3110 ),
 ( #7436, #11600 ),
 ( #16056, #9311 ),
 ( #26701, #18505 ) ),
 .UNSPECIFIED., .F., .F., .F. ) 
 B_SPLINE_SURFACE_WITH_KNOTS ( ( 4, 4 ),
 ( 2, 2 ),
 ( 0.000000000000000000, 1.000000000000000000 ),
 ( 0.000000000000000000, 1.000000000000000000 ),
 .UNSPECIFIED. ) 
 GEOMETRIC_REPRESENTATION_ITEM ( )  RATIONAL_B_SPLINE_SURFACE ( (
 ( 1.000000000000000000, 1.000000000000000000),
 ( 0.9956975270656955868, 0.8568959468854907557),
 ( 0.9956975270656955868, 0.8568959468854907557),
 ( 1.000000000000000000, 1.000000000000000000) ) ) 
 REPRESENTATION_ITEM ( '' )  SURFACE ( )  );
#17510 = EDGE_CURVE ( 'NONE', #8086, #2685, #11392, .T. ) ;
#17511 = CARTESIAN_POINT ( 'NONE',  ( 1.833721034905652525, 14.81406766076126047, -144.3516387774750456 ) ) ;
#17512 = EDGE_LOOP ( 'NONE', ( #6694, #23703, #8022, #13613 ) ) ;
#17513 = DIRECTION ( 'NONE',  ( 1.000000000000000000, -6.938893903907226837E-18, 1.734723475976806709E-18 ) ) ;
#17514 = CARTESIAN_POINT ( 'NONE',  ( 6.224689322667630975, -57.86870174583338411, -136.2818611715196653 ) ) ;
#17515 = DIRECTION ( 'NONE',  ( 1.000000000000000000, -6.938893903907226837E-18, 1.734723475976806709E-18 ) ) ;
#17516 = EDGE_LOOP ( 'NONE', ( #25785, #4091, #20402, #15772 ) ) ;
#17517 = CARTESIAN_POINT ( 'NONE',  ( -25.21435515916043713, -23.92354251275918031, 25.00736669481048224 ) ) ;
#17518 = B_SPLINE_CURVE_WITH_KNOTS ( 'NONE', 3,
 ( #26848, #13896, #4974, #13747, #22706, #11750, #20517 ),
 .UNSPECIFIED., .F., .F.,
 ( 4, 3, 4 ),
 ( 0.000000000000000000, 0.02816610861753242670, 0.04000277880656208374 ),
 .UNSPECIFIED. ) ;
#17519 = CARTESIAN_POINT ( 'NONE',  ( -1.031422197589711987, 44.01264471863864713, 12.69107518035455762 ) ) ;
#17520 = AXIS2_PLACEMENT_3D ( 'NONE', #2288, #26068, #4046 ) ;
#17521 = CARTESIAN_POINT ( 'NONE',  ( 55.79472521941426777, 48.13855120843883384, 54.55111121764100091 ) ) ;
#17522 = CARTESIAN_POINT ( 'NONE',  ( 5.340103556456304190, 146.3832391989195116, 17.70136535449949022 ) ) ;
#17523 = CARTESIAN_POINT ( 'NONE',  ( 9.884929003653626367, -146.3148513795968881, 35.39789245780281846 ) ) ;
#17524 = CIRCLE ( 'NONE', #20284, 151.1787379149930359 ) ;
#17525 = CARTESIAN_POINT ( 'NONE',  ( -25.21435515916043713, 15.02493970636190745, 31.17620025257570759 ) ) ;
#17526 = CARTESIAN_POINT ( 'NONE',  ( -4.473127245936431073, -12.17046501147550153, -47.80062405537796622 ) ) ;
#17527 = FACE_OUTER_BOUND ( 'NONE', #59, .T. ) ;
#17528 = CARTESIAN_POINT ( 'NONE',  ( 25.64660436782584796, -98.07256794792245103, -55.95243482911472199 ) ) ;
#17529 = ORIENTED_EDGE ( 'NONE', *, *, #17431, .F. ) ;
#17530 = AXIS2_PLACEMENT_3D ( 'NONE', #12026, #16482, #5700 ) ;
#17531 = ORIENTED_EDGE ( 'NONE', *, *, #10678, .F. ) ;
#17532 = CARTESIAN_POINT ( 'NONE',  ( -23.77929240705206837, -15.74261278740695502, -32.66578242509739027 ) ) ;
#17533 = CARTESIAN_POINT ( 'NONE',  ( 10.93730112725990367, -149.7554878793147566, -20.69552240458495973 ) ) ;
#17534 = CARTESIAN_POINT ( 'NONE',  ( 109.1587776205901577, -0.006661366261224517873, -0.003057017121591183717 ) ) ;
#17535 = CARTESIAN_POINT ( 'NONE',  ( -18.41936578851712980, -41.75701384111727776, 7.566034416291218534 ) ) ;
#17536 = CARTESIAN_POINT ( 'NONE',  ( 28.43349137099833612, -42.22940898499130924, -116.8557575815932950 ) ) ;
#17537 = CARTESIAN_POINT ( 'NONE',  ( 25.64660436782552466, 46.45435812945243015, 102.9120797476509779 ) ) ;
#17538 = ORIENTED_EDGE ( 'NONE', *, *, #522, .F. ) ;
#17539 = CARTESIAN_POINT ( 'NONE',  ( -1.031422197589716205, -44.01264471863856897, -12.69107518035485782 ) ) ;
#17540 = CARTESIAN_POINT ( 'NONE',  ( -22.23226125620944771, 26.80886670319662102, 16.78323347921887887 ) ) ;
#17541 = CARTESIAN_POINT ( 'NONE',  ( 1.833485406944043827, 117.0814567582556407, -85.72460230293573602 ) ) ;
#17542 = CARTESIAN_POINT ( 'NONE',  ( -20.20700224038492721, -28.44216453106542986, -8.199606986804219844 ) ) ;
#17543 = EDGE_CURVE ( 'NONE', #12674, #7760, #16547, .T. ) ;
#17544 = CARTESIAN_POINT ( 'NONE',  ( -1.619063947482197729, -43.26576862488421682, 16.67502769180607203 ) ) ;
#17545 = CARTESIAN_POINT ( 'NONE',  ( 21.16825799904897210, 9.757279788664570574, -135.0813719997368594 ) ) ;
#17546 = EDGE_CURVE ( 'NONE', #207, #3333, #7269, .T. ) ;
#17547 = CARTESIAN_POINT ( 'NONE',  ( 2.063896406836609909, 43.61045647697875438, -138.5688025270874562 ) ) ;
#17548 = VERTEX_POINT ( 'NONE', #27870 ) ;
#17549 = ADVANCED_FACE ( 'NONE', ( #3126 ), #20329, .F. ) ;
#17550 = ORIENTED_EDGE ( 'NONE', *, *, #10706, .T. ) ;
#17551 = ORIENTED_EDGE ( 'NONE', *, *, #18283, .F. ) ;
#17552 = VECTOR ( 'NONE', #758, 999.9999999999998863 ) ;
#17553 = CARTESIAN_POINT ( 'NONE',  ( -1.239374126674604337, -42.99367564261289942, -16.50008610789281605 ) ) ;
#17554 =( BOUNDED_SURFACE ( )  B_SPLINE_SURFACE ( 3, 1, ( 
 ( #14625, #23154 ),
 ( #1112, #27576 ),
 ( #20825, #7895 ),
 ( #21096, #16806 ) ),
 .UNSPECIFIED., .F., .F., .F. ) 
 B_SPLINE_SURFACE_WITH_KNOTS ( ( 4, 4 ),
 ( 2, 2 ),
 ( 0.000000000000000000, 1.000000000000000000 ),
 ( 0.000000000000000000, 1.000000000000000000 ),
 .UNSPECIFIED. ) 
 GEOMETRIC_REPRESENTATION_ITEM ( )  RATIONAL_B_SPLINE_SURFACE ( (
 ( 1.000000000000000000, 1.000000000000000000),
 ( 0.9956975270656954757, 0.8568959468854893125),
 ( 0.9956975270656954757, 0.8568959468854893125),
 ( 1.000000000000000000, 1.000000000000000000) ) ) 
 REPRESENTATION_ITEM ( '' )  SURFACE ( )  );
#17555 = CARTESIAN_POINT ( 'NONE',  ( 109.1586900883932856, -0.005715190711481754789, 0.004277182003227202392 ) ) ;
#17556 = VERTEX_POINT ( 'NONE', #25154 ) ;
#17557 = CARTESIAN_POINT ( 'NONE',  ( 1.833721034905633873, 72.86293192427493182, 125.4904194343087198 ) ) ;
#17558 = FACE_OUTER_BOUND ( 'NONE', #4709, .T. ) ;
#17559 = ORIENTED_EDGE ( 'NONE', *, *, #2942, .T. ) ;
#17560 = EDGE_LOOP ( 'NONE', ( #7210, #16289, #3362, #8858 ) ) ;
#17561 = CARTESIAN_POINT ( 'NONE',  ( 1.833603222531957178, 142.0304769734132435, -29.73464781350118358 ) ) ;
#17562 = CARTESIAN_POINT ( 'NONE',  ( -55.24198130335446422, 0.008252882783650522525, -0.004276389980776339715 ) ) ;
#17563 = CARTESIAN_POINT ( 'NONE',  ( -4.178947244162629637, 25.96944194166794162, -41.47292084251642308 ) ) ;
#17564 = CIRCLE ( 'NONE', #24954, 20.00000000000000000 ) ;
#17565 = EDGE_CURVE ( 'NONE', #12449, #21771, #25858, .T. ) ;
#17566 = CARTESIAN_POINT ( 'NONE',  ( -55.24728320129491266, 0.01402509393918583563, -0.003868537197317189515 ) ) ;
#17567 = CARTESIAN_POINT ( 'NONE',  ( -20.57838717382308147, -25.16001208503093522, 16.28767523336148315 ) ) ;
#17568 = AXIS2_PLACEMENT_3D ( 'NONE', #24086, #19190, #4346 ) ;
#17569 = EDGE_CURVE ( 'NONE', #24736, #531, #26108, .T. ) ;
#17570 = CARTESIAN_POINT ( 'NONE',  ( 1.834118845439484335, -72.70910183320656017, 125.5799175751967454 ) ) ;
#17571 = CARTESIAN_POINT ( 'NONE',  ( 1.833485406944043827, 14.63699153649359452, 144.3694338680885778 ) ) ;
#17572 = CARTESIAN_POINT ( 'NONE',  ( -1.056502255334265339, -26.51074901220530222, -37.35734037467625512 ) ) ;
#17573 = EDGE_CURVE ( 'NONE', #8689, #21137, #22354, .T. ) ;
#17574 = CARTESIAN_POINT ( 'NONE',  ( 26.11404676487257603, -110.9778746459745520, -22.43340081644882389 ) ) ;
#17575 = VERTEX_POINT ( 'NONE', #12601 ) ;
#17576 = VERTEX_POINT ( 'NONE', #3969 ) ;
#17577 = LINE ( 'NONE', #13257, #1872 ) ;
#17578 = LINE ( 'NONE', #8668, #9312 ) ;
#17579 = VERTEX_POINT ( 'NONE', #6155 ) ;
#17580 = VERTEX_POINT ( 'NONE', #13030 ) ;
#17581 = ORIENTED_EDGE ( 'NONE', *, *, #19954, .T. ) ;
#17582 = CARTESIAN_POINT ( 'NONE',  ( 28.37599760073042532, 84.05168479399091552, 78.09498850373434209 ) ) ;
#17583 = AXIS2_PLACEMENT_3D ( 'NONE', #13415, #15715, #11270 ) ;
#17584 = CARTESIAN_POINT ( 'NONE',  ( 2.063896406836609909, -107.0521644432424040, 98.19887492195825018 ) ) ;
#17586 =( BOUNDED_SURFACE ( )  B_SPLINE_SURFACE ( 3, 1, ( 
 ( #24056, #9064 ),
 ( #15659, #21740 ),
 ( #17688, #26190 ),
 ( #26329, #15380 ) ),
 .UNSPECIFIED., .F., .F., .F. ) 
 B_SPLINE_SURFACE_WITH_KNOTS ( ( 4, 4 ),
 ( 2, 2 ),
 ( 0.000000000000000000, 1.000000000000000000 ),
 ( 0.000000000000000000, 1.000000000000000000 ),
 .UNSPECIFIED. ) 
 GEOMETRIC_REPRESENTATION_ITEM ( )  RATIONAL_B_SPLINE_SURFACE ( (
 ( 1.000000000000000000, 1.000000000000000000),
 ( 0.6386103224230302855, 0.9954351624131538845),
 ( 0.6386103224230302855, 0.9954351624131538845),
 ( 1.000000000000000000, 1.000000000000000000) ) ) 
 REPRESENTATION_ITEM ( '' )  SURFACE ( )  );
#17585 = AXIS2_PLACEMENT_3D ( 'NONE', #16390, #10969, #10361 ) ;
#17587 = B_SPLINE_CURVE_WITH_KNOTS ( 'NONE', 3,
 ( #27037, #14228, #9801, #18570, #27338, #5466, #23050, #3313 ),
 .UNSPECIFIED., .F., .F.,
 ( 4, 2, 2, 4 ),
 ( 1.250926888277100303E-17, 0.0002429592666046748086, 0.0004859185332093370947, 0.0009718370664186629137 ),
 .UNSPECIFIED. ) ;
#17588 = CARTESIAN_POINT ( 'NONE',  ( 2.263178607246715490, -144.4462811785177223, 16.59120332983095381 ) ) ;
#17589 = CARTESIAN_POINT ( 'NONE',  ( -20.47566338032522637, -18.81547714195493626, -23.19796701701864805 ) ) ;
#17590 = CARTESIAN_POINT ( 'NONE',  ( -1.463510566862833207, -25.15876608740840936, -38.76366072687767428 ) ) ;
#17591 = CARTESIAN_POINT ( 'NONE',  ( 1.833485406944057594, 44.33323125130110043, -138.1714136985304151 ) ) ;
#17592 = CARTESIAN_POINT ( 'NONE',  ( -23.77929240705206126, -6.464423883190137055, 35.68044874544703049 ) ) ;
#17593 = CARTESIAN_POINT ( 'NONE',  ( -25.21435515916043002, 34.05351380035335040, -6.169479169075572145 ) ) ;
#17594 = CARTESIAN_POINT ( 'NONE',  ( -22.34422965417124374, 17.95715691811047776, -33.39267070835825990 ) ) ;
#17595 = ADVANCED_FACE ( 'NONE', ( #21816 ), #6732, .F. ) ;
#17596 = CARTESIAN_POINT ( 'NONE',  ( 26.28373643307404350, -108.3320567927994915, 67.34887744616746375 ) ) ;
#17597 = CARTESIAN_POINT ( 'NONE',  ( -1.045287976400365970, 28.14015102489882736, 36.12803364096558312 ) ) ;
#17598 = CARTESIAN_POINT ( 'NONE',  ( -55.24300891470648622, -0.009225237711097735230, -0.003362556190414862749 ) ) ;
#17599 = EDGE_CURVE ( 'NONE', #13261, #21976, #13061, .T. ) ;
#17600 = ORIENTED_EDGE ( 'NONE', *, *, #21580, .F. ) ;
#17601 = EDGE_LOOP ( 'NONE', ( #19893, #22899, #20557, #15198 ) ) ;
#17602 = B_SPLINE_CURVE_WITH_KNOTS ( 'NONE', 3,
 ( #1606, #21464, #12680, #19301, #28076, #5804 ),
 .UNSPECIFIED., .F., .F.,
 ( 4, 2, 4 ),
 ( 0.000000000000000000, 0.0004335184443140258710, 0.0008670368886280517421 ),
 .UNSPECIFIED. ) ;
#17603 = CARTESIAN_POINT ( 'NONE',  ( 2.433796855181205476, 84.34988187690927930, 118.5671979538059730 ) ) ;
#17604 = CARTESIAN_POINT ( 'NONE',  ( 25.98107933586720009, -22.45325949158398160, -110.8834224379716176 ) ) ;
#17605 = CARTESIAN_POINT ( 'NONE',  ( -1.045287976400386842, 37.92705037016744285, -25.66401692420027203 ) ) ;
#17606 = CARTESIAN_POINT ( 'NONE',  ( -55.24198130335446422, 0.008310594958153458625, -0.004163123460802744397 ) ) ;
#17607 = CARTESIAN_POINT ( 'NONE',  ( 109.1586900883932856, 0.004701023939945712764, -0.005371970278528660422 ) ) ;
#17608 = VECTOR ( 'NONE', #26075, 1000.000000000000114 ) ;
#17609 = ORIENTED_EDGE ( 'NONE', *, *, #11300, .F. ) ;
#17610 = CARTESIAN_POINT ( 'NONE',  ( 2.263178113027036087, 145.3892419963351017, 1.401567040888699101 ) ) ;
#17611 = VECTOR ( 'NONE', #23469, 1000.000000000000000 ) ;
#17612 = ORIENTED_EDGE ( 'NONE', *, *, #459, .F. ) ;
#17613 = CARTESIAN_POINT ( 'NONE',  ( -2.911734481061402757, -25.69892591260238746, 40.13920818157105685 ) ) ;
#17614 = CARTESIAN_POINT ( 'NONE',  ( -55.24300891470650754, 0.0003472257464218577502, 0.009812809446892801005 ) ) ;
#17615 = VERTEX_POINT ( 'NONE', #21952 ) ;
#17616 = VERTEX_POINT ( 'NONE', #1662 ) ;
#17617 = CARTESIAN_POINT ( 'NONE',  ( -1.259972190295293393, -28.82609802125285015, -35.85909728507041194 ) ) ;
#17618 = EDGE_LOOP ( 'NONE', ( #345, #22017, #1039, #179 ) ) ;
#17619 = CARTESIAN_POINT ( 'NONE',  ( -22.34422965417125795, -34.15536449444077505, 16.46028608106144731 ) ) ;
#17620 = VERTEX_POINT ( 'NONE', #6417 ) ;
#17621 = CARTESIAN_POINT ( 'NONE',  ( 1.833485406944043827, -125.4007332306540405, -73.01664920993097496 ) ) ;
#17622 = CIRCLE ( 'NONE', #1989, 117.6351876552689504 ) ;
#17623 = ORIENTED_EDGE ( 'NONE', *, *, #7010, .F. ) ;
#17624 = CARTESIAN_POINT ( 'NONE',  ( 13.36082413113063083, -127.3428651193242445, -84.67697637120542709 ) ) ;
#17625 = AXIS2_PLACEMENT_3D ( 'NONE', #9750, #3271, #20957 ) ;
#17626 = CARTESIAN_POINT ( 'NONE',  ( 10.93730112725932635, 0.000000000000000000, 0.000000000000000000 ) ) ;
#17627 = EDGE_CURVE ( 'NONE', #19219, #12888, #24767, .T. ) ;
#17628 = CARTESIAN_POINT ( 'NONE',  ( 26.04756280548354752, -110.9306483680201296, -22.44333019059113354 ) ) ;
#17629 = CARTESIAN_POINT ( 'NONE',  ( -9.156249394959713683, 8.027840202794694235, 53.90509764945120708 ) ) ;
#17630 = LINE ( 'NONE', #26414, #22068 ) ;
#17631 = EDGE_CURVE ( 'NONE', #23299, #26154, #13163, .T. ) ;
#17632 = CARTESIAN_POINT ( 'NONE',  ( -20.20612092514784308, -16.46550332780508796, 24.59769888281551786 ) ) ;
#17633 = CARTESIAN_POINT ( 'NONE',  ( -1.045287976400362417, -43.05558670614257721, -15.59869763335051651 ) ) ;
#17634 = CARTESIAN_POINT ( 'NONE',  ( -1.019300379054419947, 38.21680004809164899, -25.26451264419658571 ) ) ;
#17635 = EDGE_CURVE ( 'NONE', #19718, #1416, #18194, .T. ) ;
#17636 = ORIENTED_EDGE ( 'NONE', *, *, #17794, .T. ) ;
#17637 = CARTESIAN_POINT ( 'NONE',  ( -28.13707043255157103, -22.00298671236735615, 6.342158660427235972 ) ) ;
#17638 = CARTESIAN_POINT ( 'NONE',  ( -55.24198130335446422, -0.009170435128244797812, -0.001516807524708348827 ) ) ;
#17639 = CARTESIAN_POINT ( 'NONE',  ( -1.048994561756789512, -43.78680886990931498, 13.42228657661168789 ) ) ;
#17640 = CARTESIAN_POINT ( 'NONE',  ( 2.433796855181205476, -86.69855925934052721, 116.8607839509053434 ) ) ;
#17641 = CARTESIAN_POINT ( 'NONE',  ( -9.156249394959706578, 48.78605533024773422, 24.29252099376439489 ) ) ;
#17642 =( BOUNDED_SURFACE ( )  B_SPLINE_SURFACE ( 3, 1, ( 
 ( #15869, #13699 ),
 ( #2620, #24236 ),
 ( #22053, #13268 ),
 ( #22503, #4491 ) ),
 .UNSPECIFIED., .F., .F., .F. ) 
 B_SPLINE_SURFACE_WITH_KNOTS ( ( 4, 4 ),
 ( 2, 2 ),
 ( 0.000000000000000000, 1.000000000000000000 ),
 ( 0.000000000000000000, 1.000000000000000000 ),
 .UNSPECIFIED. ) 
 GEOMETRIC_REPRESENTATION_ITEM ( )  RATIONAL_B_SPLINE_SURFACE ( (
 ( 1.000000000000000000, 1.000000000000000000),
 ( 0.9934239774497837239, 0.8357310067453919133),
 ( 0.9934239774497837239, 0.8357310067453919133),
 ( 1.000000000000000000, 1.000000000000000000) ) ) 
 REPRESENTATION_ITEM ( '' )  SURFACE ( )  );
#17643 = EDGE_CURVE ( 'NONE', #23985, #11536, #11694, .T. ) ;
#17644 = VECTOR ( 'NONE', #3401, 1000.000000000000227 ) ;
#17645 = EDGE_LOOP ( 'NONE', ( #9462, #19585, #2718, #1279 ) ) ;
#17646 = CARTESIAN_POINT ( 'NONE',  ( 2.430230287190581429, 57.85706160874145354, 133.5180086894993110 ) ) ;
#17647 = CARTESIAN_POINT ( 'NONE',  ( -6.574463467970541153, -38.37705091668347279, 34.08059230520071026 ) ) ;
#17648 = CARTESIAN_POINT ( 'NONE',  ( 28.37603512858456156, 55.80522682147411473, -100.2461737936624218 ) ) ;
#17649 = CARTESIAN_POINT ( 'NONE',  ( 109.1586059443104944, -0.005067816690886790647, 0.004935564877224665227 ) ) ;
#17650 = ORIENTED_EDGE ( 'NONE', *, *, #18486, .F. ) ;
#17651 = CARTESIAN_POINT ( 'NONE',  ( -9.156249394959706578, 25.18996226954685369, 48.32878616080981260 ) ) ;
#17652 = CARTESIAN_POINT ( 'NONE',  ( -22.23226125620929139, -31.55376588768476509, 2.179935373562780221 ) ) ;
#17653 = ORIENTED_EDGE ( 'NONE', *, *, #15595, .T. ) ;
#17654 = CARTESIAN_POINT ( 'NONE',  ( -20.20700224038492721, 0.9908225410478516126, -29.58392382092673145 ) ) ;
#17655 = ORIENTED_EDGE ( 'NONE', *, *, #15448, .T. ) ;
#17656 = CARTESIAN_POINT ( 'NONE',  ( 1.833206308920054539, 85.89457656604029978, -116.9567745381551163 ) ) ;
#17657 = CARTESIAN_POINT ( 'NONE',  ( 1.894214914920945070, 108.5033568857724617, 96.41356089048316846 ) ) ;
#17658 = B_SPLINE_CURVE_WITH_KNOTS ( 'NONE', 3,
 ( #3343, #18451, #27072, #12132, #18605, #7539 ),
 .UNSPECIFIED., .F., .F.,
 ( 4, 2, 4 ),
 ( 3.929062510380680860E-17, 0.0006311571484586211847, 0.001262314296917203338 ),
 .UNSPECIFIED. ) ;
#17659 = ORIENTED_EDGE ( 'NONE', *, *, #24162, .T. ) ;
#17660 = B_SPLINE_CURVE_WITH_KNOTS ( 'NONE', 3,
 ( #10574, #16914, #17040, #10166 ),
 .UNSPECIFIED., .F., .F.,
 ( 4, 4 ),
 ( 3.368494537013313651E-16, 0.01077107486149803464 ),
 .UNSPECIFIED. ) ;
#17661 = CARTESIAN_POINT ( 'NONE',  ( -1.155031165708882979, 35.88345263711048716, -28.62780465193323920 ) ) ;
#17662 = CARTESIAN_POINT ( 'NONE',  ( 25.98107933586720719, 47.01057192495409254, -102.9042679418244290 ) ) ;
#17663 = CARTESIAN_POINT ( 'NONE',  ( 1.833838850093452599, -138.0075868208083421, -44.84137955663364750 ) ) ;
#17664 = CARTESIAN_POINT ( 'NONE',  ( -1.619063947482197729, -2.489035965910479486, -46.30105812165547974 ) ) ;
#17665 = DIRECTION ( 'NONE',  ( -0.5946245182733607137, 0.4749651461092252447, 0.6487139525627731995 ) ) ;
#17666 = EDGE_CURVE ( 'NONE', #28126, #3264, #500, .T. ) ;
#17667 = ORIENTED_EDGE ( 'NONE', *, *, #2186, .T. ) ;
#17668 = CARTESIAN_POINT ( 'NONE',  ( -16.86833981943426153, -20.94590537750580239, 38.94907963570745579 ) ) ;
#17669 = DIRECTION ( 'NONE',  ( 0.7637818620346800147, 0.3617919495470829916, 0.5345501402766235088 ) ) ;
#17670 = CARTESIAN_POINT ( 'NONE',  ( -10.86508079875782151, 46.07061504567116828, 22.20099862734772245 ) ) ;
#17671 = ORIENTED_EDGE ( 'NONE', *, *, #23921, .F. ) ;
#17672 = EDGE_CURVE ( 'NONE', #14341, #17203, #26467, .T. ) ;
#17673 = VERTEX_POINT ( 'NONE', #26127 ) ;
#17674 = ORIENTED_EDGE ( 'NONE', *, *, #23992, .T. ) ;
#17675 = CARTESIAN_POINT ( 'NONE',  ( -23.77929240705188008, 35.93174012244194415, -4.877832571065094491 ) ) ;
#17676 = CARTESIAN_POINT ( 'NONE',  ( 109.1592201516379674, 0.004368284148525261590, -0.006536841731962014269 ) ) ;
#17677 = CARTESIAN_POINT ( 'NONE',  ( 25.64692872815574631, 75.31297890941272044, 84.12425003484072761 ) ) ;
#17678 = CARTESIAN_POINT ( 'NONE',  ( 1.831572820252009626, 59.92262167723438182, 132.1614873090350954 ) ) ;
#17679 = CARTESIAN_POINT ( 'NONE',  ( 1.833721034905635872, 72.24642519953950170, -125.8463597577919586 ) ) ;
#17680 = CARTESIAN_POINT ( 'NONE',  ( 24.01988960052087307, -108.4726924928700527, 73.52806416354032137 ) ) ;
#17681 = ORIENTED_EDGE ( 'NONE', *, *, #22128, .F. ) ;
#17682 = CARTESIAN_POINT ( 'NONE',  ( -21.81686047589429833, -6.867757412720954413, -37.90526371014254892 ) ) ;
#17683 = CARTESIAN_POINT ( 'NONE',  ( -8.259864102781671491, -9.986657004933254811, 52.06232470801721490 ) ) ;
#17684 =( BOUNDED_SURFACE ( )  B_SPLINE_SURFACE ( 3, 1, ( 
 ( #10049, #1392 ),
 ( #23163, #16368 ),
 ( #22875, #14633 ),
 ( #3419, #16814 ) ),
 .UNSPECIFIED., .F., .F., .F. ) 
 B_SPLINE_SURFACE_WITH_KNOTS ( ( 4, 4 ),
 ( 2, 2 ),
 ( 0.000000000000000000, 1.000000000000000000 ),
 ( 0.000000000000000000, 1.000000000000000000 ),
 .UNSPECIFIED. ) 
 GEOMETRIC_REPRESENTATION_ITEM ( )  RATIONAL_B_SPLINE_SURFACE ( (
 ( 1.000000000000000000, 1.000000000000000000),
 ( 0.6386103224230302855, 0.9954351624131538845),
 ( 0.6386103224230302855, 0.9954351624131538845),
 ( 1.000000000000000000, 1.000000000000000000) ) ) 
 REPRESENTATION_ITEM ( '' )  SURFACE ( )  );
#17685 = CARTESIAN_POINT ( 'NONE',  ( 25.64700659047697329, 11.57609179463959848, 112.3162501909140047 ) ) ;
#17686 = CARTESIAN_POINT ( 'NONE',  ( 25.64670758986457955, -112.9099239813695732, -0.4979020485389182848 ) ) ;
#17687 = CARTESIAN_POINT ( 'NONE',  ( 32.73300124599732186, 0.000000000000000000, 0.000000000000000000 ) ) ;
#17688 = CARTESIAN_POINT ( 'NONE',  ( 109.1721716018069657, -0.01567407524362084484, -0.006757465437538735971 ) ) ;
#17689 = VERTEX_POINT ( 'NONE', #13450 ) ;
#17690 = CARTESIAN_POINT ( 'NONE',  ( -20.57838717382308147, 18.89542499756533545, 23.26537097894084383 ) ) ;
#17691 = CARTESIAN_POINT ( 'NONE',  ( 2.433796855181233454, -142.6247129145646397, -28.83182736670683610 ) ) ;
#17692 = ORIENTED_EDGE ( 'NONE', *, *, #16700, .T. ) ;
#17693 = ORIENTED_EDGE ( 'NONE', *, *, #7105, .F. ) ;
#17694 = VERTEX_POINT ( 'NONE', #9140 ) ;
#17695 = B_SPLINE_CURVE_WITH_KNOTS ( 'NONE', 3,
 ( #1687, #23317, #17091, #23184 ),
 .UNSPECIFIED., .F., .F.,
 ( 4, 4 ),
 ( 3.495726066037707399E-16, 0.01077107486149809015 ),
 .UNSPECIFIED. ) ;
#17696 = LINE ( 'NONE', #22169, #25219 ) ;
#17697 = CARTESIAN_POINT ( 'NONE',  ( 109.1586900883932856, 0.006479576224398247292, -0.002995460350188419631 ) ) ;
#17698 = VECTOR ( 'NONE', #9331, 1000.000000000000114 ) ;
#17699 = CARTESIAN_POINT ( 'NONE',  ( 1.833485406944043827, 14.63699153649552365, -144.3694338680883789 ) ) ;
#17700 = ORIENTED_EDGE ( 'NONE', *, *, #6671, .T. ) ;
#17701 = CARTESIAN_POINT ( 'NONE',  ( -55.24728320129491266, 0.01137345571546872526, -0.009072670231975240793 ) ) ;
#17702 = EDGE_CURVE ( 'NONE', #3442, #16646, #15591, .T. ) ;
#17703 = CARTESIAN_POINT ( 'NONE',  ( -1.050230347360791017, -0.0004630652115286125773, 45.79907861464602092 ) ) ;
#17704 = ORIENTED_EDGE ( 'NONE', *, *, #17792, .T. ) ;
#17705 = EDGE_CURVE ( 'NONE', #17579, #7068, #4527, .T. ) ;
#17706 = ORIENTED_EDGE ( 'NONE', *, *, #27970, .F. ) ;
#17707 = ADVANCED_FACE ( 'NONE', ( #24566 ), #16301, .F. ) ;
#17708 = CARTESIAN_POINT ( 'NONE',  ( 2.433796855181205476, -1.451562450950653949, 145.5024947199069629 ) ) ;
#17709 = CARTESIAN_POINT ( 'NONE',  ( 1.833485406944043827, 73.01664920992966756, 125.4007332306548221 ) ) ;
#17710 = DIRECTION ( 'NONE',  ( 1.000000000000000000, -0.000000000000000000, -0.000000000000000000 ) ) ;
#17711 = FACE_OUTER_BOUND ( 'NONE', #5644, .T. ) ;
#17712 = CARTESIAN_POINT ( 'NONE',  ( -55.25719721206881729, 0.009391134844733637840, 0.006045473558784292267 ) ) ;
#17713 = CARTESIAN_POINT ( 'NONE',  ( -6.588769196390754423, -44.25609997968886233, 26.02756986588589072 ) ) ;
#17714 = CARTESIAN_POINT ( 'NONE',  ( -20.20700224038492010, -16.58740185276728241, -24.51628800869040958 ) ) ;
#17715 = CARTESIAN_POINT ( 'NONE',  ( 32.73300124599735739, -99.90245962373877830, 62.10906484417201767 ) ) ;
#17716 = CARTESIAN_POINT ( 'NONE',  ( -24.53237795827005741, 30.86653739599987745, -14.09663893005569513 ) ) ;
#17717 = FACE_OUTER_BOUND ( 'NONE', #10440, .T. ) ;
#17718 = AXIS2_PLACEMENT_3D ( 'NONE', #11809, #14091, #4895 ) ;
#17719 = VERTEX_POINT ( 'NONE', #2804 ) ;
#17720 = ORIENTED_EDGE ( 'NONE', *, *, #28046, .T. ) ;
#17721 = CARTESIAN_POINT ( 'NONE',  ( -22.23226125620944416, 24.24619897613477093, -20.31044300692182603 ) ) ;
#17722 = CARTESIAN_POINT ( 'NONE',  ( 26.04756280548353686, 107.2904246402799799, -36.02883009343526766 ) ) ;
#17723 = ORIENTED_EDGE ( 'NONE', *, *, #11122, .T. ) ;
#17724 =( BOUNDED_SURFACE ( )  B_SPLINE_SURFACE ( 3, 1, ( 
 ( #25796, #19168 ),
 ( #21327, #8108 ),
 ( #12397, #3478 ),
 ( #18742, #6094 ) ),
 .UNSPECIFIED., .F., .F., .F. ) 
 B_SPLINE_SURFACE_WITH_KNOTS ( ( 4, 4 ),
 ( 2, 2 ),
 ( 0.000000000000000000, 1.000000000000000000 ),
 ( 0.000000000000000000, 1.000000000000000000 ),
 .UNSPECIFIED. ) 
 GEOMETRIC_REPRESENTATION_ITEM ( )  RATIONAL_B_SPLINE_SURFACE ( (
 ( 1.000000000000000000, 1.000000000000000000),
 ( 0.7789835883360578528, 0.9689951854195403280),
 ( 0.7789835883360578528, 0.9689951854195403280),
 ( 1.000000000000000000, 1.000000000000000000) ) ) 
 REPRESENTATION_ITEM ( '' )  SURFACE ( )  );
#17725 = ADVANCED_FACE ( 'NONE', ( #20497 ), #19247, .F. ) ;
#17726 = ORIENTED_EDGE ( 'NONE', *, *, #4158, .F. ) ;
#17727 = ORIENTED_EDGE ( 'NONE', *, *, #6909, .F. ) ;
#17728 = EDGE_CURVE ( 'NONE', #9282, #26952, #22723, .T. ) ;
#17729 = CARTESIAN_POINT ( 'NONE',  ( 2.108985857320939239, -145.2876352664462161, 1.281428372375244429 ) ) ;
#17730 = VERTEX_POINT ( 'NONE', #11162 ) ;
#17731 = CARTESIAN_POINT ( 'NONE',  ( 2.430230287190592531, 118.5711603495681459, 84.35270093935295677 ) ) ;
#17732 = EDGE_CURVE ( 'NONE', #4432, #7492, #9296, .T. ) ;
#17733 = B_SPLINE_CURVE_WITH_KNOTS ( 'NONE', 3,
 ( #15927, #5135, #27144, #18521, #5276, #9600 ),
 .UNSPECIFIED., .F., .F.,
 ( 4, 2, 4 ),
 ( 1.607967956875964627E-16, 0.003570751334075640028, 0.007141502668151118727 ),
 .UNSPECIFIED. ) ;
#17734 = B_SPLINE_CURVE_WITH_KNOTS ( 'NONE', 3,
 ( #12351, #5892, #16954, #12081 ),
 .UNSPECIFIED., .F., .F.,
 ( 4, 4 ),
 ( 3.215760458551393353E-16, 0.01077107486149844404 ),
 .UNSPECIFIED. ) ;
#17735 = CARTESIAN_POINT ( 'NONE',  ( -1.044557008772712514, -25.56990300677008676, -37.98985164565319650 ) ) ;
#17736 = FACE_OUTER_BOUND ( 'NONE', #5417, .T. ) ;
#17737 = CARTESIAN_POINT ( 'NONE',  ( -28.13707043255157103, 22.88591869784691113, 0.7675454997507791255 ) ) ;
#17738 = DIRECTION ( 'NONE',  ( -1.000000000000000000, -0.000000000000000000, -0.000000000000000000 ) ) ;
#17739 = CARTESIAN_POINT ( 'NONE',  ( 109.1778270068192853, -0.004958088776550157763, 0.007885345421907784952 ) ) ;
#17740 = CARTESIAN_POINT ( 'NONE',  ( -1.113427685307000203, 12.28784199929934751, -44.18561238466741514 ) ) ;
#17741 = CARTESIAN_POINT ( 'NONE',  ( 109.1586900883932856, 0.0001010081143884156022, -0.007137750914552288065 ) ) ;
#17742 = CARTESIAN_POINT ( 'NONE',  ( 1.833721034905632985, -117.1867194831484511, 85.58110185770060241 ) ) ;
#17743 = ORIENTED_EDGE ( 'NONE', *, *, #1030, .T. ) ;
#17744 = ORIENTED_EDGE ( 'NONE', *, *, #6043, .T. ) ;
#17746 = CARTESIAN_POINT ( 'NONE',  ( 26.11404676487257603, 57.58742681967585497, -97.48350837663548418 ) ) ;
#17745 = CARTESIAN_POINT ( 'NONE',  ( 55.49584447822657296, 69.08290406177579257, 22.16497542184429292 ) ) ;
#17747 = CARTESIAN_POINT ( 'NONE',  ( -1.031422197589716205, -1.530725436377772031, -45.78027046666443312 ) ) ;
#17748 = DIRECTION ( 'NONE',  ( 1.000000000000000000, -6.938893903907226837E-18, 1.734723475976806709E-18 ) ) ;
#17749 = CARTESIAN_POINT ( 'NONE',  ( 25.64670758986457599, 0.4979020485393113038, -112.9099239813695448 ) ) ;
#17750 = CARTESIAN_POINT ( 'NONE',  ( 10.93730112725982373, -142.1801301103788262, 51.37919228020236773 ) ) ;
#17751 = ORIENTED_EDGE ( 'NONE', *, *, #13729, .T. ) ;
#17752 = CARTESIAN_POINT ( 'NONE',  ( 10.93730112726006354, 149.7554878793152966, -20.69552240458195413 ) ) ;
#17753 = VERTEX_POINT ( 'NONE', #26833 ) ;
#17754 = DIRECTION ( 'NONE',  ( 0.000000000000000000, 5.223019709707975211E-21, -1.000000000000000000 ) ) ;
#17755 = CARTESIAN_POINT ( 'NONE',  ( 2.108393763691197353, 141.8460676169243584, 31.45977531353340950 ) ) ;
#17756 = ORIENTED_EDGE ( 'NONE', *, *, #28380, .T. ) ;
#17757 = ORIENTED_EDGE ( 'NONE', *, *, #3260, .F. ) ;
#17758 = CARTESIAN_POINT ( 'NONE',  ( 10.93730112725932635, 0.000000000000000000, 0.000000000000000000 ) ) ;
#17759 = ORIENTED_EDGE ( 'NONE', *, *, #28075, .T. ) ;
#17760 = CARTESIAN_POINT ( 'NONE',  ( 10.93730112725971715, 4.928439153520177030, 151.0983828010091372 ) ) ;
#17761 =( BOUNDED_SURFACE ( )  B_SPLINE_SURFACE ( 3, 1, ( 
 ( #23834, #1921 ),
 ( #21078, #25841 ),
 ( #1364, #28121 ),
 ( #10726, #6136 ) ),
 .UNSPECIFIED., .F., .F., .F. ) 
 B_SPLINE_SURFACE_WITH_KNOTS ( ( 4, 4 ),
 ( 2, 2 ),
 ( 0.000000000000000000, 1.000000000000000000 ),
 ( 0.000000000000000000, 1.000000000000000000 ),
 .UNSPECIFIED. ) 
 GEOMETRIC_REPRESENTATION_ITEM ( )  RATIONAL_B_SPLINE_SURFACE ( (
 ( 1.000000000000000000, 1.000000000000000000),
 ( 0.7789835883360576307, 0.9689951854195403280),
 ( 0.7789835883360576307, 0.9689951854195403280),
 ( 1.000000000000000000, 1.000000000000000000) ) ) 
 REPRESENTATION_ITEM ( '' )  SURFACE ( )  );
#17762 = ORIENTED_EDGE ( 'NONE', *, *, #22501, .T. ) ;
#17763 = CARTESIAN_POINT ( 'NONE',  ( 25.64681081121879203, -83.63051021305848565, -75.86069728269076506 ) ) ;
#17764 = EDGE_CURVE ( 'NONE', #5605, #14867, #21204, .T. ) ;
#17765 = ADVANCED_FACE ( 'NONE', ( #20359 ), #26379, .F. ) ;
#17766 = ORIENTED_EDGE ( 'NONE', *, *, #25673, .F. ) ;
#17767 = CARTESIAN_POINT ( 'NONE',  ( 1.831572820252009626, 97.82994539998382777, 107.1759352627509543 ) ) ;
#17768 = EDGE_CURVE ( 'NONE', #12739, #16696, #3125, .T. ) ;
#17769 = CARTESIAN_POINT ( 'NONE',  ( -1.031422197589711987, -25.67058493451414591, 37.93675465142499803 ) ) ;
#17770 = CARTESIAN_POINT ( 'NONE',  ( 109.1586900883932856, -0.007088091345229661187, 0.0008465529156634868553 ) ) ;
#17771 = CARTESIAN_POINT ( 'NONE',  ( -9.156249394959713683, -48.32878616081028866, -25.18996226954597972 ) ) ;
#17772 = CARTESIAN_POINT ( 'NONE',  ( 2.433796855181205476, 84.34988187690927930, 118.5671979538059730 ) ) ;
#17773 = CARTESIAN_POINT ( 'NONE',  ( 109.1778270068192853, -0.007736698406808940019, -0.005186985107090110077 ) ) ;
#17774 = CARTESIAN_POINT ( 'NONE',  ( 25.64681081121879203, -0.4157506337735756285, 112.9102952884414464 ) ) ;
#17775 = DIRECTION ( 'NONE',  ( 1.000000000000000000, -6.938893903907226837E-18, 1.734723475976806709E-18 ) ) ;
#17776 = ORIENTED_EDGE ( 'NONE', *, *, #23236, .F. ) ;
#17777 = CARTESIAN_POINT ( 'NONE',  ( 1.831572820252008738, 144.4165162501764996, -14.18623102066620412 ) ) ;
#17778 = B_SPLINE_CURVE_WITH_KNOTS ( 'NONE', 3,
 ( #2321, #15418, #6815, #26370, #6674, #24234, #21918, #11124 ),
 .UNSPECIFIED., .F., .F.,
 ( 4, 2, 2, 4 ),
 ( 1.734723475976807094E-18, 0.0002429588503611276103, 0.0004859177007222534859, 0.0009718354014444998161 ),
 .UNSPECIFIED. ) ;
#17779 = CARTESIAN_POINT ( 'NONE',  ( 1.833206310202343925, -30.89799345102857941, -141.7818020564281767 ) ) ;
#17780 = CARTESIAN_POINT ( 'NONE',  ( 2.063896406836609909, -43.61045647697787331, 138.5688025270877120 ) ) ;
#17781 = EDGE_CURVE ( 'NONE', #15925, #20443, #1438, .T. ) ;
#17782 = CARTESIAN_POINT ( 'NONE',  ( 32.73300124599738581, -39.98094346392232268, -110.6325518752277759 ) ) ;
#17783 = ORIENTED_EDGE ( 'NONE', *, *, #27857, .F. ) ;
#17784 = CARTESIAN_POINT ( 'NONE',  ( 16.05277956358206737, -132.7473359121861449, -53.98852998724714780 ) ) ;
#17785 = FACE_OUTER_BOUND ( 'NONE', #1590, .T. ) ;
#17786 = CARTESIAN_POINT ( 'NONE',  ( 30.59141879584284496, -38.47120193631536722, 109.6600586137411852 ) ) ;
#17787 = ORIENTED_EDGE ( 'NONE', *, *, #8070, .T. ) ;
#17788 = EDGE_CURVE ( 'NONE', #20235, #2885, #730, .T. ) ;
#17789 = CARTESIAN_POINT ( 'NONE',  ( 1.833750490713725201, -97.29556423840206492, 107.6587173638742883 ) ) ;
#17790 = ORIENTED_EDGE ( 'NONE', *, *, #19499, .T. ) ;
#17791 = CARTESIAN_POINT ( 'NONE',  ( -55.25719721206881729, 0.007063345920781645762, 0.008651607285661163521 ) ) ;
#17792 = EDGE_CURVE ( 'NONE', #16650, #24385, #3480, .T. ) ;
#17793 = ORIENTED_EDGE ( 'NONE', *, *, #1976, .T. ) ;
#17794 = EDGE_CURVE ( 'NONE', #9920, #4538, #19941, .T. ) ;
#17795 = CARTESIAN_POINT ( 'NONE',  ( -20.20997486282892552, 3.551351076220724598E-15, -29.60348406988233450 ) ) ;
#17796 = CARTESIAN_POINT ( 'NONE',  ( 1.832998868059890096, 117.7096351258398954, -84.86110816369486542 ) ) ;
#17797 = CARTESIAN_POINT ( 'NONE',  ( -20.20997486282892552, 3.551351076220724598E-15, -29.60348406988233450 ) ) ;
#17798 = CARTESIAN_POINT ( 'NONE',  ( -12.94347594948481195, 8.691477019903993906, 47.96504705787742040 ) ) ;
#17799 = VERTEX_POINT ( 'NONE', #22505 ) ;
#17800 = LINE ( 'NONE', #4013, #11578 ) ;
#17801 = CARTESIAN_POINT ( 'NONE',  ( -23.79248802219722592, -7.157555990716680583, 32.40806545715339126 ) ) ;
#17802 = CARTESIAN_POINT ( 'NONE',  ( -1.031422197589716205, 25.67058493451444079, -37.93675465142481329 ) ) ;
#17803 = CARTESIAN_POINT ( 'NONE',  ( -1.056502255334264895, -43.40574022158763512, 14.64009593116146846 ) ) ;
#17804 = ORIENTED_EDGE ( 'NONE', *, *, #16320, .F. ) ;
#17805 = ORIENTED_EDGE ( 'NONE', *, *, #4990, .F. ) ;
#17806 = CARTESIAN_POINT ( 'NONE',  ( -1.046935749539997573, -25.87617179820943036, -37.78548154587986119 ) ) ;
#17807 = LINE ( 'NONE', #24890, #24525 ) ;
#17808 = CARTESIAN_POINT ( 'NONE',  ( -1.259920593601971062, -38.49623866863331045, 25.19630221849093488 ) ) ;
#17809 = CARTESIAN_POINT ( 'NONE',  ( -2.911734481061372115, -36.84482841982624990, 30.23325065583398441 ) ) ;
#17810 = CARTESIAN_POINT ( 'NONE',  ( 25.64670758986456889, -103.3508631837547682, 45.46974729533248194 ) ) ;
#17811 = CARTESIAN_POINT ( 'NONE',  ( -8.786685647604894456, 37.00619870957989832, 38.68584556812258768 ) ) ;
#17812 = ORIENTED_EDGE ( 'NONE', *, *, #24439, .T. ) ;
#17813 = CARTESIAN_POINT ( 'NONE',  ( 32.73300124599734318, 116.5274707358856006, 16.10546300444864443 ) ) ;
#17814 = CARTESIAN_POINT ( 'NONE',  ( -25.21435515916025594, 1.749597353048488237E-16, -4.373993382621220594E-17 ) ) ;
#17815 = CARTESIAN_POINT ( 'NONE',  ( 2.063896406836609909, 145.2631347824382715, -1.344106060020873405 ) ) ;
#17816 = CARTESIAN_POINT ( 'NONE',  ( -25.21435515916042647, 15.02493970636146692, -31.17620025257592786 ) ) ;
#17817 = B_SPLINE_CURVE_WITH_KNOTS ( 'NONE', 3,
 ( #24919, #15972, #18261, #11811, #7076, #24780, #432 ),
 .UNSPECIFIED., .F., .F.,
 ( 4, 3, 4 ),
 ( 6.272338867242750372E-16, 0.02816610861753246486, 0.04000277880656283314 ),
 .UNSPECIFIED. ) ;
#17818 = DIRECTION ( 'NONE',  ( 0.000000000000000000, 5.223019709707975211E-21, -1.000000000000000000 ) ) ;
#17819 = CARTESIAN_POINT ( 'NONE',  ( 109.1586059443104944, -0.003127959656221041516, -0.006344953511159715648 ) ) ;
#17820 = ADVANCED_FACE ( 'NONE', ( #5068 ), #837, .F. ) ;
#17821 = ORIENTED_EDGE ( 'NONE', *, *, #15891, .T. ) ;
#17822 = CARTESIAN_POINT ( 'NONE',  ( 10.93730112725996406, 10.89264110825190457, -150.7858122213661716 ) ) ;
#17823 = CARTESIAN_POINT ( 'NONE',  ( 25.64681081121879203, -107.5125461021400355, -34.49579773461893950 ) ) ;
#17824 = ORIENTED_EDGE ( 'NONE', *, *, #11776, .F. ) ;
#17825 = EDGE_CURVE ( 'NONE', #26529, #1301, #11381, .T. ) ;
#17826 = VERTEX_POINT ( 'NONE', #8247 ) ;
#17827 = VERTEX_POINT ( 'NONE', #19174 ) ;
#17828 = ADVANCED_FACE ( 'NONE', ( #27378 ), #22191, .F. ) ;
#17829 = CARTESIAN_POINT ( 'NONE',  ( 26.11404676487257603, -36.06104232266525145, 107.3263591096429082 ) ) ;
#17830 = CARTESIAN_POINT ( 'NONE',  ( 25.64704443564076897, -23.34498572103240832, -110.4715096490035364 ) ) ;
#17831 = EDGE_CURVE ( 'NONE', #9533, #864, #15820, .T. ) ;
#17832 = CARTESIAN_POINT ( 'NONE',  ( -20.38016308990357217, 16.25718651464982045, -24.94368798801356490 ) ) ;
#17833 = VECTOR ( 'NONE', #6623, 1000.000000000000114 ) ;
#17834 = ORIENTED_EDGE ( 'NONE', *, *, #7292, .T. ) ;
#17835 = FACE_OUTER_BOUND ( 'NONE', #2843, .T. ) ;
#17836 = B_SPLINE_CURVE_WITH_KNOTS ( 'NONE', 3,
 ( #8879, #15601, #17351, #6717, #26278, #8724, #22105, #6576 ),
 .UNSPECIFIED., .F., .F.,
 ( 4, 2, 2, 4 ),
 ( 1.962615573354718958E-17, 0.0002429592666046876293, 0.0004859185332093556345, 0.0009718370664186802609 ),
 .UNSPECIFIED. ) ;
#17837 = LINE ( 'NONE', #434, #23643 ) ;
#17838 = ORIENTED_EDGE ( 'NONE', *, *, #24976, .T. ) ;
#17839 =( BOUNDED_SURFACE ( )  B_SPLINE_SURFACE ( 3, 1, ( 
 ( #28363, #10021 ),
 ( #27708, #23268 ),
 ( #14601, #16630 ),
 ( #8016, #25565 ) ),
 .UNSPECIFIED., .F., .F., .F. ) 
 B_SPLINE_SURFACE_WITH_KNOTS ( ( 4, 4 ),
 ( 2, 2 ),
 ( 0.000000000000000000, 1.000000000000000000 ),
 ( 0.000000000000000000, 1.000000000000000000 ),
 .UNSPECIFIED. ) 
 GEOMETRIC_REPRESENTATION_ITEM ( )  RATIONAL_B_SPLINE_SURFACE ( (
 ( 1.000000000000000000, 1.000000000000000000),
 ( 0.9956975270656955868, 0.8568959468854907557),
 ( 0.9956975270656955868, 0.8568959468854907557),
 ( 1.000000000000000000, 1.000000000000000000) ) ) 
 REPRESENTATION_ITEM ( '' )  SURFACE ( )  );
#17840 = VERTEX_POINT ( 'NONE', #12401 ) ;
#17841 = CARTESIAN_POINT ( 'NONE',  ( 1.894214914920955062, 126.1778046718836066, 71.74757687370502879 ) ) ;
#17842 = CARTESIAN_POINT ( 'NONE',  ( -1.046935749539994465, -37.78548154587976882, 25.87617179820957602 ) ) ;
#17843 = CARTESIAN_POINT ( 'NONE',  ( -1.031422197589716205, 43.06660437151330711, 15.60268798220593389 ) ) ;
#17844 = CARTESIAN_POINT ( 'NONE',  ( 28.37644542392841984, 21.87158679436198483, 122.4011828058665543 ) ) ;
#17845 = CARTESIAN_POINT ( 'NONE',  ( -1.050230347699842692, 1.897926697972695375E-16, 45.79907861674080749 ) ) ;
#17846 = CARTESIAN_POINT ( 'NONE',  ( -23.79223135445719706, 33.03345552685145492, 3.207301057648455966 ) ) ;
#17847 = CARTESIAN_POINT ( 'NONE',  ( 9.884929003653608603, -85.04731144912427965, -124.2095058357586055 ) ) ;
#17848 = CARTESIAN_POINT ( 'NONE',  ( -4.162674018437132695, -41.48630000627035486, 25.90909455705156006 ) ) ;
#17849 = CARTESIAN_POINT ( 'NONE',  ( 1.833691583653538348, 14.81406002961315949, 144.3515375443195694 ) ) ;
#17850 = CARTESIAN_POINT ( 'NONE',  ( 2.108985857320896162, 141.8463279126005432, -31.46042399111103549 ) ) ;
#17851 = CARTESIAN_POINT ( 'NONE',  ( -1.155031165708877872, 38.31525684316177660, 25.28071330859845389 ) ) ;
#17852 = VERTEX_POINT ( 'NONE', #3486 ) ;
#17853 = EDGE_LOOP ( 'NONE', ( #7237, #24847, #2551, #8570 ) ) ;
#17854 = CARTESIAN_POINT ( 'NONE',  ( 25.69398547355841345, 24.20764173643400952, 110.3177996916214596 ) ) ;
#17855 = CARTESIAN_POINT ( 'NONE',  ( -1.239374126674604337, -28.97829083655411964, 35.79060836339844087 ) ) ;
#17856 = VERTEX_POINT ( 'NONE', #1744 ) ;
#17857 = EDGE_CURVE ( 'NONE', #3538, #24090, #10681, .T. ) ;
#17858 = ORIENTED_EDGE ( 'NONE', *, *, #11435, .T. ) ;
#17859 = ORIENTED_EDGE ( 'NONE', *, *, #18700, .F. ) ;
#17860 = CARTESIAN_POINT ( 'NONE',  ( 1.834118845439484335, -85.14950727125780361, -117.5010238212707065 ) ) ;
#17861 = FACE_OUTER_BOUND ( 'NONE', #14359, .T. ) ;
#17862 = EDGE_CURVE ( 'NONE', #22495, #7936, #8279, .T. ) ;
#17863 = EDGE_CURVE ( 'NONE', #24126, #7024, #13406, .T. ) ;
#17864 = CARTESIAN_POINT ( 'NONE',  ( 1.831572820252008738, 125.1738732943810106, 73.40899645746047497 ) ) ;
#17865 = CARTESIAN_POINT ( 'NONE',  ( -1.259920593601968397, -25.19630221849078211, -38.49623866863340993 ) ) ;
#17866 = B_SPLINE_CURVE_WITH_KNOTS ( 'NONE', 3,
 ( #5011, #20980, #16831, #3566, #18980, #10483 ),
 .UNSPECIFIED., .F., .F.,
 ( 4, 2, 4 ),
 ( 0.000000000000000000, 0.0004335184443140195285, 0.0008670368886280390569 ),
 .UNSPECIFIED. ) ;
#17867 = CARTESIAN_POINT ( 'NONE',  ( -20.57838717382308147, 7.715628353033680220, -28.96176188950220975 ) ) ;
#17868 = CARTESIAN_POINT ( 'NONE',  ( 2.108985857320913038, -144.6256801373125427, -13.91228467251966627 ) ) ;
#17869 = CARTESIAN_POINT ( 'NONE',  ( -1.113548883309558368, 42.96943836789127147, 16.03115934825484956 ) ) ;
#17870 = CARTESIAN_POINT ( 'NONE',  ( -1.583189561560252701, 46.33203782964461936, 2.490696082060036343 ) ) ;
#17871 = CARTESIAN_POINT ( 'NONE',  ( -18.41936578851713335, 20.09935324538248480, 37.37524689996173777 ) ) ;
#17872 = CARTESIAN_POINT ( 'NONE',  ( 21.16825799904898986, 97.63815233965183893, -93.85612807858919382 ) ) ;
#17873 = ORIENTED_EDGE ( 'NONE', *, *, #5403, .F. ) ;
#17875 = CARTESIAN_POINT ( 'NONE',  ( -55.24198130335446422, -0.006527480770975599769, 0.006617369590168732142 ) ) ;
#17874 = CARTESIAN_POINT ( 'NONE',  ( -1.239374126674604337, 2.406737988131122830, -45.98822239537607004 ) ) ;
#17876 = CARTESIAN_POINT ( 'NONE',  ( 55.49584447822657296, 29.26468316696863070, -66.38758986585085609 ) ) ;
#17877 = CYLINDRICAL_SURFACE ( 'NONE', #19018, 37.50000000000001421 ) ;
#17878 = CARTESIAN_POINT ( 'NONE',  ( 25.86096068574577700, 0.9975172952974178386, -113.0494979885903604 ) ) ;
#17879 = CARTESIAN_POINT ( 'NONE',  ( 10.93730112725978287, -97.44200844886353252, 115.5857507957700250 ) ) ;
#17880 =( BOUNDED_SURFACE ( )  B_SPLINE_SURFACE ( 3, 1, ( 
 ( #14013, #11725 ),
 ( #18481, #5241 ),
 ( #22971, #25117 ),
 ( #3226, #16029 ) ),
 .UNSPECIFIED., .F., .F., .F. ) 
 B_SPLINE_SURFACE_WITH_KNOTS ( ( 4, 4 ),
 ( 2, 2 ),
 ( 0.000000000000000000, 1.000000000000000000 ),
 ( 0.000000000000000000, 1.000000000000000000 ),
 .UNSPECIFIED. ) 
 GEOMETRIC_REPRESENTATION_ITEM ( )  RATIONAL_B_SPLINE_SURFACE ( (
 ( 1.000000000000000000, 1.000000000000000000),
 ( 0.9934239774497838349, 0.8357310067453913582),
 ( 0.9934239774497838349, 0.8357310067453913582),
 ( 1.000000000000000000, 1.000000000000000000) ) ) 
 REPRESENTATION_ITEM ( '' )  SURFACE ( )  );
#17881 = EDGE_LOOP ( 'NONE', ( #7556, #26531, #15805, #3796 ) ) ;
#17882 = EDGE_LOOP ( 'NONE', ( #23389, #5420, #23077, #1651 ) ) ;
#17883 = CARTESIAN_POINT ( 'NONE',  ( 1.833206308920081185, 117.8322276971147176, -84.68961866582884568 ) ) ;
#17884 = CARTESIAN_POINT ( 'NONE',  ( 2.433796855181219243, 142.0211193075555798, 31.67151202413018396 ) ) ;
#17885 = ORIENTED_EDGE ( 'NONE', *, *, #939, .T. ) ;
#17886 = EDGE_LOOP ( 'NONE', ( #2980, #6004, #9875, #20150 ) ) ;
#17887 = EDGE_CURVE ( 'NONE', #27461, #15570, #2761, .T. ) ;
#17888 = DIRECTION ( 'NONE',  ( 0.7563875759206388771, -0.4122509917856713724, 0.5078650950445698919 ) ) ;
#17889 = ORIENTED_EDGE ( 'NONE', *, *, #21056, .T. ) ;
#17890 = CARTESIAN_POINT ( 'NONE',  ( 26.11404676487257603, 90.92995828888292920, -67.46175819463273626 ) ) ;
#17891 = VERTEX_POINT ( 'NONE', #27948 ) ;
#17892 = EDGE_CURVE ( 'NONE', #9035, #9765, #22121, .T. ) ;
#17893 = EDGE_CURVE ( 'NONE', #2443, #24769, #25113, .T. ) ;
#17894 = CARTESIAN_POINT ( 'NONE',  ( 25.64681081121879203, 66.70335573067866619, 91.10197563707968982 ) ) ;
#17895 = CARTESIAN_POINT ( 'NONE',  ( -1.583189561560256253, 25.21827308671232615, -38.94740041318302559 ) ) ;
#17896 = CARTESIAN_POINT ( 'NONE',  ( 1.834118845439484335, -96.96525081350071673, 107.9567937753789977 ) ) ;
#17897 = CARTESIAN_POINT ( 'NONE',  ( -20.90916690077965256, -34.84883504600963988, -18.74041620980156253 ) ) ;
#17898 = CARTESIAN_POINT ( 'NONE',  ( 10.93730112725990367, -104.7670965581004054, -108.9902118373752842 ) ) ;
#17899 = VECTOR ( 'NONE', #22859, 1000.000000000000114 ) ;
#17900 = CARTESIAN_POINT ( 'NONE',  ( -21.41427618760458174, 19.54551635498129514, -23.81423075802588940 ) ) ;
#17902 = CARTESIAN_POINT ( 'NONE',  ( 26.11404676487257603, -84.89295829319442532, -74.91683232331061504 ) ) ;
#17901 = FACE_OUTER_BOUND ( 'NONE', #20459, .T. ) ;
#17903 = SURFACE_STYLE_USAGE ( .BOTH. , #9147 ) ;
#17904 = B_SPLINE_CURVE_WITH_KNOTS ( 'NONE', 3,
 ( #1274, #25485, #21131, #21417, #21557, #14516, #10624 ),
 .UNSPECIFIED., .F., .F.,
 ( 4, 3, 4 ),
 ( 1.298148181579757605E-17, 0.009512539173626401862, 0.02506242213020844906 ),
 .UNSPECIFIED. ) ;
#17905 = VERTEX_POINT ( 'NONE', #12324 ) ;
#17906 = CARTESIAN_POINT ( 'NONE',  ( 1.832998868059890096, -145.1092030902949830, -0.5339089137762871307 ) ) ;
#17907 = CARTESIAN_POINT ( 'NONE',  ( -1.048996300304503082, -26.29666317565274980, 37.49570739463913327 ) ) ;
#17908 = CARTESIAN_POINT ( 'NONE',  ( -4.780792508754331038, -49.38761389561005188, -3.764354093953405922 ) ) ;
#17909 = LINE ( 'NONE', #22111, #13852 ) ;
#17910 = ADVANCED_FACE ( 'NONE', ( #23859 ), #25145, .F. ) ;
#17911 = CARTESIAN_POINT ( 'NONE',  ( 25.64681081121879203, -34.49579773461710630, -107.5125461021406181 ) ) ;
#17912 = CARTESIAN_POINT ( 'NONE',  ( 21.16825799904900052, -125.4548537968710207, -51.02216409572695710 ) ) ;
#17913 = CARTESIAN_POINT ( 'NONE',  ( -55.24728320129491266, -0.008013189884950039019, 0.01214321324516758234 ) ) ;
#17914 = VERTEX_POINT ( 'NONE', #19099 ) ;
#17915 = CARTESIAN_POINT ( 'NONE',  ( 25.64703792032469920, 110.4127989088533184, -23.62108504469137671 ) ) ;
#17917 = ORIENTED_EDGE ( 'NONE', *, *, #20041, .F. ) ;
#17916 = EDGE_CURVE ( 'NONE', #17673, #12674, #21098, .T. ) ;
#17918 = CIRCLE ( 'NONE', #12870, 151.1787379149930359 ) ;
#17919 = AXIS2_PLACEMENT_3D ( 'NONE', #21589, #6482, #19430 ) ;
#17920 = DIRECTION ( 'NONE',  ( 1.000000000000000000, -6.938893903907226837E-18, 1.734723475976806709E-18 ) ) ;
#17921 = CARTESIAN_POINT ( 'NONE',  ( -1.044556982611269058, -36.05793013899078403, 28.22896456560707534 ) ) ;
#17922 = VECTOR ( 'NONE', #27077, 1000.000000000000000 ) ;
#17923 = ORIENTED_EDGE ( 'NONE', *, *, #17666, .F. ) ;
#17924 = CARTESIAN_POINT ( 'NONE',  ( -55.24728320129491266, 0.01453410071985698077, 0.0006547948648746833647 ) ) ;
#17925 = AXIS2_PLACEMENT_3D ( 'NONE', #11092, #19861, #149 ) ;
#17926 = ORIENTED_EDGE ( 'NONE', *, *, #5675, .T. ) ;
#17927 = CARTESIAN_POINT ( 'NONE',  ( 2.263178113027036531, 86.59154384226330592, -116.7985471375923083 ) ) ;
#17928 = CARTESIAN_POINT ( 'NONE',  ( -24.53237795827028478, -30.86653739599989521, 14.09663893005617119 ) ) ;
#17929 = ORIENTED_EDGE ( 'NONE', *, *, #18959, .T. ) ;
#17930 = B_SPLINE_CURVE_WITH_KNOTS ( 'NONE', 3,
 ( #4121, #17079, #6432, #15183, #12891, #15047, #24005, #13043, #1810, #23736 ),
 .UNSPECIFIED., .F., .F.,
 ( 4, 2, 2, 2, 4 ),
 ( 2.799181570144685938E-16, 0.0003346187017559026423, 0.0006692374035115253436, 0.001003856105267148099, 0.001338474807022770746 ),
 .UNSPECIFIED. ) ;
#17931 =( NAMED_UNIT ( * ) PLANE_ANGLE_UNIT ( ) SI_UNIT ( $, .RADIAN. ) );
#17932 = CARTESIAN_POINT ( 'NONE',  ( -23.79223135445719706, -22.01133905265668034, 24.83942264280426926 ) ) ;
#17933 = CARTESIAN_POINT ( 'NONE',  ( 180.4657679828686980, -1.252232817320263489E-15, 3.130582043300658722E-16 ) ) ;
#17934 = CARTESIAN_POINT ( 'NONE',  ( 10.93730112726024117, 133.3192575531818136, -71.28103789254788580 ) ) ;
#17935 = CARTESIAN_POINT ( 'NONE',  ( 28.37644542392835234, 124.2737818798215699, 4.054996728114629967 ) ) ;
#17936 = CARTESIAN_POINT ( 'NONE',  ( 55.79472521941426777, -23.17337251492811490, 68.96476385670656839 ) ) ;
#17937 = EDGE_LOOP ( 'NONE', ( #1721, #14217, #16613, #13687 ) ) ;
#17938 = CARTESIAN_POINT ( 'NONE',  ( 2.433796855181205476, -31.67151202413066713, 142.0211193075554945 ) ) ;
#17939 = CARTESIAN_POINT ( 'NONE',  ( 8.186469777910929224, -63.89871389959373005, -134.9918587298870705 ) ) ;
#17940 = DIRECTION ( 'NONE',  ( -1.000000000000000000, -0.000000000000000000, -0.000000000000000000 ) ) ;
#17941 = VERTEX_POINT ( 'NONE', #18956 ) ;
#17942 = EDGE_CURVE ( 'NONE', #25430, #10776, #7954, .T. ) ;
#17943 = AXIS2_PLACEMENT_3D ( 'NONE', #1205, #5677, #914 ) ;
#17944 = ORIENTED_EDGE ( 'NONE', *, *, #12313, .T. ) ;
#17945 = CARTESIAN_POINT ( 'NONE',  ( 25.98107933586721074, -90.88151529733741540, -67.37827847766610034 ) ) ;
#17946 = CARTESIAN_POINT ( 'NONE',  ( -7.078251931573400491, -44.92740138729146082, 26.33626633876272649 ) ) ;
#17947 = CARTESIAN_POINT ( 'NONE',  ( -1.583189561560253589, -16.68617981233733616, -43.29471907393735819 ) ) ;
#17948 = VECTOR ( 'NONE', #14045, 1000.000000000000227 ) ;
#17949 = CARTESIAN_POINT ( 'NONE',  ( -1.050230347699842692, 0.0002315326058698765721, -45.79907861674080749 ) ) ;
#17950 = CARTESIAN_POINT ( 'NONE',  ( 10.93730112725990011, -119.3442956573265974, -92.80059208661810999 ) ) ;
#17951 = CARTESIAN_POINT ( 'NONE',  ( 25.86096068574579832, -103.6815822123522821, 45.07009591924524727 ) ) ;
#17952 = CARTESIAN_POINT ( 'NONE',  ( 2.430230287190581429, 71.49654683843510838, 126.7388733285347229 ) ) ;
#17953 = ADVANCED_FACE ( 'NONE', ( #14485 ), #15200, .T. ) ;
#17954 = ORIENTED_EDGE ( 'NONE', *, *, #1341, .T. ) ;
#17955 = CARTESIAN_POINT ( 'NONE',  ( 2.433796855181233454, -142.6247129145646397, -28.83182736670683610 ) ) ;
#17956 = DIRECTION ( 'NONE',  ( 1.000000000000000000, -6.938893903907226837E-18, 1.734723475976806709E-18 ) ) ;
#17957 = VECTOR ( 'NONE', #19677, 1000.000000000000114 ) ;
#17958 = CARTESIAN_POINT ( 'NONE',  ( 2.063896406836605024, -1.344106060021375226, 145.2631347824382715 ) ) ;
#17959 = CARTESIAN_POINT ( 'NONE',  ( 109.1624594426973118, -0.002863932759303199765, 0.01570508117120616304 ) ) ;
#17960 = EDGE_CURVE ( 'NONE', #5605, #207, #13763, .T. ) ;
#17961 = B_SPLINE_CURVE_WITH_KNOTS ( 'NONE', 3,
 ( #13065, #26298, #21562, #2107, #14933, #12912, #13190, #8606 ),
 .UNSPECIFIED., .F., .F.,
 ( 4, 2, 2, 4 ),
 ( 0.000000000000000000, 0.0002429592666046688455, 0.0004859185332093376910, 0.0009718370664186699610 ),
 .UNSPECIFIED. ) ;
#17962 = CARTESIAN_POINT ( 'NONE',  ( 25.64681081121879203, 56.09509703373343115, 97.99105938547943140 ) ) ;
#17963 = VERTEX_POINT ( 'NONE', #23290 ) ;
#17964 = ORIENTED_EDGE ( 'NONE', *, *, #17728, .F. ) ;
#17965 = CARTESIAN_POINT ( 'NONE',  ( 16.05277956358203539, 10.32496049470279154, -142.9335921074871294 ) ) ;
#17966 = VERTEX_POINT ( 'NONE', #25587 ) ;
#17967 = VERTEX_POINT ( 'NONE', #21391 ) ;
#17968 = EDGE_LOOP ( 'NONE', ( #18537, #7759, #3808, #9940 ) ) ;
#17969 = MECHANICAL_DESIGN_GEOMETRIC_PRESENTATION_REPRESENTATION (  '', ( #12904 ), #7888 ) ;
#17970 = FACE_OUTER_BOUND ( 'NONE', #1181, .T. ) ;
#17971 = CARTESIAN_POINT ( 'NONE',  ( 32.73300124599732186, 0.000000000000000000, 0.000000000000000000 ) ) ;
#17972 = VECTOR ( 'NONE', #5254, 999.9999999999998863 ) ;
#17973 = CARTESIAN_POINT ( 'NONE',  ( 109.1589550718174877, 0.002874971999843658425, 0.007008495014548480478 ) ) ;
#17974 = ORIENTED_EDGE ( 'NONE', *, *, #17002, .F. ) ;
#17975 = CARTESIAN_POINT ( 'NONE',  ( -18.41936578851708717, 30.66520733838696344, 29.33493038358041360 ) ) ;
#17976 = CARTESIAN_POINT ( 'NONE',  ( -21.41430102051752016, 11.22990201072317262, 28.68859753627381792 ) ) ;
#17977 = CARTESIAN_POINT ( 'NONE',  ( -20.20700224038492721, -23.35150625415645820, 18.19058640100249491 ) ) ;
#17978 = ORIENTED_EDGE ( 'NONE', *, *, #15448, .F. ) ;
#17979 = EDGE_CURVE ( 'NONE', #18945, #16650, #6912, .T. ) ;
#17980 = CARTESIAN_POINT ( 'NONE',  ( -1.619063947482197729, -25.20140673341345305, 38.92136151114934961 ) ) ;
#17981 = ORIENTED_EDGE ( 'NONE', *, *, #153, .F. ) ;
#17982 = CARTESIAN_POINT ( 'NONE',  ( 2.263178113027063620, 31.59906256848478989, -141.9207360579558497 ) ) ;
#17983 = EDGE_CURVE ( 'NONE', #15703, #27510, #21672, .T. ) ;
#17984 = CARTESIAN_POINT ( 'NONE',  ( 2.433796855181233454, 1.451562450949631211, 145.5024947199069913 ) ) ;
#17985 = DIRECTION ( 'NONE',  ( 0.7637818620346800147, 0.5092696688508698832, 0.3965875333584785167 ) ) ;
#17986 = CARTESIAN_POINT ( 'NONE',  ( -1.048172774974287069, 15.11899685083884393, 43.23017713506509097 ) ) ;
#17987 = CARTESIAN_POINT ( 'NONE',  ( -7.078251931573400491, -51.82710018979479116, -5.101176922830485516 ) ) ;
#17988 = CARTESIAN_POINT ( 'NONE',  ( 6.224689322667647851, -48.18553814189932893, -139.9988794244337384 ) ) ;
#17989 = CARTESIAN_POINT ( 'NONE',  ( -12.94347594948484037, -35.22469990145630447, -33.69581619287863106 ) ) ;
#17990 = CARTESIAN_POINT ( 'NONE',  ( -2.265401668238146815, -25.45016726748341540, -39.53028715828224904 ) ) ;
#17991 = ADVANCED_FACE ( 'NONE', ( #21527 ), #2504, .F. ) ;
#17992 = CARTESIAN_POINT ( 'NONE',  ( 1.833721034905633429, 15.52204855105840409, 144.2772269874176629 ) ) ;
#17993 = B_SPLINE_CURVE_WITH_KNOTS ( 'NONE', 3,
 ( #27719, #8026, #25710, #14610 ),
 .UNSPECIFIED., .F., .F.,
 ( 4, 4 ),
 ( 3.436022625892845483E-16, 0.01077107486149809015 ),
 .UNSPECIFIED. ) ;
#17994 = CARTESIAN_POINT ( 'NONE',  ( -55.24198130335446422, 0.004163123460802997666, 0.008310594958152995454 ) ) ;
#17995 = CARTESIAN_POINT ( 'NONE',  ( 26.04756280548354752, -107.9769918539638098, -33.91579348271626770 ) ) ;
#17996 = ADVANCED_FACE ( 'NONE', ( #2215 ), #13371, .F. ) ;
#17997 = ORIENTED_EDGE ( 'NONE', *, *, #15984, .F. ) ;
#17998 = AXIS2_PLACEMENT_3D ( 'NONE', #159, #6, #11238 ) ;
#17999 = VERTEX_POINT ( 'NONE', #4249 ) ;
#18000 = CARTESIAN_POINT ( 'NONE',  ( 30.59141879584312917, -21.51299111589962365, -114.2039975081484755 ) ) ;
#18001 = CARTESIAN_POINT ( 'NONE',  ( -55.24271866751342941, 0.001425019990782615698, -0.009388511352197861579 ) ) ;
#18002 = ORIENTED_EDGE ( 'NONE', *, *, #6231, .T. ) ;
#18003 = ORIENTED_EDGE ( 'NONE', *, *, #6290, .F. ) ;
#18004 = VERTEX_POINT ( 'NONE', #22393 ) ;
#18005 = CARTESIAN_POINT ( 'NONE',  ( -20.24419206586953379, 29.61012937815439372, -1.282847120831333898 ) ) ;
#18006 = CARTESIAN_POINT ( 'NONE',  ( 26.11404676487257603, 57.58742681967449784, 97.48350837663630841 ) ) ;
#18007 = CARTESIAN_POINT ( 'NONE',  ( -1.583189561560253589, -43.29471907393730135, 16.68617981233748537 ) ) ;
#18008 = B_SPLINE_CURVE_WITH_KNOTS ( 'NONE', 3,
 ( #14354, #18825, #14071, #7916, #16676, #25470, #21687, #1958, #13173, #17639, #28428, #19381, #1813 ),
 .UNSPECIFIED., .F., .F.,
 ( 4, 3, 3, 3, 4 ),
 ( 1.250926888277100303E-17, 0.0007657099931970524301, 0.001531419946797917637, 0.002296279302920158170, 0.003061450627205759400 ),
 .UNSPECIFIED. ) ;
#18009 = CARTESIAN_POINT ( 'NONE',  ( -1.019300379054419725, 45.76814864815091255, -2.023851374322835017 ) ) ;
#18010 = CARTESIAN_POINT ( 'NONE',  ( -8.786685647604892679, -53.04920435127177569, 7.199674155859498548 ) ) ;
#18011 = CIRCLE ( 'NONE', #14805, 12.50000000000000178 ) ;
#18012 = AXIS2_PLACEMENT_3D ( 'NONE', #3289, #5745, #27456 ) ;
#18013 = CARTESIAN_POINT ( 'NONE',  ( 109.1592201516379674, 0.005631912476303814301, -0.005485778713202952607 ) ) ;
#18014 = CARTESIAN_POINT ( 'NONE',  ( 25.64708228042118421, 66.33571787052811430, 91.37028996123288493 ) ) ;
#18015 = CARTESIAN_POINT ( 'NONE',  ( -1.045287976400362417, 43.05558670614268379, 15.59869763335023229 ) ) ;
#18016 = CARTESIAN_POINT ( 'NONE',  ( 16.05277956358211355, 4.672229451527888600, 143.2298391883442719 ) ) ;
#18017 = ADVANCED_FACE ( 'NONE', ( #13453 ), #19581, .F. ) ;
#18018 = B_SPLINE_CURVE_WITH_KNOTS ( 'NONE', 3,
 ( #18373, #25033, #20835, #2701 ),
 .UNSPECIFIED., .F., .F.,
 ( 4, 4 ),
 ( 5.221978698409883944E-16, 0.008383748772659984499 ),
 .UNSPECIFIED. ) ;
#18019 = CARTESIAN_POINT ( 'NONE',  ( 25.70243777736189017, 34.20488708978098913, 107.6443926015131325 ) ) ;
#18020 = LINE ( 'NONE', #22507, #26683 ) ;
#18021 = CARTESIAN_POINT ( 'NONE',  ( 1.833485406944043827, -72.09189602597619739, -125.9346397303442728 ) ) ;
#18022 = CARTESIAN_POINT ( 'NONE',  ( 1.832998868059890096, -30.69214149074107922, 141.8272129421607985 ) ) ;
#18023 = CARTESIAN_POINT ( 'NONE',  ( 1.833691583653495272, -117.6050685739175350, 85.00512109099220481 ) ) ;
#18025 = ORIENTED_EDGE ( 'NONE', *, *, #7824, .F. ) ;
#18024 = EDGE_CURVE ( 'NONE', #21137, #20144, #26269, .T. ) ;
#18026 = B_SPLINE_CURVE_WITH_KNOTS ( 'NONE', 3,
 ( #20979, #26246, #21274, #8694, #1265, #14508 ),
 .UNSPECIFIED., .F., .F.,
 ( 4, 2, 4 ),
 ( 6.505213034913026604E-19, 0.0004335151646191478343, 0.0008670303292382950180 ),
 .UNSPECIFIED. ) ;
#18027 = CARTESIAN_POINT ( 'NONE',  ( -21.41427618760448581, 7.777551129310475098, 29.81030852927058206 ) ) ;
#18028 = FACE_OUTER_BOUND ( 'NONE', #18817, .T. ) ;
#18029 = CARTESIAN_POINT ( 'NONE',  ( 109.1586059443104944, 0.006344953511164428892, 0.003127959656212888750 ) ) ;
#18030 = CARTESIAN_POINT ( 'NONE',  ( 6.224689322667630975, -147.4941644018829265, 12.92299475786910712 ) ) ;
#18031 = CARTESIAN_POINT ( 'NONE',  ( 25.64681081121879203, 83.63051021306002042, -75.86069728268907397 ) ) ;
#18032 = EDGE_LOOP ( 'NONE', ( #28408, #26787, #19947, #9701 ) ) ;
#18033 = CARTESIAN_POINT ( 'NONE',  ( -20.20898977204108604, -0.6607022527615499241, 29.59696883073212703 ) ) ;
#18034 = ORIENTED_EDGE ( 'NONE', *, *, #4213, .T. ) ;
#18035 = CARTESIAN_POINT ( 'NONE',  ( -8.259864102781671491, -22.52209142944967368, -47.98931516265586339 ) ) ;
#18037 = VECTOR ( 'NONE', #11112, 1000.000000000000114 ) ;
#18036 = CARTESIAN_POINT ( 'NONE',  ( 25.70243777736188306, -12.53519966262558860, 112.2504268534933800 ) ) ;
#18038 = ORIENTED_EDGE ( 'NONE', *, *, #23369, .T. ) ;
#18039 = CARTESIAN_POINT ( 'NONE',  ( 26.11404676487259024, 24.64483677384848903, 110.5078194225162207 ) ) ;
#18040 = EDGE_CURVE ( 'NONE', #9315, #1788, #24410, .T. ) ;
#18041 = AXIS2_PLACEMENT_3D ( 'NONE', #6819, #15564, #24375 ) ;
#18042 = EDGE_LOOP ( 'NONE', ( #18780, #15629, #16080, #16947 ) ) ;
#18043 = CARTESIAN_POINT ( 'NONE',  ( 1.833838850093427730, -97.09738632348962994, -107.8375672471893125 ) ) ;
#18044 = CONICAL_SURFACE ( 'NONE', #4740, 117.6351876552689504, 0.9945805576725580410 ) ;
#18045 = ORIENTED_EDGE ( 'NONE', *, *, #3479, .T. ) ;
#18046 = ORIENTED_EDGE ( 'NONE', *, *, #27328, .T. ) ;
#18047 = CARTESIAN_POINT ( 'NONE',  ( 13.36082413113063083, 22.28175172543560123, 151.2941478187908615 ) ) ;
#18048 = CARTESIAN_POINT ( 'NONE',  ( -10.86508079875781085, 50.32133009257468359, -9.118642906269416315 ) ) ;
#18049 = B_SPLINE_CURVE_WITH_KNOTS ( 'NONE', 3,
 ( #2450, #24078, #22032, #11242, #17423, #2296, #297, #15686, #4767, #12969 ),
 .UNSPECIFIED., .F., .F.,
 ( 4, 2, 2, 2, 4 ),
 ( 7.757919228897728493E-18, 0.0003346267210630983675, 0.0006692534421261890371, 0.001003880163189279761, 0.001338506884252370268 ),
 .UNSPECIFIED. ) ;
#18050 = VECTOR ( 'NONE', #12709, 1000.000000000000114 ) ;
#18051 = CARTESIAN_POINT ( 'NONE',  ( -1.046935749540007343, -12.93334586714209777, -43.93230528057176798 ) ) ;
#18052 = CARTESIAN_POINT ( 'NONE',  ( 13.84597867724965070, 121.4327876424627988, -82.31427113894673653 ) ) ;
#18053 = CARTESIAN_POINT ( 'NONE',  ( -1.031422197589711764, -28.14735071801717226, 36.13727897780157150 ) ) ;
#18054 = EDGE_CURVE ( 'NONE', #9521, #4937, #21676, .T. ) ;
#18056 =( BOUNDED_SURFACE ( )  B_SPLINE_SURFACE ( 3, 1, ( 
 ( #17065, #1661 ),
 ( #27574, #7893 ),
 ( #13027, #28273 ),
 ( #11018, #2357 ) ),
 .UNSPECIFIED., .F., .F., .F. ) 
 B_SPLINE_SURFACE_WITH_KNOTS ( ( 4, 4 ),
 ( 2, 2 ),
 ( 0.000000000000000000, 1.000000000000000000 ),
 ( 0.000000000000000000, 1.000000000000000000 ),
 .UNSPECIFIED. ) 
 GEOMETRIC_REPRESENTATION_ITEM ( )  RATIONAL_B_SPLINE_SURFACE ( (
 ( 1.000000000000000000, 1.000000000000000000),
 ( 0.9934239774497838349, 0.8357310067453913582),
 ( 0.9934239774497838349, 0.8357310067453913582),
 ( 1.000000000000000000, 1.000000000000000000) ) ) 
 REPRESENTATION_ITEM ( '' )  SURFACE ( )  );
#18055 = CIRCLE ( 'NONE', #1530, 151.1787379149930359 ) ;
#18057 = CARTESIAN_POINT ( 'NONE',  ( 32.73300124599735739, -110.6325518752276622, 39.98094346392273479 ) ) ;
#18058 = CARTESIAN_POINT ( 'NONE',  ( 32.73300124599738581, 99.90245962373917621, -62.10906484417127871 ) ) ;
#18059 = VECTOR ( 'NONE', #6602, 1000.000000000000000 ) ;
#18060 = EDGE_CURVE ( 'NONE', #23596, #733, #357, .T. ) ;
#18061 = ORIENTED_EDGE ( 'NONE', *, *, #5397, .T. ) ;
#18062 = CARTESIAN_POINT ( 'NONE',  ( 25.64681081121879203, 103.3177883989779531, 45.54494737132259274 ) ) ;
#18063 = CIRCLE ( 'NONE', #4284, 151.1787379149930359 ) ;
#18064 = CARTESIAN_POINT ( 'NONE',  ( 25.64681081121879203, 66.70335573067988832, -91.10197563707880875 ) ) ;
#18065 = EDGE_CURVE ( 'NONE', #8156, #25619, #21819, .T. ) ;
#18066 = CARTESIAN_POINT ( 'NONE',  ( 28.43349137099830415, -119.3601175884732868, -34.52178142065654498 ) ) ;
#18067 = CARTESIAN_POINT ( 'NONE',  ( 1.894214914920948400, 86.08679174688076330, 116.8658096527525743 ) ) ;
#18068 = ORIENTED_EDGE ( 'NONE', *, *, #5609, .F. ) ;
#18069 = CARTESIAN_POINT ( 'NONE',  ( -25.21435515916043713, -34.05351380035328646, 6.169479169075816394 ) ) ;
#18070 = CARTESIAN_POINT ( 'NONE',  ( 25.98107933586721074, 110.8834224379717313, -22.45325949158369738 ) ) ;
#18071 = B_SPLINE_CURVE_WITH_KNOTS ( 'NONE', 3,
 ( #27792, #12517, #19149, #16561 ),
 .UNSPECIFIED., .F., .F.,
 ( 4, 4 ),
 ( 2.432574717070327228E-16, 0.008383748772659696535 ),
 .UNSPECIFIED. ) ;
#18072 = CARTESIAN_POINT ( 'NONE',  ( 1.831572820252008738, 45.77972211429995752, -137.7011124121612795 ) ) ;
#18073 = ORIENTED_EDGE ( 'NONE', *, *, #18379, .T. ) ;
#18074 = CARTESIAN_POINT ( 'NONE',  ( 32.73300124599740002, 66.00340565729470654, -97.37344512919790418 ) ) ;
#18075 = ORIENTED_EDGE ( 'NONE', *, *, #18040, .F. ) ;
#18076 = B_SPLINE_CURVE_WITH_KNOTS ( 'NONE', 3,
 ( #18409, #25062, #27186, #2732, #9800, #15833 ),
 .UNSPECIFIED., .F., .F.,
 ( 4, 2, 4 ),
 ( 1.390486644391990834E-17, 0.0006311571484586102343, 0.001262314296917206808 ),
 .UNSPECIFIED. ) ;
#18077 = B_SPLINE_CURVE_WITH_KNOTS ( 'NONE', 3,
 ( #3596, #1585, #20729, #18864, #3177, #23206, #16420 ),
 .UNSPECIFIED., .F., .F.,
 ( 4, 3, 4 ),
 ( 5.901834185273117976E-16, 0.02816610861753246139, 0.04000277880656281926 ),
 .UNSPECIFIED. ) ;
#18078 = CARTESIAN_POINT ( 'NONE',  ( 16.05277956358202829, -141.9568301782830986, 19.61822947415926066 ) ) ;
#18079 = CARTESIAN_POINT ( 'NONE',  ( -20.57838717382308147, -29.92853265176832878, -1.611677988432255848 ) ) ;
#18080 = CARTESIAN_POINT ( 'NONE',  ( -1.058197053496162665, 45.77356582045591438, 1.754224732379708662 ) ) ;
#18081 = ORIENTED_EDGE ( 'NONE', *, *, #23818, .F. ) ;
#18083 = EDGE_CURVE ( 'NONE', #18556, #23588, #11995, .T. ) ;
#18082 = CARTESIAN_POINT ( 'NONE',  ( 109.1778270068192853, -0.007152128381194093436, 0.005967275455169858585 ) ) ;
#18084 = EDGE_LOOP ( 'NONE', ( #16082, #18913, #8110, #7353 ) ) ;
#18085 = CARTESIAN_POINT ( 'NONE',  ( 24.01988960052063149, -117.9135177031533033, -57.17607523395325586 ) ) ;
#18086 = ORIENTED_EDGE ( 'NONE', *, *, #27529, .F. ) ;
#18087 = DIRECTION ( 'NONE',  ( 0.000000000000000000, 0.000000000000000000, -1.000000000000000000 ) ) ;
#18088 = CARTESIAN_POINT ( 'NONE',  ( 1.833485406944043827, 85.72460230293692973, 117.0814567582547596 ) ) ;
#18089 = CARTESIAN_POINT ( 'NONE',  ( 25.64703792032468854, -34.74993974077031567, 107.4308312803557470 ) ) ;
#18090 = DIRECTION ( 'NONE',  ( 0.000000000000000000, -5.223019709708116647E-21, 1.000000000000000000 ) ) ;
#18091 = EDGE_CURVE ( 'NONE', #27787, #15270, #6616, .T. ) ;
#18092 = ORIENTED_EDGE ( 'NONE', *, *, #10275, .F. ) ;
#18093 = B_SPLINE_CURVE_WITH_KNOTS ( 'NONE', 3,
 ( #4197, #21767, #25681, #2030, #14576, #8662, #23805, #14859, #17291, #3785 ),
 .UNSPECIFIED., .F., .F.,
 ( 4, 2, 2, 2, 4 ),
 ( 2.847672227753435151E-16, 0.0003346187017559057865, 0.0006692374035115268615, 0.001003856105267147665, 0.001338474807022768795 ),
 .UNSPECIFIED. ) ;
#18094 = EDGE_CURVE ( 'NONE', #13886, #14457, #24315, .T. ) ;
#18095 = CARTESIAN_POINT ( 'NONE',  ( 19.66333377628695089, -60.10102584214464372, 123.9466021833771947 ) ) ;
#18096 = CARTESIAN_POINT ( 'NONE',  ( -1.056502255334265339, 27.33667001641170557, -36.75727364034741385 ) ) ;
#18097 = CARTESIAN_POINT ( 'NONE',  ( 10.93730112725990011, -146.7718404940640653, -36.23586118136687162 ) ) ;
#18098 = EDGE_LOOP ( 'NONE', ( #18280, #20251, #6245, #14163 ) ) ;
#18099 = ORIENTED_EDGE ( 'NONE', *, *, #21940, .F. ) ;
#18100 = CARTESIAN_POINT ( 'NONE',  ( 25.64681081121879203, -91.10197563707900770, -66.70335573067958990 ) ) ;
#18101 = CARTESIAN_POINT ( 'NONE',  ( 25.64692232868534560, 75.79483800045773023, 83.69035111837229124 ) ) ;
#18102 = CARTESIAN_POINT ( 'NONE',  ( -1.031422197589716205, 36.13727897780129439, -28.14735071801756661 ) ) ;
#18103 = CARTESIAN_POINT ( 'NONE',  ( -55.24340739397742084, 0.008612749836246956503, -0.005344433640973183380 ) ) ;
#18104 = CARTESIAN_POINT ( 'NONE',  ( 25.64700659047694487, -84.06149911284495602, 75.38309044531857239 ) ) ;
#18105 = CARTESIAN_POINT ( 'NONE',  ( 1.831572820252008738, 71.69925593429807975, 126.1609924456732159 ) ) ;
#18106 = ORIENTED_EDGE ( 'NONE', *, *, #28134, .F. ) ;
#18107 = CARTESIAN_POINT ( 'NONE',  ( 26.11404676487257603, 102.9690087468801352, 47.08215554553553517 ) ) ;
#18108 = CARTESIAN_POINT ( 'NONE',  ( -1.045287976400383290, 36.12803364096649972, 28.14015102489766917 ) ) ;
#18109 = CARTESIAN_POINT ( 'NONE',  ( 10.93730112725943471, 133.3192575531795683, 71.28103789254991796 ) ) ;
#18110 = DIRECTION ( 'NONE',  ( -5.541455922705464902E-20, 5.223019709708320524E-21, -1.000000000000000000 ) ) ;
#18111 = CARTESIAN_POINT ( 'NONE',  ( 32.73300124599735739, -51.32617430724984331, 105.8473486001049224 ) ) ;
#18112 = CARTESIAN_POINT ( 'NONE',  ( 2.263178607246659091, 142.5035407554795199, 28.85718361840967461 ) ) ;
#18113 = ORIENTED_EDGE ( 'NONE', *, *, #20410, .F. ) ;
#18114 = B_SPLINE_CURVE_WITH_KNOTS ( 'NONE', 3,
 ( #685, #16225, #9178, #20400 ),
 .UNSPECIFIED., .F., .F.,
 ( 4, 4 ),
 ( 1.211825722864169544E-16, 0.008383748772659583778 ),
 .UNSPECIFIED. ) ;
#18115 = EDGE_CURVE ( 'NONE', #27090, #18454, #27633, .T. ) ;
#18116 = CARTESIAN_POINT ( 'NONE',  ( 2.433796855181233454, 133.5135467655518369, 57.85512797797937168 ) ) ;
#18117 = VERTEX_POINT ( 'NONE', #13208 ) ;
#18118 = CARTESIAN_POINT ( 'NONE',  ( 32.73300124599734318, 116.5274707358856006, 16.10546300444864443 ) ) ;
#18119 = CARTESIAN_POINT ( 'NONE',  ( -1.619063947482197729, 11.94059994246222622, 44.80407745103770623 ) ) ;
#18120 = EDGE_LOOP ( 'NONE', ( #1374, #1232, #20115, #8231 ) ) ;
#18121 = ORIENTED_EDGE ( 'NONE', *, *, #3422, .T. ) ;
#18122 = ORIENTED_EDGE ( 'NONE', *, *, #13703, .F. ) ;
#18123 = CARTESIAN_POINT ( 'NONE',  ( -25.21435515916043002, 4.655591116594353984, -34.29329011225956947 ) ) ;
#18124 = EDGE_CURVE ( 'NONE', #21826, #27931, #20231, .T. ) ;
#18125 = CARTESIAN_POINT ( 'NONE',  ( 109.1587776205901861, -0.006388631651935916360, -0.003592288931003330757 ) ) ;
#18126 = EDGE_CURVE ( 'NONE', #22671, #24458, #23036, .T. ) ;
#18127 = CARTESIAN_POINT ( 'NONE',  ( -22.34422965417122597, 16.46028608106157876, 34.15536449444073241 ) ) ;
#18128 = CARTESIAN_POINT ( 'NONE',  ( -20.20700224038492365, 23.35150625415685255, 18.19058640100197977 ) ) ;
#18129 = ORIENTED_EDGE ( 'NONE', *, *, #555, .F. ) ;
#18130 = CARTESIAN_POINT ( 'NONE',  ( -10.86508079875779842, 36.95527278096579948, 35.35100740321738044 ) ) ;
#18131 = CARTESIAN_POINT ( 'NONE',  ( -23.79248802219728276, 13.25839849636400203, 30.42578156345371454 ) ) ;
#18132 = CARTESIAN_POINT ( 'NONE',  ( -20.20700224038492721, -29.58392382092674211, -0.9908225410477480288 ) ) ;
#18133 = ORIENTED_EDGE ( 'NONE', *, *, #22200, .T. ) ;
#18134 = VERTEX_POINT ( 'NONE', #12934 ) ;
#18135 = CARTESIAN_POINT ( 'NONE',  ( 109.1778270068192853, -0.008960903982066578330, -0.002542344697966412732 ) ) ;
#18136 = CARTESIAN_POINT ( 'NONE',  ( 2.433796855181205476, 13.76554153471693454, 144.8571464219890004 ) ) ;
#18137 = CARTESIAN_POINT ( 'NONE',  ( -2.911734481061404534, -2.802366807346520439, -47.57875121082949477 ) ) ;
#18138 = CARTESIAN_POINT ( 'NONE',  ( -1.045287976400365970, 15.59869763335156101, 43.05558670614217931 ) ) ;
#18139 = CARTESIAN_POINT ( 'NONE',  ( -21.41427618760446094, 30.75468365310879193, 1.815001260755948254 ) ) ;
#18140 = CARTESIAN_POINT ( 'NONE',  ( 109.1592201516379674, -0.001934867487012880598, 0.007620268632968135725 ) ) ;
#18141 = CARTESIAN_POINT ( 'NONE',  ( -1.155001620486259206, 44.25209926692307505, -12.20337535396694051 ) ) ;
#18142 = DIRECTION ( 'NONE',  ( 0.000000000000000000, 0.000000000000000000, 1.000000000000000000 ) ) ;
#18143 = CARTESIAN_POINT ( 'NONE',  ( -1.019300379054419947, -16.06793277091962935, 42.90269154183443590 ) ) ;
#18144 = CARTESIAN_POINT ( 'NONE',  ( 2.433796855181205476, 125.2830755159753977, 74.00833731765604284 ) ) ;
#18145 = CARTESIAN_POINT ( 'NONE',  ( 2.433796855181205476, -142.6247129145649808, 28.83182736670489987 ) ) ;
#18146 = ORIENTED_EDGE ( 'NONE', *, *, #14456, .F. ) ;
#18147 = CARTESIAN_POINT ( 'NONE',  ( 2.263178113027049410, -96.24282436106540217, -108.9830942735803063 ) ) ;
#18148 = ORIENTED_EDGE ( 'NONE', *, *, #1314, .T. ) ;
#18149 = ORIENTED_EDGE ( 'NONE', *, *, #19778, .T. ) ;
#18150 = VECTOR ( 'NONE', #112, 1000.000000000000341 ) ;
#18151 = ORIENTED_EDGE ( 'NONE', *, *, #26899, .T. ) ;
#18152 = EDGE_CURVE ( 'NONE', #27648, #18231, #23692, .T. ) ;
#18153 = EDGE_CURVE ( 'NONE', #4864, #17580, #17480, .T. ) ;
#18154 = CARTESIAN_POINT ( 'NONE',  ( -1.046935749539993799, 43.14401153755488849, 15.35946454248350435 ) ) ;
#18155 = CARTESIAN_POINT ( 'NONE',  ( -1.239374126674604337, 2.406737988131765871, 45.98822239537605583 ) ) ;
#18156 = EDGE_CURVE ( 'NONE', #10460, #26876, #14081, .T. ) ;
#18157 = CARTESIAN_POINT ( 'NONE',  ( 1.831572820252008738, -144.4165162501764144, 14.18623102066721664 ) ) ;
#18158 = B_SPLINE_CURVE_WITH_KNOTS ( 'NONE', 3,
 ( #5950, #23930, #6232, #1884, #19173, #12821, #16883, #14852, #21608, #8111 ),
 .UNSPECIFIED., .F., .F.,
 ( 4, 3, 3, 4 ),
 ( 5.594315114139762021E-17, 0.0002669559177086202858, 0.0005339118354150952607, 0.001067817517169147769 ),
 .UNSPECIFIED. ) ;
#18159 = FACE_OUTER_BOUND ( 'NONE', #26910, .T. ) ;
#18160 = ADVANCED_FACE ( 'NONE', ( #20406 ), #22597, .T. ) ;
#18161 = CARTESIAN_POINT ( 'NONE',  ( -1.058197053496165108, -15.81317659443655721, 42.99116279335168400 ) ) ;
#18162 = CARTESIAN_POINT ( 'NONE',  ( 1.833838848569444124, 132.6367525013577051, 58.85887272891235966 ) ) ;
#18163 = CARTESIAN_POINT ( 'NONE',  ( 2.263178607246685736, -133.3897506477018169, -57.85473702627246695 ) ) ;
#18164 = CARTESIAN_POINT ( 'NONE',  ( 1.894214914920938408, 59.90782071839196021, 132.2104617488239455 ) ) ;
#18165 = CARTESIAN_POINT ( 'NONE',  ( -22.23342874802668234, -16.78332232459660389, -26.81018246605532340 ) ) ;
#18166 = CARTESIAN_POINT ( 'NONE',  ( -1.045287976400365970, -45.76855895860947498, -1.530335034933654859 ) ) ;
#18167 = VERTEX_POINT ( 'NONE', #7046 ) ;
#18168 = CARTESIAN_POINT ( 'NONE',  ( -20.21097721650786738, -24.14932365326965069, -17.13687097598128517 ) ) ;
#18169 = DIRECTION ( 'NONE',  ( -1.000000000000000000, -0.000000000000000000, -0.000000000000000000 ) ) ;
#18170 = CARTESIAN_POINT ( 'NONE',  ( 19.66333377628715340, 84.55762186019687476, -108.7423656420548213 ) ) ;
#18171 = CARTESIAN_POINT ( 'NONE',  ( 2.430230287190572103, -144.8619874886007892, 13.76600171652595428 ) ) ;
#18172 = CARTESIAN_POINT ( 'NONE',  ( 6.224689322667647851, 111.7293398381264922, 97.14981701196357733 ) ) ;
#18173 = ORIENTED_EDGE ( 'NONE', *, *, #17410, .F. ) ;
#18174 = CARTESIAN_POINT ( 'NONE',  ( 6.224689322667647851, 148.0369967195762797, -2.565137105444267540 ) ) ;
#18175 = ORIENTED_EDGE ( 'NONE', *, *, #5165, .F. ) ;
#18176 = CARTESIAN_POINT ( 'NONE',  ( -7.711401346138392121, -21.83927363365067364, -47.70038152767084227 ) ) ;
#18177 = CARTESIAN_POINT ( 'NONE',  ( 32.73300124599735739, -103.7392577722179823, 55.46353551261974957 ) ) ;
#18178 = ORIENTED_EDGE ( 'NONE', *, *, #13947, .F. ) ;
#18179 = B_SPLINE_CURVE_WITH_KNOTS ( 'NONE', 3,
 ( #17008, #12402, #14987, #8392, #23802, #23374, #25803 ),
 .UNSPECIFIED., .F., .F.,
 ( 4, 3, 4 ),
 ( 0.000000000000000000, 0.006568092053401790135, 0.02506242213020847681 ),
 .UNSPECIFIED. ) ;
#18180 = CARTESIAN_POINT ( 'NONE',  ( -22.23342874802667879, -29.33662284748868387, -11.82490389046302859 ) ) ;
#18181 = ORIENTED_EDGE ( 'NONE', *, *, #27970, .T. ) ;
#18182 = B_SPLINE_CURVE_WITH_KNOTS ( 'NONE', 3,
 ( #26113, #23977, #15299, #23836, #15153, #6400, #6269, #6546 ),
 .UNSPECIFIED., .F., .F.,
 ( 4, 2, 2, 4 ),
 ( 0.000000000000000000, 0.002761524886576648477, 0.005523049773153296954, 0.01104609954630659391 ),
 .UNSPECIFIED. ) ;
#18183 = ORIENTED_EDGE ( 'NONE', *, *, #1183, .F. ) ;
#18184 = EDGE_CURVE ( 'NONE', #9343, #6084, #830, .T. ) ;
#18185 = ADVANCED_FACE ( 'NONE', ( #24612 ), #12594, .F. ) ;
#18186 = ORIENTED_EDGE ( 'NONE', *, *, #28040, .T. ) ;
#18187 = CARTESIAN_POINT ( 'NONE',  ( 2.433796855181233454, 13.76554153471886366, -144.8571464219887730 ) ) ;
#18188 = ADVANCED_FACE ( 'NONE', ( #690 ), #978, .F. ) ;
#18189 = FACE_OUTER_BOUND ( 'NONE', #11816, .T. ) ;
#18190 = CARTESIAN_POINT ( 'NONE',  ( 2.108393763691160494, 137.7805780486507103, 46.11438684123211118 ) ) ;
#18191 = CARTESIAN_POINT ( 'NONE',  ( 1.833838848569417257, 30.34409872482234860, 141.9017642089166600 ) ) ;
#18192 = CARTESIAN_POINT ( 'NONE',  ( 1.833691583653550783, -72.24637705290399481, -125.8462703805706440 ) ) ;
#18193 = CARTESIAN_POINT ( 'NONE',  ( 32.73300124599732186, 0.000000000000000000, 0.000000000000000000 ) ) ;
#18194 = B_SPLINE_CURVE_WITH_KNOTS ( 'NONE', 3,
 ( #4392, #8573, #27999, #8712, #8441, #8298 ),
 .UNSPECIFIED., .F., .F.,
 ( 4, 2, 4 ),
 ( 0.000000000000000000, 0.0004335151646191501111, 0.0008670303292383002222 ),
 .UNSPECIFIED. ) ;
#18195 = FACE_OUTER_BOUND ( 'NONE', #19687, .T. ) ;
#18196 = CARTESIAN_POINT ( 'NONE',  ( 26.11404676487257603, -1.130420376097928115, 113.2169081140373947 ) ) ;
#18197 = CARTESIAN_POINT ( 'NONE',  ( 25.64681081121879203, 83.63051021305903987, 75.86069728269016821 ) ) ;
#18198 = ORIENTED_EDGE ( 'NONE', *, *, #22245, .T. ) ;
#18199 = CARTESIAN_POINT ( 'NONE',  ( -55.24271866751342941, -0.004365563123935077734, -0.008433070970613952902 ) ) ;
#18201 = CARTESIAN_POINT ( 'NONE',  ( 26.11404676487257603, 45.01677474591409833, 103.8885755249570906 ) ) ;
#18200 = CARTESIAN_POINT ( 'NONE',  ( -1.045287976400351981, 36.12803364096590997, -28.14015102489844011 ) ) ;
#18202 = CARTESIAN_POINT ( 'NONE',  ( 1.894214914920928416, 0.9536781033360174353, 145.1469726764545385 ) ) ;
#18203 = CARTESIAN_POINT ( 'NONE',  ( 10.93730112725932635, 0.000000000000000000, 0.000000000000000000 ) ) ;
#18204 = DIRECTION ( 'NONE',  ( 0.7637818620346801257, 0.5345501402766276167, -0.3617919495470772184 ) ) ;
#18205 = EDGE_LOOP ( 'NONE', ( #23792, #8389, #13161, #8787 ) ) ;
#18206 = CARTESIAN_POINT ( 'NONE',  ( 5.340103556456485379, -47.74933482044465194, 139.5040934094288616 ) ) ;
#18207 = CARTESIAN_POINT ( 'NONE',  ( 109.1586059443104944, -0.007058870754606105975, 0.0004635842312890713491 ) ) ;
#18208 = CARTESIAN_POINT ( 'NONE',  ( 30.58324630866342630, -87.19147450740413774, 83.81536267638921345 ) ) ;
#18209 = ORIENTED_EDGE ( 'NONE', *, *, #12803, .T. ) ;
#18210 = CARTESIAN_POINT ( 'NONE',  ( 25.64692872815577473, 75.79105864157502026, -83.69378511050487646 ) ) ;
#18211 = ORIENTED_EDGE ( 'NONE', *, *, #18851, .F. ) ;
#18212 = CARTESIAN_POINT ( 'NONE',  ( -1.323439229708125886, 2.317790194800380288, 46.01398008004440499 ) ) ;
#18213 = CARTESIAN_POINT ( 'NONE',  ( -25.21435515916025594, 1.749597353048488237E-16, -4.373993382621220594E-17 ) ) ;
#18214 = EDGE_CURVE ( 'NONE', #7707, #19215, #19223, .T. ) ;
#18215 = DIRECTION ( 'NONE',  ( 0.000000000000000000, 0.000000000000000000, 1.000000000000000000 ) ) ;
#18216 = VERTEX_POINT ( 'NONE', #9479 ) ;
#18217 = EDGE_CURVE ( 'NONE', #22553, #27179, #9715, .T. ) ;
#18218 = LINE ( 'NONE', #7452, #26262 ) ;
#18219 = VERTEX_POINT ( 'NONE', #5436 ) ;
#18220 = EDGE_CURVE ( 'NONE', #22412, #709, #21280, .T. ) ;
#18221 =( BOUNDED_SURFACE ( )  B_SPLINE_SURFACE ( 3, 1, ( 
 ( #19951, #511 ),
 ( #20512, #17780 ),
 ( #15913, #15604 ),
 ( #4970, #24852 ) ),
 .UNSPECIFIED., .F., .F., .F. ) 
 B_SPLINE_SURFACE_WITH_KNOTS ( ( 4, 4 ),
 ( 2, 2 ),
 ( 0.000000000000000000, 1.000000000000000000 ),
 ( 0.000000000000000000, 1.000000000000000000 ),
 .UNSPECIFIED. ) 
 GEOMETRIC_REPRESENTATION_ITEM ( )  RATIONAL_B_SPLINE_SURFACE ( (
 ( 1.000000000000000000, 1.000000000000000000),
 ( 0.9956975270656954757, 0.8568959468854893125),
 ( 0.9956975270656954757, 0.8568959468854893125),
 ( 1.000000000000000000, 1.000000000000000000) ) ) 
 REPRESENTATION_ITEM ( '' )  SURFACE ( )  );
#18222 = CARTESIAN_POINT ( 'NONE',  ( 32.73300124599734318, 81.52272205837205377, 84.80615050150403533 ) ) ;
#18223 = CARTESIAN_POINT ( 'NONE',  ( -8.786685647604898008, 38.68584556812353981, 37.00619870957891777 ) ) ;
#18224 = DIRECTION ( 'NONE',  ( 0.5914120900931444380, 0.2567974902965144413, -0.7643865440136096145 ) ) ;
#18225 = ORIENTED_EDGE ( 'NONE', *, *, #9735, .T. ) ;
#18226 = B_SPLINE_CURVE_WITH_KNOTS ( 'NONE', 3,
 ( #4533, #13306, #24571, #224, #15596, #6854 ),
 .UNSPECIFIED., .F., .F.,
 ( 4, 2, 4 ),
 ( 3.729292374017667178E-16, 0.003576372551511173073, 0.007152745103021973180 ),
 .UNSPECIFIED. ) ;
#18227 = B_SPLINE_CURVE_WITH_KNOTS ( 'NONE', 3,
 ( #17879, #6832, #26392, #9122, #15296, #15575, #6693 ),
 .UNSPECIFIED., .F., .F.,
 ( 4, 3, 4 ),
 ( 5.185633697872110560E-16, 0.02816610861753246139, 0.04000277880656268048 ),
 .UNSPECIFIED. ) ;
#18228 = B_SPLINE_CURVE_WITH_KNOTS ( 'NONE', 3,
 ( #16567, #11826, #9967, #16280, #18588, #12251, #18726 ),
 .UNSPECIFIED., .F., .F.,
 ( 4, 3, 4 ),
 ( 1.309687503460226953E-17, 0.009512539173626405331, 0.02506242213020846293 ),
 .UNSPECIFIED. ) ;
#18229 = CARTESIAN_POINT ( 'NONE',  ( -55.24728320129491266, -0.005114031043468280843, 0.01362040845703383143 ) ) ;
#18230 = DIRECTION ( 'NONE',  ( -1.000000000000000000, -0.000000000000000000, -0.000000000000000000 ) ) ;
#18231 = VERTEX_POINT ( 'NONE', #12065 ) ;
#18232 = ORIENTED_EDGE ( 'NONE', *, *, #16418, .T. ) ;
#18233 = DIRECTION ( 'NONE',  ( 0.000000000000000000, 5.223019709708233256E-21, -1.000000000000000000 ) ) ;
#18234 = CARTESIAN_POINT ( 'NONE',  ( -55.25719721206881729, -0.01041086141212241994, -0.004044147484874939351 ) ) ;
#18236 = CARTESIAN_POINT ( 'NONE',  ( -7.733045908741323693, -35.49239760110648945, 38.67583825854190138 ) ) ;
#18235 = CARTESIAN_POINT ( 'NONE',  ( 1.831572820252009626, 16.14965423926210519, 144.2101521542831222 ) ) ;
#18237 = CARTESIAN_POINT ( 'NONE',  ( 24.01988960052073807, 44.53753990739662072, -123.2441023955610433 ) ) ;
#18238 = CARTESIAN_POINT ( 'NONE',  ( 1.833750490713709880, 144.2866297127912958, 15.43355859895708093 ) ) ;
#18239 = CARTESIAN_POINT ( 'NONE',  ( 1.833485406944057594, 108.1939177044926055, 96.69979900902202985 ) ) ;
#18240 = CARTESIAN_POINT ( 'NONE',  ( -55.24271866751342941, 0.009388511352200527849, -0.001425019990779188969 ) ) ;
#18241 = ORIENTED_EDGE ( 'NONE', *, *, #22568, .T. ) ;
#18242 = CARTESIAN_POINT ( 'NONE',  ( 10.93730112725990367, -142.1801301103781157, -51.37919228020433593 ) ) ;
#18243 = CARTESIAN_POINT ( 'NONE',  ( -20.20612092514791058, -23.26073121129628873, 18.30568145913871447 ) ) ;
#18244 = CARTESIAN_POINT ( 'NONE',  ( 109.1587776205901577, -0.006944419901758109442, -0.002343968083389333292 ) ) ;
#18245 = FACE_OUTER_BOUND ( 'NONE', #17254, .T. ) ;
#18246 = LINE ( 'NONE', #20562, #15193 ) ;
#18247 = CARTESIAN_POINT ( 'NONE',  ( 109.1592201516379674, -0.0005146241775907877628, 0.007845213074660000591 ) ) ;
#18248 = CARTESIAN_POINT ( 'NONE',  ( 13.36082413113063083, -37.97423473099187419, -148.1362653801006957 ) ) ;
#18249 = CARTESIAN_POINT ( 'NONE',  ( -20.57838717382308147, 7.715628353034087894, 28.96176188950209962 ) ) ;
#18250 = FACE_OUTER_BOUND ( 'NONE', #16198, .T. ) ;
#18251 = VERTEX_POINT ( 'NONE', #15806 ) ;
#18252 = EDGE_CURVE ( 'NONE', #15678, #23588, #26731, .T. ) ;
#18253 = ORIENTED_EDGE ( 'NONE', *, *, #13678, .T. ) ;
#18254 = B_SPLINE_CURVE_WITH_KNOTS ( 'NONE', 3,
 ( #23033, #22895, #20858, #23319 ),
 .UNSPECIFIED., .F., .F.,
 ( 4, 4 ),
 ( 0.000000000000000000, 0.008383560773332696461 ),
 .UNSPECIFIED. ) ;
#18255 = VERTEX_POINT ( 'NONE', #16084 ) ;
#18256 = DIRECTION ( 'NONE',  ( -1.000000000000000000, -0.000000000000000000, -0.000000000000000000 ) ) ;
#18257 = FACE_OUTER_BOUND ( 'NONE', #3336, .T. ) ;
#18258 =( BOUNDED_SURFACE ( )  B_SPLINE_SURFACE ( 3, 1, ( 
 ( #19226, #15459 ),
 ( #28140, #24130 ),
 ( #6420, #23721 ),
 ( #10464, #10597 ) ),
 .UNSPECIFIED., .F., .F., .F. ) 
 B_SPLINE_SURFACE_WITH_KNOTS ( ( 4, 4 ),
 ( 2, 2 ),
 ( 0.000000000000000000, 1.000000000000000000 ),
 ( 0.000000000000000000, 1.000000000000000000 ),
 .UNSPECIFIED. ) 
 GEOMETRIC_REPRESENTATION_ITEM ( )  RATIONAL_B_SPLINE_SURFACE ( (
 ( 1.000000000000000000, 1.000000000000000000),
 ( 0.6386103224230302855, 0.9954351624131538845),
 ( 0.6386103224230302855, 0.9954351624131538845),
 ( 1.000000000000000000, 1.000000000000000000) ) ) 
 REPRESENTATION_ITEM ( '' )  SURFACE ( )  );
#18259 = CARTESIAN_POINT ( 'NONE',  ( -12.82751273423880001, 21.21958768041857724, 44.03362901246980243 ) ) ;
#18260 = CARTESIAN_POINT ( 'NONE',  ( 1.833721034905679392, 125.4904194343094446, -72.86293192427356757 ) ) ;
#18261 = CARTESIAN_POINT ( 'NONE',  ( 21.16825799904898986, 115.0183107335399768, -71.50503315297764573 ) ) ;
#18262 = CARTESIAN_POINT ( 'NONE',  ( -1.583189561560255143, 43.29471907393764951, 16.68617981233656877 ) ) ;
#18263 = CARTESIAN_POINT ( 'NONE',  ( 109.1587776205901577, 0.005390665547499365502, 0.004965871434389470748 ) ) ;
#18264 = ORIENTED_EDGE ( 'NONE', *, *, #7093, .F. ) ;
#18265 = ORIENTED_EDGE ( 'NONE', *, *, #22023, .F. ) ;
#18266 = CARTESIAN_POINT ( 'NONE',  ( -1.050229599974480843, -43.47850826583062656, -14.39582765040444912 ) ) ;
#18267 = B_SPLINE_CURVE_WITH_KNOTS ( 'NONE', 3,
 ( #842, #8061, #27463, #1408, #9926, #3438, #16385, #16531, #25321, #16832, #12489, #23314, #14208 ),
 .UNSPECIFIED., .F., .F.,
 ( 4, 3, 3, 3, 4 ),
 ( 8.673617379884035472E-18, 0.0007657099931970526470, 0.001531419946797914385, 0.002296279302920149496, 0.003061450627205760701 ),
 .UNSPECIFIED. ) ;
#18268 = CARTESIAN_POINT ( 'NONE',  ( 10.93730112726006176, 146.7718404940648611, -36.23586118136403655 ) ) ;
#18269 = CARTESIAN_POINT ( 'NONE',  ( -20.20612091757417161, 27.77903622052274102, 10.22177757278288013 ) ) ;
#18270 = CARTESIAN_POINT ( 'NONE',  ( 109.1587776205901861, -0.007328861771499511728, 8.330235398543782790E-05 ) ) ;
#18271 = CARTESIAN_POINT ( 'NONE',  ( 1.833838848569429247, -137.9525894882060584, 45.01064392477885434 ) ) ;
#18272 = ORIENTED_EDGE ( 'NONE', *, *, #26924, .T. ) ;
#18273 = CARTESIAN_POINT ( 'NONE',  ( 25.64681081121880624, 35.28660243342550729, 107.2555980796242494 ) ) ;
#18274 = CARTESIAN_POINT ( 'NONE',  ( 1.833206308920082739, 15.90849808442071023, -144.2348261777514153 ) ) ;
#18275 = CARTESIAN_POINT ( 'NONE',  ( -7.733045908741311258, -38.67583825854175217, -35.49239760110661024 ) ) ;
#18276 = DIRECTION ( 'NONE',  ( 1.000000000000000000, -6.938893903907226837E-18, 1.734723475976806709E-18 ) ) ;
#18277 = CARTESIAN_POINT ( 'NONE',  ( 25.87036335909427365, -107.8283083010001491, -33.99475147239120787 ) ) ;
#18278 = EDGE_CURVE ( 'NONE', #10583, #3526, #26879, .T. ) ;
#18279 = EDGE_CURVE ( 'NONE', #27772, #14162, #5470, .T. ) ;
#18280 = ORIENTED_EDGE ( 'NONE', *, *, #21932, .F. ) ;
#18281 = CARTESIAN_POINT ( 'NONE',  ( 1.833691583653554336, 145.1092556475514073, 0.3559373310799965884 ) ) ;
#18282 = ORIENTED_EDGE ( 'NONE', *, *, #24195, .F. ) ;
#18283 = EDGE_CURVE ( 'NONE', #15966, #19470, #11323, .T. ) ;
#18284 = ORIENTED_EDGE ( 'NONE', *, *, #25084, .F. ) ;
#18285 = ORIENTED_EDGE ( 'NONE', *, *, #7766, .T. ) ;
#18286 = CARTESIAN_POINT ( 'NONE',  ( 109.1592201516379674, -0.0005146241775983334847, -0.007845213074654432128 ) ) ;
#18287 = CARTESIAN_POINT ( 'NONE',  ( -1.045287976400386842, 37.92705037016744285, -25.66401692420027203 ) ) ;
#18288 = CARTESIAN_POINT ( 'NONE',  ( -1.048171036023507474, 43.23005599774320729, 15.11933492062782847 ) ) ;
#18289 = CARTESIAN_POINT ( 'NONE',  ( -18.41936578851705519, -42.05131332928132082, -5.707900577128024011 ) ) ;
#18290 = B_SPLINE_CURVE_WITH_KNOTS ( 'NONE', 3,
 ( #8588, #24140, #21685, #26007, #21402, #6169, #4262, #1955, #19521, #28426 ),
 .UNSPECIFIED., .F., .F.,
 ( 4, 3, 3, 4 ),
 ( 1.387778780781445676E-17, 0.0002669559177086201773, 0.0005339118354150702156, 0.001067817517169167285 ),
 .UNSPECIFIED. ) ;
#18291 = CARTESIAN_POINT ( 'NONE',  ( 1.834118845439484335, -107.9567937753786708, -96.96525081350110042 ) ) ;
#18292 = CARTESIAN_POINT ( 'NONE',  ( 32.73300124599735739, 32.68291970228236920, 113.0038235389603472 ) ) ;
#18293 = CARTESIAN_POINT ( 'NONE',  ( 26.11404676487257603, -36.06104232266525145, 107.3263591096429082 ) ) ;
#18294 = CARTESIAN_POINT ( 'NONE',  ( 25.64681081121879203, 112.9102952884414464, 0.4157506337731812773 ) ) ;
#18295 = CARTESIAN_POINT ( 'NONE',  ( 1.832998868059890096, 132.7810136645738055, 58.53348008137691494 ) ) ;
#18296 = CARTESIAN_POINT ( 'NONE',  ( 2.430230287190589422, 137.9371479820468949, -46.34481016236680517 ) ) ;
#18297 =( BOUNDED_SURFACE ( )  B_SPLINE_SURFACE ( 3, 1, ( 
 ( #21955, #21392 ),
 ( #19511, #8576 ),
 ( #1664, #14905 ),
 ( #15172, #23993 ) ),
 .UNSPECIFIED., .F., .F., .F. ) 
 B_SPLINE_SURFACE_WITH_KNOTS ( ( 4, 4 ),
 ( 2, 2 ),
 ( 0.000000000000000000, 1.000000000000000000 ),
 ( 0.000000000000000000, 1.000000000000000000 ),
 .UNSPECIFIED. ) 
 GEOMETRIC_REPRESENTATION_ITEM ( )  RATIONAL_B_SPLINE_SURFACE ( (
 ( 1.000000000000000000, 1.000000000000000000),
 ( 0.9956975270656954757, 0.8568959468854893125),
 ( 0.9956975270656954757, 0.8568959468854893125),
 ( 1.000000000000000000, 1.000000000000000000) ) ) 
 REPRESENTATION_ITEM ( '' )  SURFACE ( )  );
#18298 = LINE ( 'NONE', #5505, #17922 ) ;
#18299 = CARTESIAN_POINT ( 'NONE',  ( -28.13707043255157103, 0.7675454997506996335, -22.88591869784691113 ) ) ;
#18300 = CARTESIAN_POINT ( 'NONE',  ( 2.433796855181205476, -116.8607839509050734, -86.69855925934092511 ) ) ;
#18301 = CIRCLE ( 'NONE', #858, 117.6351876552689504 ) ;
#18302 = CARTESIAN_POINT ( 'NONE',  ( -24.53239521893650021, -3.868435622621272163, 33.71193723315178659 ) ) ;
#18303 = ADVANCED_FACE ( 'NONE', ( #548 ), #3789, .F. ) ;
#18304 = CARTESIAN_POINT ( 'NONE',  ( 109.1721716018069515, 0.01665253177025271744, 0.003746085893651872681 ) ) ;
#18305 = CARTESIAN_POINT ( 'NONE',  ( -1.155001620486251879, -2.068551059060010022, 45.85729774065939779 ) ) ;
#18306 = CARTESIAN_POINT ( 'NONE',  ( -1.048994561756784405, -37.49601524795390617, 26.29622118251720764 ) ) ;
#18307 = CARTESIAN_POINT ( 'NONE',  ( 109.1721716018069515, 0.01127028715939371907, 0.01281875973823906091 ) ) ;
#18308 = CARTESIAN_POINT ( 'NONE',  ( 109.1592201516379674, 0.001331853079201392653, -0.007748443302134886378 ) ) ;
#18309 = CARTESIAN_POINT ( 'NONE',  ( 109.1592201516379674, -0.002134489919774417484, -0.007566779963318545632 ) ) ;
#18310 = EDGE_CURVE ( 'NONE', #24736, #14545, #10474, .T. ) ;
#18311 = ORIENTED_EDGE ( 'NONE', *, *, #23420, .T. ) ;
#18312 = EDGE_CURVE ( 'NONE', #8086, #10267, #23169, .T. ) ;
#18313 = ORIENTED_EDGE ( 'NONE', *, *, #15886, .T. ) ;
#18314 = CARTESIAN_POINT ( 'NONE',  ( -8.786685647604885574, 6.096987947571466530E-17, -1.524246986892866633E-17 ) ) ;
#18315 = CARTESIAN_POINT ( 'NONE',  ( 24.22246935314087324, 1.405874241570340095E-14, 111.9614997405030152 ) ) ;
#18316 = VERTEX_POINT ( 'NONE', #16818 ) ;
#18317 = B_SPLINE_CURVE_WITH_KNOTS ( 'NONE', 3,
 ( #22662, #2929, #11707, #18300 ),
 .UNSPECIFIED., .F., .F.,
 ( 4, 4 ),
 ( 0.000000000000000000, 0.01077107196513875549 ),
 .UNSPECIFIED. ) ;
#18318 = ORIENTED_EDGE ( 'NONE', *, *, #15785, .F. ) ;
#18319 = ORIENTED_EDGE ( 'NONE', *, *, #19898, .T. ) ;
#18320 = B_SPLINE_CURVE_WITH_KNOTS ( 'NONE', 3,
 ( #27744, #3697, #14634, #7906, #27878, #23434 ),
 .UNSPECIFIED., .F., .F.,
 ( 4, 2, 4 ),
 ( 0.000000000000000000, 0.0004335184443140219679, 0.0008670368886280439358 ),
 .UNSPECIFIED. ) ;
#18321 = ORIENTED_EDGE ( 'NONE', *, *, #15387, .F. ) ;
#18322 = CARTESIAN_POINT ( 'NONE',  ( 9.884929003653626367, 91.84919534721940693, 119.2676479132376954 ) ) ;
#18323 = DIRECTION ( 'NONE',  ( 0.000000000000000000, 5.223019709707975211E-21, -1.000000000000000000 ) ) ;
#18324 = CARTESIAN_POINT ( 'NONE',  ( 1.833750490713699444, 144.3424379351782534, -14.90257883162603925 ) ) ;
#18325 = CARTESIAN_POINT ( 'NONE',  ( -55.25719721206881729, -0.0006290797159227240433, -0.01115102788683359700 ) ) ;
#18326 = CARTESIAN_POINT ( 'NONE',  ( -8.786685647604887350, -25.35688121747534751, -47.14957014837345639 ) ) ;
#18327 = CARTESIAN_POINT ( 'NONE',  ( 1.833485406944043827, -72.09189602597619739, -125.9346397303442728 ) ) ;
#18328 = CARTESIAN_POINT ( 'NONE',  ( -1.019300379054419947, 16.06793277091992067, -42.90269154183433642 ) ) ;
#18329 = CARTESIAN_POINT ( 'NONE',  ( 2.433796855181205476, -86.69855925934052721, 116.8607839509053434 ) ) ;
#18331 = CARTESIAN_POINT ( 'NONE',  ( 1.833206308920039662, 58.34024961171237322, 132.8652726225755032 ) ) ;
#18330 = CARTESIAN_POINT ( 'NONE',  ( -55.25719721206881729, -0.002847566758683717138, -0.01079965405819494247 ) ) ;
#18332 = CARTESIAN_POINT ( 'NONE',  ( 109.1586059443104944, 0.004378796245590010905, 0.005555961672773786220 ) ) ;
#18333 = EDGE_CURVE ( 'NONE', #14920, #25928, #3555, .T. ) ;
#18334 = VERTEX_POINT ( 'NONE', #8051 ) ;
#18335 = EDGE_LOOP ( 'NONE', ( #24583, #27979, #12392, #26898 ) ) ;
#18336 = CARTESIAN_POINT ( 'NONE',  ( 55.79472521941428198, -35.74479459808892301, 63.36760613016212318 ) ) ;
#18337 = EDGE_CURVE ( 'NONE', #16763, #10758, #17078, .T. ) ;
#18339 = CARTESIAN_POINT ( 'NONE',  ( 109.1592201516379674, -0.003661068210037343815, -0.006957642258146904887 ) ) ;
#18338 = CARTESIAN_POINT ( 'NONE',  ( -8.786685647604890903, -52.67761315067279781, 9.545808661481174795 ) ) ;
#18340 = CARTESIAN_POINT ( 'NONE',  ( -8.786685647604890903, -9.545808661480982948, -52.67761315067281913 ) ) ;
#18341 = CARTESIAN_POINT ( 'NONE',  ( 24.01988960052067767, 31.41104197353493532, -127.2243989116370386 ) ) ;
#18342 = PRESENTATION_STYLE_ASSIGNMENT (( #9880 ) ) ;
#18343 = CARTESIAN_POINT ( 'NONE',  ( -1.463510566862834983, -35.90603835816524025, -29.09194585123821497 ) ) ;
#18344 = ORIENTED_EDGE ( 'NONE', *, *, #8857, .T. ) ;
#18345 = DIRECTION ( 'NONE',  ( 0.000000000000000000, 0.000000000000000000, 1.000000000000000000 ) ) ;
#18346 = EDGE_CURVE ( 'NONE', #1690, #25788, #24899, .T. ) ;
#18347 = CARTESIAN_POINT ( 'NONE',  ( 109.1587776205901577, 0.007186028091163433260, -0.001442274045003928652 ) ) ;
#18348 = CARTESIAN_POINT ( 'NONE',  ( 32.73300124599737160, -84.80615050150427692, 81.52272205837169849 ) ) ;
#18349 = ORIENTED_EDGE ( 'NONE', *, *, #24418, .T. ) ;
#18350 = CARTESIAN_POINT ( 'NONE',  ( -20.20700224038492010, 16.58740185276710832, -24.51628800869052682 ) ) ;
#18351 = VERTEX_POINT ( 'NONE', #1254 ) ;
#18352 = B_SPLINE_CURVE_WITH_KNOTS ( 'NONE', 3,
 ( #18826, #5883, #1129, #7917, #18684, #16677, #10214, #25471, #18974, #23595 ),
 .UNSPECIFIED., .F., .F.,
 ( 4, 2, 2, 2, 4 ),
 ( 2.863532086325413454E-16, 0.0003346187017559052986, 0.0006692374035115242594, 0.001003856105267143329, 0.001338474807022762289 ),
 .UNSPECIFIED. ) ;
#18353 = DIRECTION ( 'NONE',  ( 0.000000000000000000, 1.000000000000000000, 3.122502256758243698E-15 ) ) ;
#18354 = EDGE_CURVE ( 'NONE', #23186, #10231, #18884, .T. ) ;
#18355 = CARTESIAN_POINT ( 'NONE',  ( -55.25719721206881729, -0.01115102788682980142, -0.0006290797159206544097 ) ) ;
#18356 = CARTESIAN_POINT ( 'NONE',  ( 2.433796855181219243, -132.3327394885235435, 60.50726454507858421 ) ) ;
#18357 = ORIENTED_EDGE ( 'NONE', *, *, #12080, .T. ) ;
#18358 = CARTESIAN_POINT ( 'NONE',  ( -9.156249394959706578, -38.17928057391962682, 38.89149400288449243 ) ) ;
#18359 = ORIENTED_EDGE ( 'NONE', *, *, #1846, .T. ) ;
#18360 = CARTESIAN_POINT ( 'NONE',  ( 10.93730112726005821, 140.0398180619120865, -56.95489579269602842 ) ) ;
#18361 = ORIENTED_EDGE ( 'NONE', *, *, #4387, .F. ) ;
#18362 = DIRECTION ( 'NONE',  ( 1.000000000000000000, 0.000000000000000000, 0.000000000000000000 ) ) ;
#18363 = CARTESIAN_POINT ( 'NONE',  ( -20.20997486282891131, 0.3303743256174362375, -29.60348406988234871 ) ) ;
#18364 = CARTESIAN_POINT ( 'NONE',  ( -1.323439229708128551, -38.58845475799787295, -25.17120723334079457 ) ) ;
#18365 = LINE ( 'NONE', #7312, #22655 ) ;
#18366 = B_SPLINE_CURVE_WITH_KNOTS ( 'NONE', 3,
 ( #11333, #2695, #20106, #13917, #26869, #7178, #24744, #389, #9470, #11771 ),
 .UNSPECIFIED., .F., .F.,
 ( 4, 2, 2, 2, 4 ),
 ( 2.879654849182128713E-16, 0.0003346187017559071959, 0.0006692374035115264278, 0.001003856105267145714, 0.001338474807022764891 ),
 .UNSPECIFIED. ) ;
#18367 = CARTESIAN_POINT ( 'NONE',  ( 25.64681081121879203, 112.3352186517032294, -11.38886654529559017 ) ) ;
#18368 = CARTESIAN_POINT ( 'NONE',  ( -55.24390624410018802, 0.004896917417131886954, -0.009209468562452662738 ) ) ;
#18369 = B_SPLINE_CURVE_WITH_KNOTS ( 'NONE', 3,
 ( #2152, #157, #15680, #2444, #24493, #2590, #24345, #4464 ),
 .UNSPECIFIED., .F., .F.,
 ( 4, 2, 2, 4 ),
 ( 0.000000000000000000, 0.0002429592666046768957, 0.0004859185332093537914, 0.0009718370664186768999 ),
 .UNSPECIFIED. ) ;
#18370 = VERTEX_POINT ( 'NONE', #16943 ) ;
#18371 = CARTESIAN_POINT ( 'NONE',  ( 28.37644542392835945, -54.25112470585808211, 111.8804331835014239 ) ) ;
#18372 = CARTESIAN_POINT ( 'NONE',  ( -20.57838717382308147, -28.96176188950213870, 7.715628353033985753 ) ) ;
#18373 = CARTESIAN_POINT ( 'NONE',  ( 32.73300124599739291, -3.836798148478013371, -117.5726003567929610 ) ) ;
#18374 = ORIENTED_EDGE ( 'NONE', *, *, #7772, .F. ) ;
#18375 = VERTEX_POINT ( 'NONE', #10054 ) ;
#18376 = ORIENTED_EDGE ( 'NONE', *, *, #4387, .T. ) ;
#18377 = DIRECTION ( 'NONE',  ( -5.541455922705464902E-20, 5.223019709708320524E-21, -1.000000000000000000 ) ) ;
#18378 = CARTESIAN_POINT ( 'NONE',  ( -1.583189561560256253, -11.94859433442871399, 44.83405390829683057 ) ) ;
#18379 = EDGE_CURVE ( 'NONE', #16312, #4790, #5164, .T. ) ;
#18380 = CARTESIAN_POINT ( 'NONE',  ( 32.73300124599732186, 0.000000000000000000, 0.000000000000000000 ) ) ;
#18381 = B_SPLINE_CURVE_WITH_KNOTS ( 'NONE', 3,
 ( #3037, #18414, #1160, #9649 ),
 .UNSPECIFIED., .F., .F.,
 ( 4, 4 ),
 ( 5.516747950212996126E-16, 0.008383748772659998377 ),
 .UNSPECIFIED. ) ;
#18382 = CARTESIAN_POINT ( 'NONE',  ( 10.93730112726007775, 51.37919228020501805, -142.1801301103781725 ) ) ;
#18383 = CARTESIAN_POINT ( 'NONE',  ( -1.583189561560256253, -11.94859433442871399, 44.83405390829683057 ) ) ;
#18384 = CARTESIAN_POINT ( 'NONE',  ( 1.833603222531973387, 107.5392551439154545, 97.42748212378315031 ) ) ;
#18385 = CARTESIAN_POINT ( 'NONE',  ( 32.73300124599732186, 0.000000000000000000, 0.000000000000000000 ) ) ;
#18386 = ORIENTED_EDGE ( 'NONE', *, *, #9347, .F. ) ;
#18387 = CARTESIAN_POINT ( 'NONE',  ( 2.430230287190589422, -142.6294793592095687, -28.83279105684573551 ) ) ;
#18388 = CARTESIAN_POINT ( 'NONE',  ( -20.38016308990357217, -23.16952666206571365, 18.69911008768360361 ) ) ;
#18389 = CARTESIAN_POINT ( 'NONE',  ( -20.20612092514784663, 28.48192215759677737, 8.058517256680804763 ) ) ;
#18390 = CARTESIAN_POINT ( 'NONE',  ( 6.224689322667630975, 147.4941644018829834, -12.92299475786806973 ) ) ;
#18391 = ADVANCED_FACE ( 'NONE', ( #7762 ), #9672, .F. ) ;
#18392 =( BOUNDED_SURFACE ( )  B_SPLINE_SURFACE ( 3, 1, ( 
 ( #13632, #19973 ),
 ( #22139, #22432 ),
 ( #2402, #24606 ),
 ( #20399, #11199 ) ),
 .UNSPECIFIED., .F., .F., .F. ) 
 B_SPLINE_SURFACE_WITH_KNOTS ( ( 4, 4 ),
 ( 2, 2 ),
 ( 0.000000000000000000, 1.000000000000000000 ),
 ( 0.000000000000000000, 1.000000000000000000 ),
 .UNSPECIFIED. ) 
 GEOMETRIC_REPRESENTATION_ITEM ( )  RATIONAL_B_SPLINE_SURFACE ( (
 ( 1.000000000000000000, 1.000000000000000000),
 ( 0.6386103224230316178, 0.9954351624131538845),
 ( 0.6386103224230316178, 0.9954351624131538845),
 ( 1.000000000000000000, 1.000000000000000000) ) ) 
 REPRESENTATION_ITEM ( '' )  SURFACE ( )  );
#18393 = B_SPLINE_CURVE_WITH_KNOTS ( 'NONE', 3,
 ( #2834, #5271, #20385, #669, #22417, #18079 ),
 .UNSPECIFIED., .F., .F.,
 ( 4, 2, 4 ),
 ( 3.607901639910057446E-16, 0.003576372551511165700, 0.007152745103021970578 ),
 .UNSPECIFIED. ) ;
#18394 = CARTESIAN_POINT ( 'NONE',  ( 26.11404676487257603, 110.5078194225164481, -24.64483677384740545 ) ) ;
#18395 = CARTESIAN_POINT ( 'NONE',  ( -55.25297051322618813, 0.01483298743814672610, -0.001818774723749509541 ) ) ;
#18396 = CIRCLE ( 'NONE', #16560, 53.53553390275978785 ) ;
#18397 = ORIENTED_EDGE ( 'NONE', *, *, #8741, .T. ) ;
#18398 = CARTESIAN_POINT ( 'NONE',  ( 1.833838850855486591, -30.08297881069573521, -141.9572669680998160 ) ) ;
#18399 = DIRECTION ( 'NONE',  ( -0.5914120900931443270, -0.8010740644654243958, 0.09226095020377671208 ) ) ;
#18400 = ORIENTED_EDGE ( 'NONE', *, *, #16545, .F. ) ;
#18401 = B_SPLINE_CURVE_WITH_KNOTS ( 'NONE', 3,
 ( #8698, #10580, #11006, #17463 ),
 .UNSPECIFIED., .F., .F.,
 ( 4, 4 ),
 ( 2.005388357681274105E-16, 0.001982023823822939412 ),
 .UNSPECIFIED. ) ;
#18402 =( BOUNDED_SURFACE ( )  B_SPLINE_SURFACE ( 3, 1, ( 
 ( #18840, #10226 ),
 ( #3722, #14652 ),
 ( #27899, #23457 ),
 ( #12633, #27766 ) ),
 .UNSPECIFIED., .F., .F., .F. ) 
 B_SPLINE_SURFACE_WITH_KNOTS ( ( 4, 4 ),
 ( 2, 2 ),
 ( 0.000000000000000000, 1.000000000000000000 ),
 ( 0.000000000000000000, 1.000000000000000000 ),
 .UNSPECIFIED. ) 
 GEOMETRIC_REPRESENTATION_ITEM ( )  RATIONAL_B_SPLINE_SURFACE ( (
 ( 1.000000000000000000, 1.000000000000000000),
 ( 0.6386103224230316178, 0.9954351624131538845),
 ( 0.6386103224230316178, 0.9954351624131538845),
 ( 1.000000000000000000, 1.000000000000000000) ) ) 
 REPRESENTATION_ITEM ( '' )  SURFACE ( )  );
#18403 = ORIENTED_EDGE ( 'NONE', *, *, #1237, .T. ) ;
#18404 = ORIENTED_EDGE ( 'NONE', *, *, #4354, .F. ) ;
#18405 = CARTESIAN_POINT ( 'NONE',  ( 109.1624594426973118, -0.01154818537151447444, 0.01102230012606822233 ) ) ;
#18406 = CARTESIAN_POINT ( 'NONE',  ( 25.64708010899962787, -23.52908206539823155, -110.4325102642037564 ) ) ;
#18407 = CARTESIAN_POINT ( 'NONE',  ( 109.1624594426973260, 0.0004639210235575793413, -0.01595733256931100227 ) ) ;
#18408 = AXIS2_PLACEMENT_3D ( 'NONE', #22778, #14102, #869 ) ;
#18409 = CARTESIAN_POINT ( 'NONE',  ( 1.833485406944057594, 58.53321471327059555, -132.7804117027882285 ) ) ;
#18410 = CARTESIAN_POINT ( 'NONE',  ( 1.833603222531960286, 125.8904991419477142, -72.16916166673607336 ) ) ;
#18411 = ORIENTED_EDGE ( 'NONE', *, *, #21879, .T. ) ;
#18412 = AXIS2_PLACEMENT_3D ( 'NONE', #15207, #25899, #24028 ) ;
#18413 = CARTESIAN_POINT ( 'NONE',  ( 109.1592201516379674, -0.003476928926125439582, 0.007051465909551701133 ) ) ;
#18414 = CARTESIAN_POINT ( 'NONE',  ( 30.59138290137910943, 21.51300488027276003, -114.2039707400271595 ) ) ;
#18415 = ORIENTED_EDGE ( 'NONE', *, *, #11971, .F. ) ;
#18416 = MECHANICAL_DESIGN_GEOMETRIC_PRESENTATION_REPRESENTATION (  '', ( #11074 ), #13327 ) ;
#18417 = ORIENTED_EDGE ( 'NONE', *, *, #10951, .T. ) ;
#18418 = CARTESIAN_POINT ( 'NONE',  ( -55.24340739397742794, 0.007744344507854989193, -0.006539691034608598359 ) ) ;
#18419 = CARTESIAN_POINT ( 'NONE',  ( -1.046936909428682672, -36.28616897897433091, 27.93981068760662012 ) ) ;
#18420 = EDGE_CURVE ( 'NONE', #1094, #10623, #27113, .T. ) ;
#18421 = CARTESIAN_POINT ( 'NONE',  ( 26.11404676487257603, 90.92995828888292920, -67.46175819463273626 ) ) ;
#18422 = CARTESIAN_POINT ( 'NONE',  ( 55.49584447822657296, 62.69727227546400883, 36.50733923851220197 ) ) ;
#18423 = LINE ( 'NONE', #22298, #12528 ) ;
#18424 = CARTESIAN_POINT ( 'NONE',  ( 109.1586900883932856, 0.006130969560693664243, 0.003656351050324906093 ) ) ;
#18425 = CARTESIAN_POINT ( 'NONE',  ( -6.574463467970655728, 51.07975593197905795, -5.014313797967199449 ) ) ;
#18426 = B_SPLINE_CURVE_WITH_KNOTS ( 'NONE', 3,
 ( #2970, #11745, #230, #9019, #17908, #799, #6859, #7011 ),
 .UNSPECIFIED., .F., .F.,
 ( 4, 2, 2, 4 ),
 ( 2.324173423859648542E-16, 0.002761568181852869404, 0.005523136363705506355, 0.01104627272741079066 ),
 .UNSPECIFIED. ) ;
#18427 = CARTESIAN_POINT ( 'NONE',  ( -1.048994561756806165, -45.79144455904140898, -0.7655149579821828310 ) ) ;
#18428 = VERTEX_POINT ( 'NONE', #86 ) ;
#18429 = CARTESIAN_POINT ( 'NONE',  ( 1.833750490713684345, 58.77746103890281404, 132.6726660571946184 ) ) ;
#18430 = FACE_OUTER_BOUND ( 'NONE', #19108, .T. ) ;
#18431 = EDGE_CURVE ( 'NONE', #3869, #16027, #14732, .T. ) ;
#18432 = EDGE_CURVE ( 'NONE', #6423, #21210, #13713, .T. ) ;
#18433 = CARTESIAN_POINT ( 'NONE',  ( -1.056502255334264895, 0.5104472526226292439, 45.80535052436395915 ) ) ;
#18434 = CARTESIAN_POINT ( 'NONE',  ( 109.1624594426973118, -0.006066618937910808231, 0.01476644236456995697 ) ) ;
#18435 = CARTESIAN_POINT ( 'NONE',  ( -55.24271866751342941, -0.006671293903667678896, -0.006757859501010191408 ) ) ;
#18436 = ORIENTED_EDGE ( 'NONE', *, *, #2687, .T. ) ;
#18437 = ORIENTED_EDGE ( 'NONE', *, *, #9767, .T. ) ;
#18438 = CARTESIAN_POINT ( 'NONE',  ( 25.64681081121879203, 23.06870491922322230, 110.5293738517609228 ) ) ;
#18439 = VECTOR ( 'NONE', #21375, 1000.000000000000114 ) ;
#18440 = ORIENTED_EDGE ( 'NONE', *, *, #12847, .F. ) ;
#18441 = CIRCLE ( 'NONE', #8349, 34.60786435723138510 ) ;
#18442 = B_SPLINE_CURVE_WITH_KNOTS ( 'NONE', 3,
 ( #8080, #16704, #5768, #19269, #25629, #23333, #8202, #5911 ),
 .UNSPECIFIED., .F., .F.,
 ( 4, 2, 2, 4 ),
 ( 2.299172327962918193E-16, 0.002761568181852868970, 0.005523136363705508090, 0.01104627272741078720 ),
 .UNSPECIFIED. ) ;
#18443 = B_SPLINE_CURVE_WITH_KNOTS ( 'NONE', 3,
 ( #5296, #9773, #10057, #20972, #20551, #27592, #833, #23020, #9917, #10211 ),
 .UNSPECIFIED., .F., .F.,
 ( 4, 3, 3, 4 ),
 ( 1.214306433183764966E-17, 0.0002669560319015731767, 0.0005492286108966349485, 0.0008315040496093412115 ),
 .UNSPECIFIED. ) ;
#18444 = EDGE_LOOP ( 'NONE', ( #4818, #5828, #4865, #7618 ) ) ;
#18445 = ORIENTED_EDGE ( 'NONE', *, *, #23096, .F. ) ;
#18447 = AXIS2_PLACEMENT_3D ( 'NONE', #9183, #9770, #18377 ) ;
#18446 =( BOUNDED_SURFACE ( )  B_SPLINE_SURFACE ( 3, 1, ( 
 ( #27491, #7803 ),
 ( #14237, #21156 ),
 ( #10248, #25507 ),
 ( #14539, #9958 ) ),
 .UNSPECIFIED., .F., .F., .F. ) 
 B_SPLINE_SURFACE_WITH_KNOTS ( ( 4, 4 ),
 ( 2, 2 ),
 ( 0.000000000000000000, 1.000000000000000000 ),
 ( 0.000000000000000000, 1.000000000000000000 ),
 .UNSPECIFIED. ) 
 GEOMETRIC_REPRESENTATION_ITEM ( )  RATIONAL_B_SPLINE_SURFACE ( (
 ( 1.000000000000000000, 1.000000000000000000),
 ( 0.9934239774497838349, 0.8357310067453913582),
 ( 0.9934239774497838349, 0.8357310067453913582),
 ( 1.000000000000000000, 1.000000000000000000) ) ) 
 REPRESENTATION_ITEM ( '' )  SURFACE ( )  );
#18448 = EDGE_CURVE ( 'NONE', #5027, #16169, #9979, .T. ) ;
#18449 = DIRECTION ( 'NONE',  ( 0.000000000000000000, 5.223019709708233256E-21, -1.000000000000000000 ) ) ;
#18450 = CARTESIAN_POINT ( 'NONE',  ( -15.02187109954776290, -45.93032478317472567, -6.234056423739352759 ) ) ;
#18451 = CARTESIAN_POINT ( 'NONE',  ( 1.833206310202340816, -126.0392056382537191, -71.90885922990283063 ) ) ;
#18452 = EDGE_CURVE ( 'NONE', #14622, #18231, #28287, .T. ) ;
#18453 = DIRECTION ( 'NONE',  ( -0.7563875759206388771, 0.4122509917856786443, 0.5078650950445640078 ) ) ;
#18454 = VERTEX_POINT ( 'NONE', #4690 ) ;
#18455 = CIRCLE ( 'NONE', #5584, 117.6351876552689504 ) ;
#18456 = LINE ( 'NONE', #7385, #12955 ) ;
#18457 = AXIS2_PLACEMENT_3D ( 'NONE', #13537, #22035, #2899 ) ;
#18458 = CARTESIAN_POINT ( 'NONE',  ( 1.893872463202046275, 108.5026245911431744, -96.41404152942830308 ) ) ;
#18459 = ADVANCED_FACE ( 'NONE', ( #6857 ), #28077, .T. ) ;
#18460 = B_SPLINE_CURVE_WITH_KNOTS ( 'NONE', 3,
 ( #7232, #27059, #22487, #2750, #16135, #22341, #24934, #5196, #4773, #3050 ),
 .UNSPECIFIED., .F., .F.,
 ( 4, 2, 2, 2, 4 ),
 ( 2.863532086325413454E-16, 0.0003346187017559064912, 0.0006692374035115266446, 0.001003856105267146798, 0.001338474807022767060 ),
 .UNSPECIFIED. ) ;
#18461 = EDGE_CURVE ( 'NONE', #26821, #19892, #17836, .T. ) ;
#18462 = CARTESIAN_POINT ( 'NONE',  ( -1.045287976400365970, 45.76855895860943235, -1.530335034934267258 ) ) ;
#18463 = CARTESIAN_POINT ( 'NONE',  ( 32.73300124599738581, -28.19767303745521758, -114.2056417606550696 ) ) ;
#18464 = CARTESIAN_POINT ( 'NONE',  ( -24.53239521893651442, -14.09666242510773948, 30.86654523348680002 ) ) ;
#18465 = CARTESIAN_POINT ( 'NONE',  ( -25.21435515916025594, 1.749597353048488237E-16, -4.373993382621220594E-17 ) ) ;
#18466 = CIRCLE ( 'NONE', #23538, 53.53553390275978785 ) ;
#18467 = CARTESIAN_POINT ( 'NONE',  ( 109.1778270068192853, 0.007152128381195953059, 0.005967275455179350992 ) ) ;
#18468 = CARTESIAN_POINT ( 'NONE',  ( -55.24728320129491266, 0.01362040845703433277, 0.005114031043468512429 ) ) ;
#18469 = CARTESIAN_POINT ( 'NONE',  ( 2.433796855181205476, -84.34988187690851191, -118.5671979538065273 ) ) ;
#18470 = CARTESIAN_POINT ( 'NONE',  ( 13.36082413113063083, -97.52406103376836199, 117.7941133658635238 ) ) ;
#18471 = CARTESIAN_POINT ( 'NONE',  ( -2.265401668238153032, -11.98901689611074062, -45.46007138824035820 ) ) ;
#18472 = ORIENTED_EDGE ( 'NONE', *, *, #1529, .T. ) ;
#18473 = CARTESIAN_POINT ( 'NONE',  ( 30.58324630866342630, 28.99049605145726360, 117.4177132550297387 ) ) ;
#18474 = ORIENTED_EDGE ( 'NONE', *, *, #13404, .F. ) ;
#18475 = CARTESIAN_POINT ( 'NONE',  ( -1.049817751779881680, 43.71287583013727129, -13.66628317065001674 ) ) ;
#18476 = FACE_OUTER_BOUND ( 'NONE', #7096, .T. ) ;
#18477 = ORIENTED_EDGE ( 'NONE', *, *, #15865, .F. ) ;
#18478 = ORIENTED_EDGE ( 'NONE', *, *, #13806, .T. ) ;
#18479 = VERTEX_POINT ( 'NONE', #4120 ) ;
#18480 = AXIS2_PLACEMENT_3D ( 'NONE', #17340, #9142, #11730 ) ;
#18481 = CARTESIAN_POINT ( 'NONE',  ( -55.24300891470650754, -0.007734635432136225362, 0.006048736206179294861 ) ) ;
#18482 = CARTESIAN_POINT ( 'NONE',  ( 109.1586900883932856, 0.005371970278523965393, -0.004701023939953875505 ) ) ;
#18483 = CONICAL_SURFACE ( 'NONE', #9766, 117.6351876552689504, 0.9945805576725580410 ) ;
#18484 = CARTESIAN_POINT ( 'NONE',  ( 32.73300124599732186, 0.000000000000000000, 0.000000000000000000 ) ) ;
#18485 =( BOUNDED_SURFACE ( )  B_SPLINE_SURFACE ( 3, 1, ( 
 ( #611, #13842 ),
 ( #16145, #2920 ),
 ( #11399, #890 ),
 ( #4926, #22649 ) ),
 .UNSPECIFIED., .F., .F., .F. ) 
 B_SPLINE_SURFACE_WITH_KNOTS ( ( 4, 4 ),
 ( 2, 2 ),
 ( 0.000000000000000000, 1.000000000000000000 ),
 ( 0.000000000000000000, 1.000000000000000000 ),
 .UNSPECIFIED. ) 
 GEOMETRIC_REPRESENTATION_ITEM ( )  RATIONAL_B_SPLINE_SURFACE ( (
 ( 1.000000000000000000, 1.000000000000000000),
 ( 0.9934239774497838349, 0.8357310067453913582),
 ( 0.9934239774497838349, 0.8357310067453913582),
 ( 1.000000000000000000, 1.000000000000000000) ) ) 
 REPRESENTATION_ITEM ( '' )  SURFACE ( )  );
#18486 = EDGE_CURVE ( 'NONE', #19810, #10856, #24391, .T. ) ;
#18487 = CARTESIAN_POINT ( 'NONE',  ( 1.833721034905633651, 30.51809396651017181, 141.8643653601971550 ) ) ;
#18488 = EDGE_CURVE ( 'NONE', #24385, #23267, #3443, .T. ) ;
#18489 = CARTESIAN_POINT ( 'NONE',  ( 1.833206310202321498, 71.90885922990329959, -126.0392056382534633 ) ) ;
#18490 = CARTESIAN_POINT ( 'NONE',  ( 109.1586059443104944, -0.006344953511159748608, 0.003127959656220974296 ) ) ;
#18491 = CARTESIAN_POINT ( 'NONE',  ( -1.464342487929852998, 25.15873223207692178, -38.76467504336592640 ) ) ;
#18492 = DIRECTION ( 'NONE',  ( -1.000000000000000000, -0.000000000000000000, -0.000000000000000000 ) ) ;
#18493 = CARTESIAN_POINT ( 'NONE',  ( -1.259972190295313599, -44.39825172539703146, -12.06706380853675142 ) ) ;
#18494 = DIRECTION ( 'NONE',  ( -1.000000000000000000, -0.000000000000000000, -0.000000000000000000 ) ) ;
#18495 = ORIENTED_EDGE ( 'NONE', *, *, #8553, .F. ) ;
#18496 = ORIENTED_EDGE ( 'NONE', *, *, #18283, .T. ) ;
#18497 = CARTESIAN_POINT ( 'NONE',  ( -1.019300379054419947, -2.023851374322355845, 45.76814864815092676 ) ) ;
#18499 = CARTESIAN_POINT ( 'NONE',  ( 25.64704443564076186, -91.42548471394241005, 66.25951665433258597 ) ) ;
#18498 = CARTESIAN_POINT ( 'NONE',  ( 1.833838848569443014, 85.43736077718862987, 117.2916552720321448 ) ) ;
#18500 = CARTESIAN_POINT ( 'NONE',  ( 30.59138290137906324, -38.47117663195886195, -109.6600423140545786 ) ) ;
#18501 = CARTESIAN_POINT ( 'NONE',  ( -8.259864102781680373, 47.98931516265592734, -22.52209142944943565 ) ) ;
#18502 = VERTEX_POINT ( 'NONE', #24139 ) ;
#18503 = CIRCLE ( 'NONE', #14374, 34.60786435723138510 ) ;
#18504 = EDGE_LOOP ( 'NONE', ( #16203, #22046, #18509, #6088 ) ) ;
#18505 = CARTESIAN_POINT ( 'NONE',  ( 2.430230287190581429, 126.7388733285354760, -71.49654683843377256 ) ) ;
#18506 = AXIS2_PLACEMENT_3D ( 'NONE', #23531, #16896, #1206 ) ;
#18507 = CARTESIAN_POINT ( 'NONE',  ( 2.430230287190581429, 144.5585181921885862, 16.65331920325786896 ) ) ;
#18508 = DIRECTION ( 'NONE',  ( 0.5946245182733607137, 0.5955128528260739129, 0.5401723099040939280 ) ) ;
#18509 = ORIENTED_EDGE ( 'NONE', *, *, #26281, .T. ) ;
#18510 = CARTESIAN_POINT ( 'NONE',  ( 10.93730112725994275, -26.59437931460641025, -148.8212007290665042 ) ) ;
#18511 = CARTESIAN_POINT ( 'NONE',  ( 1.833485406944043827, -144.3694338680886062, 14.63699153649312201 ) ) ;
#18512 = CARTESIAN_POINT ( 'NONE',  ( 55.49584447822657296, -53.73688382046297818, 48.74506217377864203 ) ) ;
#18513 = B_SPLINE_CURVE_WITH_KNOTS ( 'NONE', 3,
 ( #1718, #21583, #12660, #21444, #3892, #27921, #6210, #17259, #1999, #26048 ),
 .UNSPECIFIED., .F., .F.,
 ( 4, 2, 2, 2, 4 ),
 ( 4.210279659405072890E-18, 0.0003346267210630959280, 0.0006692534421261876277, 0.001003880163189279110, 0.001338506884252370919 ),
 .UNSPECIFIED. ) ;
#18514 = B_SPLINE_CURVE_WITH_KNOTS ( 'NONE', 3,
 ( #18643, #21072, #18932, #10832, #16783, #1357 ),
 .UNSPECIFIED., .F., .F.,
 ( 4, 2, 4 ),
 ( 6.071532165918824830E-18, 0.0006311636237756803203, 0.001262327247551354569 ),
 .UNSPECIFIED. ) ;
#18515 = EDGE_LOOP ( 'NONE', ( #8178, #19277, #2430, #6730 ) ) ;
#18516 = CARTESIAN_POINT ( 'NONE',  ( -1.583189561560256253, 36.01941156322789794, -29.24830400313178203 ) ) ;
#18517 = AXIS2_PLACEMENT_3D ( 'NONE', #8397, #6106, #19049 ) ;
#18518 = EDGE_CURVE ( 'NONE', #26365, #21439, #8236, .T. ) ;
#18519 = ORIENTED_EDGE ( 'NONE', *, *, #17979, .T. ) ;
#18520 = CARTESIAN_POINT ( 'NONE',  ( -1.323830074806768398, -43.04593525292981582, -16.42382241777520946 ) ) ;
#18521 = CARTESIAN_POINT ( 'NONE',  ( -23.79248802219731473, -16.82188324679459868, 28.61009539422402881 ) ) ;
#18522 = ADVANCED_FACE ( 'NONE', ( #15182 ), #14284, .T. ) ;
#18523 = ORIENTED_EDGE ( 'NONE', *, *, #20403, .F. ) ;
#18524 = CARTESIAN_POINT ( 'NONE',  ( -1.239374126674604337, 38.61989855450975995, 25.08410696974200604 ) ) ;
#18525 =( BOUNDED_SURFACE ( )  B_SPLINE_SURFACE ( 3, 1, ( 
 ( #23831, #12719 ),
 ( #10575, #14885 ),
 ( #3811, #10318 ),
 ( #21368, #6394 ) ),
 .UNSPECIFIED., .F., .F., .F. ) 
 B_SPLINE_SURFACE_WITH_KNOTS ( ( 4, 4 ),
 ( 2, 2 ),
 ( 0.000000000000000000, 1.000000000000000000 ),
 ( 0.000000000000000000, 1.000000000000000000 ),
 .UNSPECIFIED. ) 
 GEOMETRIC_REPRESENTATION_ITEM ( )  RATIONAL_B_SPLINE_SURFACE ( (
 ( 1.000000000000000000, 1.000000000000000000),
 ( 0.9593753223639863714, 0.9995975284513187731),
 ( 0.9593753223639863714, 0.9995975284513187731),
 ( 1.000000000000000000, 1.000000000000000000) ) ) 
 REPRESENTATION_ITEM ( '' )  SURFACE ( )  );
#18526 = ADVANCED_FACE ( 'NONE', ( #19376 ), #15525, .F. ) ;
#18527 = FACE_OUTER_BOUND ( 'NONE', #22490, .T. ) ;
#18528 = FACE_OUTER_BOUND ( 'NONE', #19322, .T. ) ;
#18529 = FACE_OUTER_BOUND ( 'NONE', #28248, .T. ) ;
#18530 = ORIENTED_EDGE ( 'NONE', *, *, #653, .F. ) ;
#18531 = B_SPLINE_CURVE_WITH_KNOTS ( 'NONE', 3,
 ( #23338, #27629, #27783, #25634, #19273, #9952, #10505, #5773, #14530, #28045 ),
 .UNSPECIFIED., .F., .F.,
 ( 4, 3, 3, 4 ),
 ( 1.387778780781445676E-17, 0.0002669559177086277667, 0.0005339118354151018743, 0.001067817517169159262 ),
 .UNSPECIFIED. ) ;
#18532 = EDGE_CURVE ( 'NONE', #21438, #22199, #20079, .T. ) ;
#18533 = CARTESIAN_POINT ( 'NONE',  ( -55.25719721206881729, 0.008651607285660455754, 0.007063345920777159767 ) ) ;
#18535 = CARTESIAN_POINT ( 'NONE',  ( -1.058473599757823846, -45.77379534793241334, 1.755404039369906188 ) ) ;
#18534 = DIRECTION ( 'NONE',  ( 0.000000000000000000, -1.000000000000000000, 0.000000000000000000 ) ) ;
#18536 = CARTESIAN_POINT ( 'NONE',  ( -22.34422965417124018, -26.20925041532873223, -27.39717383755272451 ) ) ;
#18537 = ORIENTED_EDGE ( 'NONE', *, *, #4777, .F. ) ;
#18538 = ORIENTED_EDGE ( 'NONE', *, *, #1536, .T. ) ;
#18539 = VERTEX_POINT ( 'NONE', #9577 ) ;
#18540 = CARTESIAN_POINT ( 'NONE',  ( -8.786685647604885574, 6.096987947571466530E-17, -1.524246986892866633E-17 ) ) ;
#18541 = CARTESIAN_POINT ( 'NONE',  ( -21.41430102051751660, -28.68859753627386766, 11.22990201072307137 ) ) ;
#18543 = CARTESIAN_POINT ( 'NONE',  ( -20.20700224038492010, -0.9908225410480588913, -29.58392382092672435 ) ) ;
#18542 = DIRECTION ( 'NONE',  ( -1.000000000000000000, -0.000000000000000000, -0.000000000000000000 ) ) ;
#18544 = CARTESIAN_POINT ( 'NONE',  ( -20.47566338032515887, -7.708089572830225222, 28.85746366088577375 ) ) ;
#18545 = CARTESIAN_POINT ( 'NONE',  ( 30.58324630866342986, -8.712468656081444607, 120.6294372749320161 ) ) ;
#18546 = CARTESIAN_POINT ( 'NONE',  ( -1.031422197589716205, -25.67058493451469658, -37.93675465142464276 ) ) ;
#18547 = CARTESIAN_POINT ( 'NONE',  ( 32.73300124599735739, -39.98094346392385745, 110.6325518752272501 ) ) ;
#18548 = EDGE_LOOP ( 'NONE', ( #28435, #25856, #19732, #3534 ) ) ;
#18549 = CARTESIAN_POINT ( 'NONE',  ( 32.73300124599734318, 105.8473486001051072, 51.32617430724947383 ) ) ;
#18550 = CARTESIAN_POINT ( 'NONE',  ( -2.904412668506649808, -30.27712468694961956, 36.79926976721486653 ) ) ;
#18551 = CARTESIAN_POINT ( 'NONE',  ( 25.70243777736188306, -66.98101477609066023, 90.94412140945929934 ) ) ;
#18552 = PLANE ( 'NONE',  #4981 ) ;
#18553 = DIRECTION ( 'NONE',  ( -0.5946245182733607137, -0.002950380665379280162, -0.8039981203473693938 ) ) ;
#18554 = CARTESIAN_POINT ( 'NONE',  ( 1.833485406944057594, 15.69895494453384721, 144.2578170162063884 ) ) ;
#18555 = CARTESIAN_POINT ( 'NONE',  ( 32.73300124599734318, 108.9684813982489118, 44.31599526637995012 ) ) ;
#18556 = VERTEX_POINT ( 'NONE', #18062 ) ;
#18557 = DIRECTION ( 'NONE',  ( 0.7637818620346801257, -0.5092696688508668856, -0.3965875333584823470 ) ) ;
#18558 = AXIS2_PLACEMENT_3D ( 'NONE', #18565, #1281, #22762 ) ;
#18559 = VECTOR ( 'NONE', #19751, 1000.000000000000000 ) ;
#18560 = CARTESIAN_POINT ( 'NONE',  ( -20.57838717382308147, 16.28767523336121315, -25.16001208503110931 ) ) ;
#18561 = CARTESIAN_POINT ( 'NONE',  ( 26.28373643307435614, 55.65614982951275636, 114.7784771129672379 ) ) ;
#18562 = ORIENTED_EDGE ( 'NONE', *, *, #3617, .T. ) ;
#18563 = EDGE_LOOP ( 'NONE', ( #4082, #19671, #4718, #18975 ) ) ;
#18564 = EDGE_CURVE ( 'NONE', #12372, #23363, #11446, .T. ) ;
#18565 = CARTESIAN_POINT ( 'NONE',  ( -8.786685647604885574, 6.096987947571466530E-17, -1.524246986892866633E-17 ) ) ;
#18566 = CARTESIAN_POINT ( 'NONE',  ( -1.050230346682684113, -43.55729751025872787, -14.15335421912565828 ) ) ;
#18567 = FILL_AREA_STYLE_COLOUR ( '', #6044 ) ;
#18568 = EDGE_CURVE ( 'NONE', #2788, #4272, #15087, .T. ) ;
#18569 = CARTESIAN_POINT ( 'NONE',  ( -20.20700224038492721, 23.35150625415659320, -18.19058640100232438 ) ) ;
#18570 = CARTESIAN_POINT ( 'NONE',  ( 25.87036335909426654, 97.41424496619603701, -57.38512068812907074 ) ) ;
#18571 = VERTEX_POINT ( 'NONE', #7283 ) ;
#18572 = CARTESIAN_POINT ( 'NONE',  ( -55.24271866751342941, -0.001425019990778742711, -0.009388511352200234680 ) ) ;
#18573 = CARTESIAN_POINT ( 'NONE',  ( -1.019300379054419947, 42.90269154183450695, 16.06793277091947658 ) ) ;
#18574 = ADVANCED_FACE ( 'NONE', ( #2689 ), #20361, .T. ) ;
#18575 = CARTESIAN_POINT ( 'NONE',  ( 26.11404676487259024, -45.01677474591480888, 103.8885755249567922 ) ) ;
#18576 = ORIENTED_EDGE ( 'NONE', *, *, #23790, .F. ) ;
#18577 = VERTEX_POINT ( 'NONE', #7428 ) ;
#18578 = CARTESIAN_POINT ( 'NONE',  ( 10.93730112725972070, -26.59437931460858451, 148.8212007290659642 ) ) ;
#18579 = CARTESIAN_POINT ( 'NONE',  ( -7.078251931573400491, -26.33626633876254886, -44.92740138729156030 ) ) ;
#18580 = CARTESIAN_POINT ( 'NONE',  ( 21.16825799904907512, -18.54093663547738302, -134.1581724640165305 ) ) ;
#18581 = LINE ( 'NONE', #17393, #23945 ) ;
#18582 = CARTESIAN_POINT ( 'NONE',  ( -4.780792508754322157, 37.74278713234441796, 32.07473752860738614 ) ) ;
#18583 = CARTESIAN_POINT ( 'NONE',  ( 1.833603222531969834, -138.1443021179084099, 44.41798579679493741 ) ) ;
#18584 = B_SPLINE_CURVE_WITH_KNOTS ( 'NONE', 3,
 ( #20805, #5259, #13893, #12032, #25429, #1093 ),
 .UNSPECIFIED., .F., .F.,
 ( 4, 2, 4 ),
 ( 1.389302603484999005E-17, 0.0006311571484586140290, 0.001262314296917213963 ),
 .UNSPECIFIED. ) ;
#18585 = CARTESIAN_POINT ( 'NONE',  ( 109.1592201516379674, -0.005631912476305732905, -0.005485778713193728215 ) ) ;
#18586 = ORIENTED_EDGE ( 'NONE', *, *, #16868, .T. ) ;
#18587 = CARTESIAN_POINT ( 'NONE',  ( 1.833485406944057594, 59.50871042846225834, 132.3460930279893262 ) ) ;
#18588 = CARTESIAN_POINT ( 'NONE',  ( -18.41936578851712625, -30.66520733838672186, -29.33493038358061966 ) ) ;
#18589 = FACE_OUTER_BOUND ( 'NONE', #13519, .T. ) ;
#18590 = CARTESIAN_POINT ( 'NONE',  ( 109.1589550718174877, 0.005777059646704591107, -0.004900004919105018994 ) ) ;
#18591 =( BOUNDED_SURFACE ( )  B_SPLINE_SURFACE ( 3, 1, ( 
 ( #19959, #17651 ),
 ( #24150, #21977 ),
 ( #28436, #11041 ),
 ( #8738, #26431 ) ),
 .UNSPECIFIED., .F., .F., .F. ) 
 B_SPLINE_SURFACE_WITH_KNOTS ( ( 4, 4 ),
 ( 2, 2 ),
 ( 0.000000000000000000, 1.000000000000000000 ),
 ( 0.000000000000000000, 1.000000000000000000 ),
 .UNSPECIFIED. ) 
 GEOMETRIC_REPRESENTATION_ITEM ( )  RATIONAL_B_SPLINE_SURFACE ( (
 ( 1.000000000000000000, 1.000000000000000000),
 ( 0.7789835883360578528, 0.9689951854195403280),
 ( 0.7789835883360578528, 0.9689951854195403280),
 ( 1.000000000000000000, 1.000000000000000000) ) ) 
 REPRESENTATION_ITEM ( '' )  SURFACE ( )  );
#18592 = CARTESIAN_POINT ( 'NONE',  ( 25.98107933586718232, 65.61242423298442361, 92.16448350435750569 ) ) ;
#18593 = VERTEX_POINT ( 'NONE', #13599 ) ;
#18594 = CARTESIAN_POINT ( 'NONE',  ( 10.93730112725932635, 0.000000000000000000, 0.000000000000000000 ) ) ;
#18595 = ORIENTED_EDGE ( 'NONE', *, *, #13369, .F. ) ;
#18596 = VERTEX_POINT ( 'NONE', #20215 ) ;
#18597 = VERTEX_POINT ( 'NONE', #938 ) ;
#18598 = ADVANCED_FACE ( 'NONE', ( #361 ), #18620, .F. ) ;
#18599 = CARTESIAN_POINT ( 'NONE',  ( 25.86096068574578410, -107.8247115223744146, 33.98552076022159696 ) ) ;
#18600 = CARTESIAN_POINT ( 'NONE',  ( 32.73300124599738581, 44.31599526638102304, -108.9684813982483860 ) ) ;
#18601 = ADVANCED_FACE ( 'NONE', ( #16192 ), #10718, .F. ) ;
#18602 = PRODUCT_DEFINITION_CONTEXT ( 'detailed design', #4206, 'design' ) ;
#18603 = CARTESIAN_POINT ( 'NONE',  ( 109.1778270068192853, 0.0006237116683806083386, 0.009293669915253099933 ) ) ;
#18604 = EDGE_CURVE ( 'NONE', #457, #16924, #2815, .T. ) ;
#18605 = CARTESIAN_POINT ( 'NONE',  ( 2.263178607246673746, -126.6115608827432482, -71.48082837426134972 ) ) ;
#18606 = DIRECTION ( 'NONE',  ( 0.000000000000000000, 5.223019709707975211E-21, -1.000000000000000000 ) ) ;
#18607 = CARTESIAN_POINT ( 'NONE',  ( -55.24340739397742084, -0.007744344507854280558, -0.006539691034612628989 ) ) ;
#18608 = B_SPLINE_CURVE_WITH_KNOTS ( 'NONE', 3,
 ( #2219, #19370, #24134, #10886, #21394, #8718, #14909, #26271 ),
 .UNSPECIFIED., .F., .F.,
 ( 4, 2, 2, 4 ),
 ( 1.734723475976807094E-17, 0.0002429592666046780883, 0.0004859185332093388294, 0.0009718370664186723462 ),
 .UNSPECIFIED. ) ;
#18609 = CARTESIAN_POINT ( 'NONE',  ( 2.433796855181205476, -107.1581411821778858, -98.43889364293970345 ) ) ;
#18610 = CARTESIAN_POINT ( 'NONE',  ( 1.833721034905648972, -85.58110185770016187, -117.1867194831487495 ) ) ;
#18611 = CARTESIAN_POINT ( 'NONE',  ( 10.93730112725978287, -133.3192575531804209, 71.28103789254889477 ) ) ;
#18612 = FACE_OUTER_BOUND ( 'NONE', #25519, .T. ) ;
#18613 = CARTESIAN_POINT ( 'NONE',  ( 10.93730112725999248, 42.00474393596446987, -145.2260730187398110 ) ) ;
#18614 = CARTESIAN_POINT ( 'NONE',  ( 25.81918753295380498, -22.58534689649746596, 110.7464580477337108 ) ) ;
#18615 = LINE ( 'NONE', #5513, #1085 ) ;
#18616 = CARTESIAN_POINT ( 'NONE',  ( -1.619063947482194177, 35.99532424477422410, 29.22875152547716482 ) ) ;
#18617 = CARTESIAN_POINT ( 'NONE',  ( 25.64708010899966339, 83.87281825978713812, -75.59303792846540659 ) ) ;
#18618 = ORIENTED_EDGE ( 'NONE', *, *, #7453, .T. ) ;
#18619 = DIRECTION ( 'NONE',  ( -1.000000000000000000, -0.000000000000000000, -0.000000000000000000 ) ) ;
#18620 =( BOUNDED_SURFACE ( )  B_SPLINE_SURFACE ( 3, 1, ( 
 ( #9728, #24849 ),
 ( #27120, #4967 ),
 ( #27271, #5111 ),
 ( #13740, #22402 ) ),
 .UNSPECIFIED., .F., .F., .F. ) 
 B_SPLINE_SURFACE_WITH_KNOTS ( ( 4, 4 ),
 ( 2, 2 ),
 ( 0.000000000000000000, 1.000000000000000000 ),
 ( 0.000000000000000000, 1.000000000000000000 ),
 .UNSPECIFIED. ) 
 GEOMETRIC_REPRESENTATION_ITEM ( )  RATIONAL_B_SPLINE_SURFACE ( (
 ( 1.000000000000000000, 1.000000000000000000),
 ( 0.9593753223639863714, 0.9995975284513187731),
 ( 0.9593753223639863714, 0.9995975284513187731),
 ( 1.000000000000000000, 1.000000000000000000) ) ) 
 REPRESENTATION_ITEM ( '' )  SURFACE ( )  );
#18621 = ORIENTED_EDGE ( 'NONE', *, *, #3667, .T. ) ;
#18622 = CARTESIAN_POINT ( 'NONE',  ( -55.24390624410018802, -0.004896917417127438256, -0.009209468562451287102 ) ) ;
#18623 = CARTESIAN_POINT ( 'NONE',  ( -1.046936909428682450, 27.93981068760674802, 36.28616897897423144 ) ) ;
#18624 = ORIENTED_EDGE ( 'NONE', *, *, #17431, .T. ) ;
#18625 = EDGE_CURVE ( 'NONE', #26606, #20029, #25417, .T. ) ;
#18626 = ORIENTED_EDGE ( 'NONE', *, *, #16752, .F. ) ;
#18627 = ORIENTED_EDGE ( 'NONE', *, *, #3127, .T. ) ;
#18628 = B_SPLINE_CURVE_WITH_KNOTS ( 'NONE', 3,
 ( #17591, #6818, #15563, #2324, #11128, #9108 ),
 .UNSPECIFIED., .F., .F.,
 ( 4, 2, 4 ),
 ( 1.389302603484999005E-17, 0.0006311571484586018859, 0.001262314296917189894 ),
 .UNSPECIFIED. ) ;
#18629 = ADVANCED_FACE ( 'NONE', ( #11879 ), #23782, .F. ) ;
#18630 = CARTESIAN_POINT ( 'NONE',  ( 109.1721716018069515, 0.01706748904931388797, 0.0002019688922686267024 ) ) ;
#18631 = CARTESIAN_POINT ( 'NONE',  ( 16.75465622695650225, -140.8868039942616122, -19.47041796022383053 ) ) ;
#18632 = CARTESIAN_POINT ( 'NONE',  ( -1.583189561560255143, 44.83405390829672399, -11.94859433442917762 ) ) ;
#18633 = CARTESIAN_POINT ( 'NONE',  ( 30.59141879584288048, -111.3296561588015265, 33.33270905817553853 ) ) ;
#18634 = FACE_OUTER_BOUND ( 'NONE', #12202, .T. ) ;
#18635 = CARTESIAN_POINT ( 'NONE',  ( -25.21435515916025594, 1.749597353048488237E-16, -4.373993382621220594E-17 ) ) ;
#18636 = B_SPLINE_CURVE_WITH_KNOTS ( 'NONE', 3,
 ( #19819, #19545, #109, #17241, #4288, #17661, #8479, #13069, #1703, #10499 ),
 .UNSPECIFIED., .F., .F.,
 ( 4, 2, 2, 2, 4 ),
 ( 0.000000000000000000, 0.0003346267210630939765, 0.0006692534421261879529, 0.001003880163189281929, 0.001338506884252375906 ),
 .UNSPECIFIED. ) ;
#18637 = CARTESIAN_POINT ( 'NONE',  ( 109.1586059443104944, -0.005881369279875432732, 0.003930911098393195108 ) ) ;
#18638 = CARTESIAN_POINT ( 'NONE',  ( -1.155031165708886087, 25.28071330859886245, -38.31525684316149949 ) ) ;
#18639 = CARTESIAN_POINT ( 'NONE',  ( 109.1592201516379674, -0.007376275279032879113, 0.002720803050370542309 ) ) ;
#18640 = CARTESIAN_POINT ( 'NONE',  ( 6.224689322667630975, -134.1951906609234868, -62.55544044765383660 ) ) ;
#18641 = ORIENTED_EDGE ( 'NONE', *, *, #21531, .T. ) ;
#18642 = EDGE_LOOP ( 'NONE', ( #22178, #12867, #16930, #310 ) ) ;
#18643 = CARTESIAN_POINT ( 'NONE',  ( 2.433796855181205476, -28.83182736670433499, -142.6247129145651229 ) ) ;
#18645 = CARTESIAN_POINT ( 'NONE',  ( 25.73574536432415272, 76.18908113044869879, -83.41179791497782503 ) ) ;
#18644 = CARTESIAN_POINT ( 'NONE',  ( 24.22246935314087324, 0.000000000000000000, -111.9614997405030152 ) ) ;
#18646 = CARTESIAN_POINT ( 'NONE',  ( 1.833691583653494162, -85.58103979054574495, 117.1866391460183507 ) ) ;
#18647 = CARTESIAN_POINT ( 'NONE',  ( -1.539763995773692828, -35.94321074656915016, -29.16712963492449973 ) ) ;
#18648 = ORIENTED_EDGE ( 'NONE', *, *, #9204, .F. ) ;
#18649 = CARTESIAN_POINT ( 'NONE',  ( 26.11404676487259024, 36.06104232266452669, 107.3263591096431639 ) ) ;
#18650 = CARTESIAN_POINT ( 'NONE',  ( -1.031422197589711987, 1.530725436378101989, 45.78027046666441180 ) ) ;
#18651 = CARTESIAN_POINT ( 'NONE',  ( -1.031422197589711764, 28.14735071801743871, -36.13727897780136544 ) ) ;
#18652 = CARTESIAN_POINT ( 'NONE',  ( -21.41427618760447515, -7.777551129310266376, -29.81030852927063890 ) ) ;
#18653 = CARTESIAN_POINT ( 'NONE',  ( 109.1589550718175161, 0.004632048724982901558, 0.005994046294305926253 ) ) ;
#18654 = EDGE_CURVE ( 'NONE', #18677, #11017, #1692, .T. ) ;
#18655 = CONICAL_SURFACE ( 'NONE', #27837, 117.6351876552689504, 0.9945805576725580410 ) ;
#18656 = ORIENTED_EDGE ( 'NONE', *, *, #10514, .F. ) ;
#18657 = EDGE_CURVE ( 'NONE', #6378, #11630, #18514, .T. ) ;
#18658 = AXIS2_PLACEMENT_3D ( 'NONE', #7348, #20436, #22618 ) ;
#18659 = ADVANCED_FACE ( 'NONE', ( #8146 ), #16622, .T. ) ;
#18660 =( BOUNDED_SURFACE ( )  B_SPLINE_SURFACE ( 3, 1, ( 
 ( #18622, #12414 ),
 ( #5375, #1485 ),
 ( #16460, #5519 ),
 ( #14141, #3500 ) ),
 .UNSPECIFIED., .F., .F., .F. ) 
 B_SPLINE_SURFACE_WITH_KNOTS ( ( 4, 4 ),
 ( 2, 2 ),
 ( 0.000000000000000000, 1.000000000000000000 ),
 ( 0.000000000000000000, 1.000000000000000000 ),
 .UNSPECIFIED. ) 
 GEOMETRIC_REPRESENTATION_ITEM ( )  RATIONAL_B_SPLINE_SURFACE ( (
 ( 1.000000000000000000, 1.000000000000000000),
 ( 0.9934239774497837239, 0.8357310067453919133),
 ( 0.9934239774497837239, 0.8357310067453919133),
 ( 1.000000000000000000, 1.000000000000000000) ) ) 
 REPRESENTATION_ITEM ( '' )  SURFACE ( )  );
#18661 = ORIENTED_EDGE ( 'NONE', *, *, #223, .F. ) ;
#18662 = VERTEX_POINT ( 'NONE', #20800 ) ;
#18663 = CARTESIAN_POINT ( 'NONE',  ( 1.832998868059890096, -144.3700883710218363, 14.63705790013964680 ) ) ;
#18664 = ORIENTED_EDGE ( 'NONE', *, *, #4579, .F. ) ;
#18665 = APPLICATION_PROTOCOL_DEFINITION ( 'draft international standard', 'automotive_design', 1998, #9950 ) ;
#18666 = CARTESIAN_POINT ( 'NONE',  ( 2.433796855181205476, -60.50726454507993424, 132.3327394885229182 ) ) ;
#18667 = CARTESIAN_POINT ( 'NONE',  ( -55.25297051322618813, 0.01306918787467309905, 0.007247191603128975632 ) ) ;
#18668 = FACE_OUTER_BOUND ( 'NONE', #2400, .T. ) ;
#18669 = CARTESIAN_POINT ( 'NONE',  ( 1.833838850093452821, -107.8375718686133098, -97.09738119087818120 ) ) ;
#18670 = ORIENTED_EDGE ( 'NONE', *, *, #21425, .F. ) ;
#18671 = B_SPLINE_CURVE_WITH_KNOTS ( 'NONE', 3,
 ( #13181, #24016, #26428, #19532, #26018, #2100, #23745, #236 ),
 .UNSPECIFIED., .F., .F.,
 ( 4, 2, 2, 4 ),
 ( 0.000000000000000000, 0.0002429588503611182591, 0.0004859177007222365181, 0.0009718354014444730363 ),
 .UNSPECIFIED. ) ;
#18672 = FACE_OUTER_BOUND ( 'NONE', #26400, .T. ) ;
#18674 = CARTESIAN_POINT ( 'NONE',  ( -4.473127245936431073, -41.70021447285034810, 26.34600523034583119 ) ) ;
#18673 = CARTESIAN_POINT ( 'NONE',  ( 21.16825799904900407, -135.0813719997368310, -9.757279788664144249 ) ) ;
#18675 = CARTESIAN_POINT ( 'NONE',  ( 10.93730112725932635, 0.000000000000000000, 0.000000000000000000 ) ) ;
#18676 = ORIENTED_EDGE ( 'NONE', *, *, #10421, .T. ) ;
#18677 = VERTEX_POINT ( 'NONE', #21766 ) ;
#18678 = ORIENTED_EDGE ( 'NONE', *, *, #18346, .T. ) ;
#18679 = CARTESIAN_POINT ( 'NONE',  ( -16.86833981943423666, 7.884812276282103127, -43.51541671545727041 ) ) ;
#18680 = DIRECTION ( 'NONE',  ( 0.7071067811865485719, 0.000000000000000000, -0.7071067811865465735 ) ) ;
#18682 = CARTESIAN_POINT ( 'NONE',  ( -1.031422197589716205, 37.93675465142509751, 25.67058493451402157 ) ) ;
#18681 = CARTESIAN_POINT ( 'NONE',  ( 32.73300124599734318, 92.86301839380026024, 72.21147546950587071 ) ) ;
#18683 = CARTESIAN_POINT ( 'NONE',  ( -20.38016308990357217, -7.753479680700753107, 28.74660391518353109 ) ) ;
#18684 = CARTESIAN_POINT ( 'NONE',  ( -1.155001620486249214, -12.20337535396710749, -44.25209926692303952 ) ) ;
#18685 = EDGE_LOOP ( 'NONE', ( #10684, #17294, #7194, #19314 ) ) ;
#18686 = CARTESIAN_POINT ( 'NONE',  ( -20.90916690077966322, 35.64494649500682755, -17.17795951644668762 ) ) ;
#18687 = CARTESIAN_POINT ( 'NONE',  ( 28.43349137099831481, -124.1860347533534963, 4.052139611197981495 ) ) ;
#18688 = ORIENTED_EDGE ( 'NONE', *, *, #22365, .T. ) ;
#18689 = CARTESIAN_POINT ( 'NONE',  ( -1.058197053496171769, -42.99116279335166269, -15.81317659443667445 ) ) ;
#18690 = CARTESIAN_POINT ( 'NONE',  ( 1.832998868059858122, 44.33343224355235890, 138.1720401012268553 ) ) ;
#18691 = CARTESIAN_POINT ( 'NONE',  ( 26.11404676487257603, 45.01677474591409833, 103.8885755249570906 ) ) ;
#18692 = ADVANCED_FACE ( 'NONE', ( #14311 ), #17839, .F. ) ;
#18693 = CARTESIAN_POINT ( 'NONE',  ( 25.98552792386799126, -67.36997957637598233, -90.89136171349154836 ) ) ;
#18694 = CARTESIAN_POINT ( 'NONE',  ( 1.832998868059858122, -72.09222286250995637, -125.9352106559991427 ) ) ;
#18695 = CARTESIAN_POINT ( 'NONE',  ( 1.893872463202069811, -108.5026245911425207, 96.41404152942899941 ) ) ;
#18696 = CARTESIAN_POINT ( 'NONE',  ( 9.884929003653626367, -139.1775604444700321, -57.36421526887299649 ) ) ;
#18697 = ORIENTED_EDGE ( 'NONE', *, *, #15631, .F. ) ;
#18698 = CARTESIAN_POINT ( 'NONE',  ( 24.22246935314087324, 0.000000000000000000, 0.000000000000000000 ) ) ;
#18700 = EDGE_CURVE ( 'NONE', #4838, #195, #12734, .T. ) ;
#18699 = DIRECTION ( 'NONE',  ( 0.000000000000000000, 0.000000000000000000, 1.000000000000000000 ) ) ;
#18701 = CARTESIAN_POINT ( 'NONE',  ( -1.058197053496158890, 12.47644286888577270, 44.07533330186774378 ) ) ;
#18702 = EDGE_CURVE ( 'NONE', #600, #12444, #13101, .T. ) ;
#18703 = ORIENTED_EDGE ( 'NONE', *, *, #15313, .T. ) ;
#18704 = VERTEX_POINT ( 'NONE', #7871 ) ;
#18705 =( BOUNDED_SURFACE ( )  B_SPLINE_SURFACE ( 3, 1, ( 
 ( #10133, #3784 ),
 ( #21042, #25537 ),
 ( #6767, #23240 ),
 ( #3492, #12276 ) ),
 .UNSPECIFIED., .F., .F., .F. ) 
 B_SPLINE_SURFACE_WITH_KNOTS ( ( 4, 4 ),
 ( 2, 2 ),
 ( 0.000000000000000000, 1.000000000000000000 ),
 ( 0.000000000000000000, 1.000000000000000000 ),
 .UNSPECIFIED. ) 
 GEOMETRIC_REPRESENTATION_ITEM ( )  RATIONAL_B_SPLINE_SURFACE ( (
 ( 1.000000000000000000, 1.000000000000000000),
 ( 0.7789835883360578528, 0.9689951854195403280),
 ( 0.7789835883360578528, 0.9689951854195403280),
 ( 1.000000000000000000, 1.000000000000000000) ) ) 
 REPRESENTATION_ITEM ( '' )  SURFACE ( )  );
#18706 = CARTESIAN_POINT ( 'NONE',  ( 2.430230287190572103, 125.2872625092162338, 74.01081053031143142 ) ) ;
#18707 = VERTEX_POINT ( 'NONE', #17426 ) ;
#18708 = CARTESIAN_POINT ( 'NONE',  ( 2.063896406836609909, 108.8509294491465198, 96.20114399516431547 ) ) ;
#18709 = CARTESIAN_POINT ( 'NONE',  ( 1.832998868059890096, 144.2584710144582516, -15.69902610990226144 ) ) ;
#18710 = VECTOR ( 'NONE', #20112, 999.9999999999998863 ) ;
#18711 = CARTESIAN_POINT ( 'NONE',  ( -4.780792508754330150, 48.13366140756558309, -11.68149851467477340 ) ) ;
#18712 = CARTESIAN_POINT ( 'NONE',  ( 8.186469777911009160, 118.7566730872913752, -90.56875928602613612 ) ) ;
#18713 = LINE ( 'NONE', #20873, #15245 ) ;
#18714 = CARTESIAN_POINT ( 'NONE',  ( 2.108393763691183587, -116.7869873529603808, -86.43392821214699495 ) ) ;
#18715 = VERTEX_POINT ( 'NONE', #25424 ) ;
#18716 = VERTEX_POINT ( 'NONE', #5400 ) ;
#18717 = CARTESIAN_POINT ( 'NONE',  ( -10.86508079875782329, -46.07061504567103327, -22.20099862734805996 ) ) ;
#18718 = CARTESIAN_POINT ( 'NONE',  ( 2.108393763691185363, 107.1124103264149738, 98.16799842733286141 ) ) ;
#18719 = CARTESIAN_POINT ( 'NONE',  ( -21.81686047589425925, 34.70276904128910189, 16.72402253294277230 ) ) ;
#18720 = CARTESIAN_POINT ( 'NONE',  ( -1.619063947482201282, 11.94059994246159384, -44.80407745103787676 ) ) ;
#18721 = CARTESIAN_POINT ( 'NONE',  ( 1.832998868059858122, -107.4798986104853356, -97.49378069860905782 ) ) ;
#18722 = CARTESIAN_POINT ( 'NONE',  ( -5.986830583229486358, 50.53158596890444443, -4.559539818181313819 ) ) ;
#18723 = CARTESIAN_POINT ( 'NONE',  ( 109.1589550718174877, -0.005994046294307837919, -0.004632048724973697983 ) ) ;
#18724 = ORIENTED_EDGE ( 'NONE', *, *, #19589, .T. ) ;
#18725 = CARTESIAN_POINT ( 'NONE',  ( -55.24340739397742084, -0.009386184976286139278, -0.003826481709803953961 ) ) ;
#18726 = CARTESIAN_POINT ( 'NONE',  ( -25.21435515916043357, -25.00736669481038987, -23.92354251275926558 ) ) ;
#18727 = LINE ( 'NONE', #11962, #5074 ) ;
#18728 = EDGE_CURVE ( 'NONE', #14998, #17856, #14164, .T. ) ;
#18729 = ADVANCED_FACE ( 'NONE', ( #3245 ), #9744, .T. ) ;
#18730 = CARTESIAN_POINT ( 'NONE',  ( 32.73300124599735739, -44.31599526638029118, 108.9684813982487412 ) ) ;
#18731 = VERTEX_POINT ( 'NONE', #25273 ) ;
#18732 = VERTEX_POINT ( 'NONE', #3387 ) ;
#18734 = EDGE_CURVE ( 'NONE', #26383, #22553, #394, .T. ) ;
#18733 = CARTESIAN_POINT ( 'NONE',  ( 109.1586059443104944, 0.006637156007973981676, 0.002447596125905610390 ) ) ;
#18735 = CARTESIAN_POINT ( 'NONE',  ( 109.1592201516379674, 0.005485778713193748164, -0.005631912476305715558 ) ) ;
#18736 = ORIENTED_EDGE ( 'NONE', *, *, #20176, .T. ) ;
#18737 = EDGE_CURVE ( 'NONE', #8126, #7229, #6518, .T. ) ;
#18738 = VERTEX_POINT ( 'NONE', #9391 ) ;
#18739 = EDGE_LOOP ( 'NONE', ( #6810, #27475, #21929, #27126 ) ) ;
#18740 = CARTESIAN_POINT ( 'NONE',  ( -7.078251931573406708, 20.86696228105292761, 47.71415099571781582 ) ) ;
#18741 = CARTESIAN_POINT ( 'NONE',  ( 28.37644542392835589, -98.15613422114043374, -76.32685750075110320 ) ) ;
#18742 = CARTESIAN_POINT ( 'NONE',  ( -55.24390624410018802, 0.004896917417128144288, 0.009209468562451129242 ) ) ;
#18743 = CARTESIAN_POINT ( 'NONE',  ( -23.79248802219729697, -24.83956736572394064, 22.01156985585195258 ) ) ;
#18744 = CARTESIAN_POINT ( 'NONE',  ( -20.20700224038492721, 16.58740185276746359, 24.51628800869029234 ) ) ;
#18745 = FACE_OUTER_BOUND ( 'NONE', #24739, .T. ) ;
#18746 = CARTESIAN_POINT ( 'NONE',  ( 25.64703792032468854, 84.00887408969053638, 75.44170528134917220 ) ) ;
#18747 =( BOUNDED_SURFACE ( )  B_SPLINE_SURFACE ( 3, 1, ( 
 ( #26745, #4589 ),
 ( #10940, #13222 ),
 ( #28472, #22011 ),
 ( #22309, #2572 ) ),
 .UNSPECIFIED., .F., .F., .F. ) 
 B_SPLINE_SURFACE_WITH_KNOTS ( ( 4, 4 ),
 ( 2, 2 ),
 ( 0.000000000000000000, 1.000000000000000000 ),
 ( 0.000000000000000000, 1.000000000000000000 ),
 .UNSPECIFIED. ) 
 GEOMETRIC_REPRESENTATION_ITEM ( )  RATIONAL_B_SPLINE_SURFACE ( (
 ( 1.000000000000000000, 1.000000000000000000),
 ( 0.6386103224230316178, 0.9954351624131538845),
 ( 0.6386103224230316178, 0.9954351624131538845),
 ( 1.000000000000000000, 1.000000000000000000) ) ) 
 REPRESENTATION_ITEM ( '' )  SURFACE ( )  );
#18748 = CARTESIAN_POINT ( 'NONE',  ( -20.20612092514784308, 24.59769888281557471, 16.46550332780499559 ) ) ;
#18749 = CARTESIAN_POINT ( 'NONE',  ( -20.20612091757426043, 24.59769958242388910, -16.46550228026404028 ) ) ;
#18750 = CARTESIAN_POINT ( 'NONE',  ( -20.57838717382308147, -28.96176188950213870, 7.715628353033985753 ) ) ;
#18751 = CARTESIAN_POINT ( 'NONE',  ( 32.73300124599736449, -114.2056417606550127, 28.19767303745571496 ) ) ;
#18752 = CARTESIAN_POINT ( 'NONE',  ( -1.323439229708146536, -25.17120723334064891, 38.58845475799796532 ) ) ;
#18753 = ADVANCED_FACE ( 'NONE', ( #20157 ), #4911, .F. ) ;
#18754 = CARTESIAN_POINT ( 'NONE',  ( 1.833485406944057594, 15.69895494453384721, 144.2578170162063884 ) ) ;
#18755 = CARTESIAN_POINT ( 'NONE',  ( 2.430230287190572103, -144.5585181921884725, -16.65331920325888149 ) ) ;
#18756 = CARTESIAN_POINT ( 'NONE',  ( 55.79472521941426777, 53.57698701322215129, 49.22042574086442812 ) ) ;
#18757 = LINE ( 'NONE', #5821, #10067 ) ;
#18758 = VERTEX_POINT ( 'NONE', #20018 ) ;
#18759 = CARTESIAN_POINT ( 'NONE',  ( -1.058473599757816963, 25.48501014712399737, -38.06357893967437889 ) ) ;
#18760 = CIRCLE ( 'NONE', #10950, 44.74884827092600403 ) ;
#18761 = ORIENTED_EDGE ( 'NONE', *, *, #19329, .T. ) ;
#18763 = ADVANCED_FACE ( 'NONE', ( #593 ), #5599, .T. ) ;
#18762 = CARTESIAN_POINT ( 'NONE',  ( -8.786685647604885574, 6.096987947571466530E-17, -1.524246986892866633E-17 ) ) ;
#18764 = CARTESIAN_POINT ( 'NONE',  ( -1.050230346682680560, 26.91946103437159721, 37.05264119692660785 ) ) ;
#18765 = ORIENTED_EDGE ( 'NONE', *, *, #22200, .F. ) ;
#18766 = ADVANCED_FACE ( 'NONE', ( #20302 ), #4826, .F. ) ;
#18767 = ORIENTED_EDGE ( 'NONE', *, *, #9432, .T. ) ;
#18768 = ORIENTED_EDGE ( 'NONE', *, *, #28227, .T. ) ;
#18769 = CARTESIAN_POINT ( 'NONE',  ( 32.73300124599735739, 44.31599526637956643, 108.9684813982490539 ) ) ;
#18770 = AXIS2_PLACEMENT_3D ( 'NONE', #376, #17920, #28303 ) ;
#18771 = VECTOR ( 'NONE', #18204, 999.9999999999998863 ) ;
#18772 = CARTESIAN_POINT ( 'NONE',  ( -15.02187109954782862, -41.75590530176324222, -20.12219089991075904 ) ) ;
#18773 = CARTESIAN_POINT ( 'NONE',  ( -1.058473599757821404, -1.755404039369745650, -45.77379534793243465 ) ) ;
#18774 = CARTESIAN_POINT ( 'NONE',  ( 2.063896406836605024, 13.84738934186190917, 144.6078654718902214 ) ) ;
#18775 = CARTESIAN_POINT ( 'NONE',  ( 109.1589550718174877, -0.001793588804091283831, 0.007359857714023712583 ) ) ;
#18777 = CARTESIAN_POINT ( 'NONE',  ( 109.1592201516379674, 0.006649399203953463774, -0.004194960840990087647 ) ) ;
#18776 = CARTESIAN_POINT ( 'NONE',  ( -25.21435515916043357, -16.39063784838764093, -30.48034229288631991 ) ) ;
#18778 = CARTESIAN_POINT ( 'NONE',  ( -7.733045908741329022, -47.75066202881810540, -21.80378472388470001 ) ) ;
#18779 =( BOUNDED_SURFACE ( )  B_SPLINE_SURFACE ( 3, 1, ( 
 ( #27743, #20680 ),
 ( #3135, #11911 ),
 ( #3278, #18674 ),
 ( #20964, #12059 ) ),
 .UNSPECIFIED., .F., .F., .F. ) 
 B_SPLINE_SURFACE_WITH_KNOTS ( ( 4, 4 ),
 ( 2, 2 ),
 ( 0.000000000000000000, 1.000000000000000000 ),
 ( 0.000000000000000000, 1.000000000000000000 ),
 .UNSPECIFIED. ) 
 GEOMETRIC_REPRESENTATION_ITEM ( )  RATIONAL_B_SPLINE_SURFACE ( (
 ( 1.000000000000000000, 1.000000000000000000),
 ( 0.7789835883360578528, 0.9689951854195403280),
 ( 0.7789835883360578528, 0.9689951854195403280),
 ( 1.000000000000000000, 1.000000000000000000) ) ) 
 REPRESENTATION_ITEM ( '' )  SURFACE ( )  );
#18780 = ORIENTED_EDGE ( 'NONE', *, *, #22905, .F. ) ;
#18781 = ORIENTED_EDGE ( 'NONE', *, *, #27490, .T. ) ;
#18782 = CARTESIAN_POINT ( 'NONE',  ( 25.64708010899968116, -107.4019003251853377, -34.83947233573784530 ) ) ;
#18784 = CARTESIAN_POINT ( 'NONE',  ( 25.98107933586719653, 76.50887835172657958, -83.34070894055800238 ) ) ;
#18783 = CARTESIAN_POINT ( 'NONE',  ( 1.834118845439484335, -30.34413640949595603, -141.9019470378990775 ) ) ;
#18785 = EDGE_CURVE ( 'NONE', #13365, #26863, #10376, .T. ) ;
#18786 = CARTESIAN_POINT ( 'NONE',  ( -20.57838717382308147, -7.715628353033886278, -28.96176188950215646 ) ) ;
#18787 = CARTESIAN_POINT ( 'NONE',  ( 25.64681081121879203, 11.38886654529823694, -112.3352186517029594 ) ) ;
#18788 = CARTESIAN_POINT ( 'NONE',  ( -4.473127245936431073, 18.25038884639870673, -45.82513704981550262 ) ) ;
#18789 = B_SPLINE_CURVE_WITH_KNOTS ( 'NONE', 3,
 ( #16194, #23132, #16337, #12172, #12441, #25134, #1362, #14167 ),
 .UNSPECIFIED., .F., .F.,
 ( 4, 2, 2, 4 ),
 ( 0.000000000000000000, 0.002761524886576648043, 0.005523049773153296087, 0.01104609954630659217 ),
 .UNSPECIFIED. ) ;
#18790 = ORIENTED_EDGE ( 'NONE', *, *, #5781, .F. ) ;
#18791 = CARTESIAN_POINT ( 'NONE',  ( 25.64692232868535626, 91.15460455808917573, -66.63160215461171276 ) ) ;
#18793 = EDGE_CURVE ( 'NONE', #10995, #16671, #25459, .T. ) ;
#18792 = CARTESIAN_POINT ( 'NONE',  ( 109.1587776205901861, -0.007151389024635742414, 0.001605238040368439862 ) ) ;
#18794 = CARTESIAN_POINT ( 'NONE',  ( 32.73300124599734318, 115.8010721414084117, 20.69176323058669809 ) ) ;
#18795 = ORIENTED_EDGE ( 'NONE', *, *, #20535, .T. ) ;
#18796 = ADVANCED_FACE ( 'NONE', ( #9232 ), #14737, .F. ) ;
#18797 = CARTESIAN_POINT ( 'NONE',  ( -7.711401346138398338, -51.42722225669428582, -10.36923727626100522 ) ) ;
#18798 = CONICAL_SURFACE ( 'NONE', #19246, 34.60786435723138510, 0.8559913436420825139 ) ;
#18799 = ORIENTED_EDGE ( 'NONE', *, *, #7300, .F. ) ;
#18800 = CARTESIAN_POINT ( 'NONE',  ( 2.433796855181233454, -86.69855925933894980, -116.8607839509065371 ) ) ;
#18801 = ORIENTED_EDGE ( 'NONE', *, *, #9862, .T. ) ;
#18802 = CARTESIAN_POINT ( 'NONE',  ( -22.23226125620944771, 26.80886670319662102, 16.78323347921887887 ) ) ;
#18803 = DIRECTION ( 'NONE',  ( 0.5914120900931444380, 0.6942916636548107645, 0.4101107478122142935 ) ) ;
#18804 = CARTESIAN_POINT ( 'NONE',  ( 936.3835875555738539, 950.5262624572891355, 1447.888130612201621 ) ) ;
#18805 = CARTESIAN_POINT ( 'NONE',  ( -55.24390624410018802, -0.007245494385991098352, -0.007503127514281985981 ) ) ;
#18806 = CARTESIAN_POINT ( 'NONE',  ( -1.583189561560253589, -36.01941156322766346, 29.24830400313204848 ) ) ;
#18807 = CARTESIAN_POINT ( 'NONE',  ( 25.64681081121879203, -107.2555980796243773, 35.28660243342513070 ) ) ;
#18808 = LINE ( 'NONE', #27296, #10162 ) ;
#18809 = CARTESIAN_POINT ( 'NONE',  ( -20.21097721712958872, 28.26295595852185727, -8.835581498567558256 ) ) ;
#18810 = ORIENTED_EDGE ( 'NONE', *, *, #22532, .T. ) ;
#18811 = ADVANCED_FACE ( 'NONE', ( #2161 ), #6973, .T. ) ;
#18812 = CARTESIAN_POINT ( 'NONE',  ( 10.93730112725990011, -146.7718404940640653, -36.23586118136687162 ) ) ;
#18814 = CARTESIAN_POINT ( 'NONE',  ( 2.433796855181219243, -144.5536872373193376, 16.65276281464516828 ) ) ;
#18813 = CARTESIAN_POINT ( 'NONE',  ( -20.21097721712958872, -28.05863618200116250, -9.464413111084637009 ) ) ;
#18815 = DIRECTION ( 'NONE',  ( 1.000000000000000000, -6.938893903907226837E-18, 1.734723475976806709E-18 ) ) ;
#18816 = ORIENTED_EDGE ( 'NONE', *, *, #12267, .F. ) ;
#18817 = EDGE_LOOP ( 'NONE', ( #18915, #4594, #1541, #17299 ) ) ;
#18818 = ORIENTED_EDGE ( 'NONE', *, *, #6536, .T. ) ;
#18819 = CARTESIAN_POINT ( 'NONE',  ( -55.24300891470650754, -0.006048736206179085827, -0.007734635432136639961 ) ) ;
#18820 = LINE ( 'NONE', #27590, #2441 ) ;
#18822 = CARTESIAN_POINT ( 'NONE',  ( 14.74894986621300141, -1.023413983156985299E-16, 2.558534957892463246E-17 ) ) ;
#18821 = CARTESIAN_POINT ( 'NONE',  ( 119.2224693531408803, 90.00000000000005684, -19.99999999999998934 ) ) ;
#18823 = EDGE_CURVE ( 'NONE', #20516, #10945, #9337, .T. ) ;
#18824 = B_SPLINE_CURVE_WITH_KNOTS ( 'NONE', 3,
 ( #6070, #21585, #17124, #21447, #15091, #19286 ),
 .UNSPECIFIED., .F., .F.,
 ( 4, 2, 4 ),
 ( 2.394688213745465202E-17, 0.0006311636237756846571, 0.001262327247551345028 ),
 .UNSPECIFIED. ) ;
#18825 = CARTESIAN_POINT ( 'NONE',  ( -1.046936909428679785, -43.14407378092982981, 15.35929614323710801 ) ) ;
#18826 = CARTESIAN_POINT ( 'NONE',  ( -1.045287976400383290, -12.68782741917353185, -44.00138577190637079 ) ) ;
#18827 = ORIENTED_EDGE ( 'NONE', *, *, #17303, .F. ) ;
#18828 = CARTESIAN_POINT ( 'NONE',  ( 25.64681081121879203, -112.2483031020012589, -12.21581276189922427 ) ) ;
#18829 = EDGE_CURVE ( 'NONE', #17799, #11098, #1427, .T. ) ;
#18830 = DIRECTION ( 'NONE',  ( 0.000000000000000000, 0.000000000000000000, 1.000000000000000000 ) ) ;
#18831 = VERTEX_POINT ( 'NONE', #20736 ) ;
#18832 = CARTESIAN_POINT ( 'NONE',  ( -10.86508079875781263, 45.04061326950873223, -24.22249093393315533 ) ) ;
#18833 = CARTESIAN_POINT ( 'NONE',  ( -55.24390624410018802, 0.007503127514278223366, 0.007245494385991344682 ) ) ;
#18834 = CARTESIAN_POINT ( 'NONE',  ( -1.044556982611280604, 44.03203163107544071, 12.57890920527730394 ) ) ;
#18835 = CARTESIAN_POINT ( 'NONE',  ( 5.340103579038175674, -57.86178752084584431, 135.6222865281527277 ) ) ;
#18836 = CARTESIAN_POINT ( 'NONE',  ( 25.70243777736187596, 75.03063812272054633, 84.42566495012475514 ) ) ;
#18837 = CARTESIAN_POINT ( 'NONE',  ( 2.430230287190581429, -126.7388733285349787, 71.49654683843465364 ) ) ;
#18838 = FACE_OUTER_BOUND ( 'NONE', #3221, .T. ) ;
#18839 = ORIENTED_EDGE ( 'NONE', *, *, #15719, .F. ) ;
#18840 = CARTESIAN_POINT ( 'NONE',  ( 109.1778270068192853, -0.006682187084639273911, -0.006489198140358696729 ) ) ;
#18841 =( BOUNDED_SURFACE ( )  B_SPLINE_SURFACE ( 3, 1, ( 
 ( #8827, #6384 ),
 ( #9104, #17864 ),
 ( #19897, #13409 ),
 ( #13266, #17441 ) ),
 .UNSPECIFIED., .F., .F., .F. ) 
 B_SPLINE_SURFACE_WITH_KNOTS ( ( 4, 4 ),
 ( 2, 2 ),
 ( 0.000000000000000000, 1.000000000000000000 ),
 ( 0.000000000000000000, 1.000000000000000000 ),
 .UNSPECIFIED. ) 
 GEOMETRIC_REPRESENTATION_ITEM ( )  RATIONAL_B_SPLINE_SURFACE ( (
 ( 1.000000000000000000, 1.000000000000000000),
 ( 0.9956975270656955868, 0.8568959468854907557),
 ( 0.9956975270656955868, 0.8568959468854907557),
 ( 1.000000000000000000, 1.000000000000000000) ) ) 
 REPRESENTATION_ITEM ( '' )  SURFACE ( )  );
#18842 = CARTESIAN_POINT ( 'NONE',  ( 25.69398547355837437, 110.3177996916217438, -24.20764173643295436 ) ) ;
#18843 = B_SPLINE_CURVE_WITH_KNOTS ( 'NONE', 3,
 ( #2295, #17982, #11099, #26485, #7083, #15843 ),
 .UNSPECIFIED., .F., .F.,
 ( 4, 2, 4 ),
 ( 6.505213034913026604E-18, 0.0006311636237756838982, 0.001262327247551370615 ),
 .UNSPECIFIED. ) ;
#18844 = VERTEX_POINT ( 'NONE', #23213 ) ;
#18845 = CARTESIAN_POINT ( 'NONE',  ( -1.113548883309551485, -1.968251867498553409, 45.82026503946953255 ) ) ;
#18846 = VECTOR ( 'NONE', #24688, 1000.000000000000114 ) ;
#18847 = ORIENTED_EDGE ( 'NONE', *, *, #1840, .T. ) ;
#18848 = CARTESIAN_POINT ( 'NONE',  ( -1.048996300304514850, -45.79145529752467070, 0.7649764263856586588 ) ) ;
#18849 = CARTESIAN_POINT ( 'NONE',  ( 25.64681081121879203, -102.9795863647031666, 46.30456157731292421 ) ) ;
#18850 = CARTESIAN_POINT ( 'NONE',  ( -25.21435515916043713, -15.02493970636168896, -31.17620025257581062 ) ) ;
#18851 = EDGE_CURVE ( 'NONE', #5379, #15303, #22387, .T. ) ;
#18852 = ORIENTED_EDGE ( 'NONE', *, *, #2993, .T. ) ;
#18853 = CARTESIAN_POINT ( 'NONE',  ( 1.832998868059858122, 145.1092030902949830, 0.5339089137753076919 ) ) ;
#18854 = CARTESIAN_POINT ( 'NONE',  ( 1.833721034905619884, -125.8463597577922428, -72.24642519953907538 ) ) ;
#18855 = ADVANCED_FACE ( 'NONE', ( #18430 ), #23083, .T. ) ;
#18856 = CARTESIAN_POINT ( 'NONE',  ( 25.98107933586725338, -35.99661810150939090, 107.2544904356371092 ) ) ;
#18857 = CARTESIAN_POINT ( 'NONE',  ( 55.49584447822657296, 53.73688382046329082, -48.74506217377828676 ) ) ;
#18858 = ORIENTED_EDGE ( 'NONE', *, *, #11273, .T. ) ;
#18859 = ADVANCED_FACE ( 'NONE', ( #14402 ), #11556, .T. ) ;
#18860 = EDGE_LOOP ( 'NONE', ( #11833, #7828, #10179, #6686 ) ) ;
#18861 = CARTESIAN_POINT ( 'NONE',  ( 1.833691583653524804, -30.51806994139693785, 141.8642667235907311 ) ) ;
#18862 = B_SPLINE_CURVE_WITH_KNOTS ( 'NONE', 3,
 ( #14657, #8604, #23887, #12638, #8474, #23463 ),
 .UNSPECIFIED., .F., .F.,
 ( 4, 2, 4 ),
 ( 5.637851296924623057E-18, 0.0006311636237756782604, 0.001262327247551351100 ),
 .UNSPECIFIED. ) ;
#18863 = DIRECTION ( 'NONE',  ( 0.000000000000000000, 5.223019709708233256E-21, -1.000000000000000000 ) ) ;
#18864 = CARTESIAN_POINT ( 'NONE',  ( 26.28373643307404350, -78.30371666786325591, -100.6987277884692418 ) ) ;
#18865 = VECTOR ( 'NONE', #12956, 1000.000000000000000 ) ;
#18866 = CARTESIAN_POINT ( 'NONE',  ( 119.2224693531408803, 0.000000000000000000, 0.000000000000000000 ) ) ;
#18867 = CARTESIAN_POINT ( 'NONE',  ( 1.833485406944057594, 107.4794113447422603, -97.49333871408586560 ) ) ;
#18868 = CARTESIAN_POINT ( 'NONE',  ( -2.911734481061402757, 47.57875121082948766, -2.802366807346352129 ) ) ;
#18869 = VERTEX_POINT ( 'NONE', #7231 ) ;
#18870 = CARTESIAN_POINT ( 'NONE',  ( 5.340103556456326395, 117.9209211572685518, 88.52145167812622617 ) ) ;
#18871 = FACE_OUTER_BOUND ( 'NONE', #19711, .T. ) ;
#18872 = CARTESIAN_POINT ( 'NONE',  ( 25.64681081121879203, -11.38886654529598275, -112.3352186517031726 ) ) ;
#18873 = CARTESIAN_POINT ( 'NONE',  ( -8.786685647604890903, 52.67761315067286176, -9.545808661480789326 ) ) ;
#18874 = CARTESIAN_POINT ( 'NONE',  ( 109.1589550718174877, 0.003284595046925658200, -0.006826119083824085977 ) ) ;
#18875 = ORIENTED_EDGE ( 'NONE', *, *, #25823, .T. ) ;
#18876 = CARTESIAN_POINT ( 'NONE',  ( 25.81918753295377300, -57.31966094783135901, -97.41320410180144052 ) ) ;
#18877 = CARTESIAN_POINT ( 'NONE',  ( 1.831572820252009626, -29.20415387690664133, 142.1425225354579140 ) ) ;
#18878 = ORIENTED_EDGE ( 'NONE', *, *, #16867, .F. ) ;
#18879 = B_SPLINE_CURVE_WITH_KNOTS ( 'NONE', 3,
 ( #12807, #3902, #6344, #1597, #21457, #14835, #23786, #23495, #25786, #10397 ),
 .UNSPECIFIED., .F., .F.,
 ( 4, 3, 3, 4 ),
 ( 1.387778780781445676E-17, 0.0002669560319015634731, 0.0005492286108966289854, 0.0008315040496093382841 ),
 .UNSPECIFIED. ) ;
#18880 = EDGE_LOOP ( 'NONE', ( #18576, #2642, #11557, #6205 ) ) ;
#18881 = ORIENTED_EDGE ( 'NONE', *, *, #23679, .T. ) ;
#18882 = CIRCLE ( 'NONE', #13366, 53.53553390275978785 ) ;
#18883 = AXIS2_PLACEMENT_3D ( 'NONE', #4142, #9139, #15750 ) ;
#18884 = B_SPLINE_CURVE_WITH_KNOTS ( 'NONE', 3,
 ( #19109, #27589, #1542, #23302, #18679, #14778, #25870 ),
 .UNSPECIFIED., .F., .F.,
 ( 4, 3, 4 ),
 ( 0.000000000000000000, 0.006568092053401815289, 0.02506242213020845253 ),
 .UNSPECIFIED. ) ;
#18885 = CARTESIAN_POINT ( 'NONE',  ( 25.64692232868535626, -110.5112661748243710, -23.15582834340398222 ) ) ;
#18886 = CARTESIAN_POINT ( 'NONE',  ( 13.84597867724964004, -115.8103190066268837, -90.05293531772760218 ) ) ;
#18887 = CIRCLE ( 'NONE', #17483, 12.50000000000000000 ) ;
#18888 = EDGE_CURVE ( 'NONE', #25030, #449, #24915, .T. ) ;
#18889 = EDGE_CURVE ( 'NONE', #22240, #11755, #25375, .T. ) ;
#18890 = CARTESIAN_POINT ( 'NONE',  ( 1.833721034905660296, 29.82176961967109818, -142.0123736691683973 ) ) ;
#18891 = CARTESIAN_POINT ( 'NONE',  ( -1.113427685307000203, 1.967672929087815881, 45.82016658690749722 ) ) ;
#18892 = ORIENTED_EDGE ( 'NONE', *, *, #8265, .T. ) ;
#18893 = EDGE_CURVE ( 'NONE', #8964, #10429, #2832, .T. ) ;
#18894 = CARTESIAN_POINT ( 'NONE',  ( 2.433796855181205476, -132.3327394885227477, -60.50726454508036056 ) ) ;
#18895 = CARTESIAN_POINT ( 'NONE',  ( -1.619063947482197729, 46.30105812165548684, -2.489035965910316506 ) ) ;
#18896 = B_SPLINE_CURVE_WITH_KNOTS ( 'NONE', 3,
 ( #12505, #10242, #3455, #1707 ),
 .UNSPECIFIED., .F., .F.,
 ( 4, 4 ),
 ( 3.214625617059125298E-16, 0.01077107486149828444 ),
 .UNSPECIFIED. ) ;
#18897 = CARTESIAN_POINT ( 'NONE',  ( 32.73300124599732186, 0.000000000000000000, 0.000000000000000000 ) ) ;
#18898 = EDGE_CURVE ( 'NONE', #28309, #26876, #19832, .T. ) ;
#18899 = CARTESIAN_POINT ( 'NONE',  ( 28.37603512858449051, -25.60641750873823952, -111.8384105897144707 ) ) ;
#18900 = CARTESIAN_POINT ( 'NONE',  ( 21.16825799904911776, 46.02882515936479280, 127.3716170292823477 ) ) ;
#18901 = CARTESIAN_POINT ( 'NONE',  ( 25.64703792032471341, -11.65444440562256823, 112.3081285890370111 ) ) ;
#18902 = AXIS2_PLACEMENT_3D ( 'NONE', #8019, #5844, #14604 ) ;
#18903 = CARTESIAN_POINT ( 'NONE',  ( 5.340103579038250281, -147.4316330314913159, 2.303180387974738341 ) ) ;
#18904 = CARTESIAN_POINT ( 'NONE',  ( -1.619063947482194177, 35.99532424477422410, 29.22875152547716482 ) ) ;
#18905 = CARTESIAN_POINT ( 'NONE',  ( 25.64706015949225915, -0.09919735511113483839, -112.9111942614908060 ) ) ;
#18906 = CARTESIAN_POINT ( 'NONE',  ( -25.21435515916043713, 6.169479169075932745, 34.05351380035326514 ) ) ;
#18907 = CARTESIAN_POINT ( 'NONE',  ( -4.473127245936434626, 45.82513704981544578, -18.25038884639885950 ) ) ;
#18908 = VERTEX_POINT ( 'NONE', #7668 ) ;
#18909 = AXIS2_PLACEMENT_3D ( 'NONE', #17626, #7144, #11581 ) ;
#18910 = EDGE_LOOP ( 'NONE', ( #1793, #26856, #11009, #15533 ) ) ;
#18911 = CARTESIAN_POINT ( 'NONE',  ( -1.046935749540010674, 43.93230528057182482, -12.93334586714193790 ) ) ;
#18913 = ORIENTED_EDGE ( 'NONE', *, *, #18054, .F. ) ;
#18912 = CARTESIAN_POINT ( 'NONE',  ( 2.063896406836605024, 138.5688025270884793, -43.61045647697548588 ) ) ;
#18914 = ORIENTED_EDGE ( 'NONE', *, *, #19884, .F. ) ;
#18915 = ORIENTED_EDGE ( 'NONE', *, *, #24348, .F. ) ;
#18916 = EDGE_LOOP ( 'NONE', ( #23835, #28370, #23853, #26872 ) ) ;
#18917 = B_SPLINE_CURVE_WITH_KNOTS ( 'NONE', 3,
 ( #25097, #5363, #21039, #14129, #18749, #1328 ),
 .UNSPECIFIED., .F., .F.,
 ( 4, 2, 4 ),
 ( 0.000000000000000000, 0.0004335151646191511953, 0.0008670303292383023906 ),
 .UNSPECIFIED. ) ;
#18918 = VECTOR ( 'NONE', #25289, 999.9999999999998863 ) ;
#18919 = ADVANCED_FACE ( 'NONE', ( #7519 ), #22670, .F. ) ;
#18920 = AXIS2_PLACEMENT_3D ( 'NONE', #7731, #943, #22551 ) ;
#18921 = CARTESIAN_POINT ( 'NONE',  ( 7.762687761849954095E-17, 6.048924312129458720E-15, -44.74884827092600403 ) ) ;
#18922 = CARTESIAN_POINT ( 'NONE',  ( 25.64681081121879203, 107.5125461021402486, 34.49579773461821475 ) ) ;
#18923 = EDGE_CURVE ( 'NONE', #20933, #25194, #18228, .T. ) ;
#18924 = CARTESIAN_POINT ( 'NONE',  ( -1.044556982611271279, -1.643392503293034768, -45.76404732357878657 ) ) ;
#18925 = CARTESIAN_POINT ( 'NONE',  ( 2.433796855181233454, 60.50726454507903895, 132.3327394885233446 ) ) ;
#18926 = CARTESIAN_POINT ( 'NONE',  ( 2.063896406836605024, 86.47093297169155335, -116.7302989755729072 ) ) ;
#18927 = CARTESIAN_POINT ( 'NONE',  ( 1.833485406944043827, -85.72460230293772554, 117.0814567582541201 ) ) ;
#18928 = CARTESIAN_POINT ( 'NONE',  ( 25.64681081121879203, 56.81519825470756047, 97.57530875170624540 ) ) ;
#18929 = CARTESIAN_POINT ( 'NONE',  ( -23.79248802219722592, -7.157555990716680583, 32.40806545715339126 ) ) ;
#18930 = ORIENTED_EDGE ( 'NONE', *, *, #2247, .T. ) ;
#18931 = EDGE_LOOP ( 'NONE', ( #3244, #13062, #14869, #26715 ) ) ;
#18932 = CARTESIAN_POINT ( 'NONE',  ( 2.108393763691210676, -28.95405853987412570, -142.3786741588522773 ) ) ;
#18934 = CARTESIAN_POINT ( 'NONE',  ( 55.79472521941428198, -15.83764557006218610, -71.00924468211174201 ) ) ;
#18933 = CARTESIAN_POINT ( 'NONE',  ( 25.64699802086724389, 112.9109702078780373, -0.2377811728601773311 ) ) ;
#18935 = CARTESIAN_POINT ( 'NONE',  ( 28.37603512858459709, -37.15644006762142482, -108.5491486026795087 ) ) ;
#18936 = CARTESIAN_POINT ( 'NONE',  ( -20.21097721650786738, 8.835581399095163491, -28.26295598655176633 ) ) ;
#18937 = CARTESIAN_POINT ( 'NONE',  ( 25.64681081121879203, 91.10197563707947666, 66.70335573067896462 ) ) ;
#18938 = ORIENTED_EDGE ( 'NONE', *, *, #20837, .F. ) ;
#18939 = FACE_OUTER_BOUND ( 'NONE', #3255, .T. ) ;
#18940 = CARTESIAN_POINT ( 'NONE',  ( 10.93730112725990011, -128.3908183996585990, -79.81734490846054086 ) ) ;
#18941 = CARTESIAN_POINT ( 'NONE',  ( 10.93730112725972958, -84.82621002473526062, 125.1380233598475229 ) ) ;
#18942 = ORIENTED_EDGE ( 'NONE', *, *, #5260, .T. ) ;
#18943 = ORIENTED_EDGE ( 'NONE', *, *, #9347, .T. ) ;
#18944 = CARTESIAN_POINT ( 'NONE',  ( -1.155031165708884755, -38.31525684316158475, -25.28071330859873100 ) ) ;
#18945 = VERTEX_POINT ( 'NONE', #5336 ) ;
#18946 = CONICAL_SURFACE ( 'NONE', #21242, 117.6351876552689504, 0.9945805576725580410 ) ;
#18947 = ORIENTED_EDGE ( 'NONE', *, *, #16511, .T. ) ;
#18948 = CARTESIAN_POINT ( 'NONE',  ( 28.43349137099831836, 98.08682467580888442, -76.27296957774029806 ) ) ;
#18949 = ORIENTED_EDGE ( 'NONE', *, *, #16475, .T. ) ;
#18950 = CARTESIAN_POINT ( 'NONE',  ( -25.21435515916043713, 30.48034229288662544, 16.39063784838709736 ) ) ;
#18951 = CARTESIAN_POINT ( 'NONE',  ( 25.81918753295377655, 112.5005889664128631, 10.88546493098895063 ) ) ;
#18952 = EDGE_CURVE ( 'NONE', #21175, #14322, #14112, .T. ) ;
#18953 = CARTESIAN_POINT ( 'NONE',  ( -55.25297051322618813, 0.001818774723749727032, -0.01483298743815054943 ) ) ;
#18954 = EDGE_CURVE ( 'NONE', #20493, #9181, #12488, .T. ) ;
#18955 = CARTESIAN_POINT ( 'NONE',  ( -55.24728320129491266, 0.009072670231975488858, 0.01137345571546827770 ) ) ;
#18956 = CARTESIAN_POINT ( 'NONE',  ( -8.786685647604898008, 48.22796981442802178, 23.24040270374343464 ) ) ;
#18957 = DIRECTION ( 'NONE',  ( 0.7637818620346800147, 0.3965875333584841234, -0.5092696688508654423 ) ) ;
#18958 = CARTESIAN_POINT ( 'NONE',  ( -22.23226125620943705, 20.31044300692207472, 24.24619897613454000 ) ) ;
#18959 = EDGE_CURVE ( 'NONE', #24758, #7039, #13447, .T. ) ;
#18960 = VERTEX_POINT ( 'NONE', #14684 ) ;
#18961 = VECTOR ( 'NONE', #17489, 1000.000000000000341 ) ;
#18962 = CARTESIAN_POINT ( 'NONE',  ( -1.619063947482197729, 46.30105812165548684, -2.489035965910316506 ) ) ;
#18963 = CARTESIAN_POINT ( 'NONE',  ( 21.16825799904932381, 103.5479404090032602, 87.29264348877838131 ) ) ;
#18964 = CARTESIAN_POINT ( 'NONE',  ( 26.11404676487257603, -102.9690087468798509, -47.08215554553621729 ) ) ;
#18965 = EDGE_LOOP ( 'NONE', ( #3319, #7354, #2350, #17655 ) ) ;
#18966 = VECTOR ( 'NONE', #4397, 1000.000000000000000 ) ;
#18967 = ORIENTED_EDGE ( 'NONE', *, *, #16963, .F. ) ;
#18968 = EDGE_LOOP ( 'NONE', ( #13796, #13215, #6975, #19513 ) ) ;
#18969 = CARTESIAN_POINT ( 'NONE',  ( -55.24271866751342941, -0.004365563123939053720, 0.008433070970613821063 ) ) ;
#18970 = DIRECTION ( 'NONE',  ( -1.000000000000000000, -0.000000000000000000, -0.000000000000000000 ) ) ;
#18972 = CARTESIAN_POINT ( 'NONE',  ( 109.1592201516379674, 0.007376275279032895593, -0.002720803050370492436 ) ) ;
#18971 = CARTESIAN_POINT ( 'NONE',  ( 109.1721716018069657, 0.01616973485710950648, -0.005466227998629047229 ) ) ;
#18973 = CARTESIAN_POINT ( 'NONE',  ( -20.57838717382308147, 27.96569011373101077, 10.78122205916971055 ) ) ;
#18974 = CARTESIAN_POINT ( 'NONE',  ( -1.539763995773685057, -11.93465967526326921, -44.72359274866478529 ) ) ;
#18975 = ORIENTED_EDGE ( 'NONE', *, *, #23530, .F. ) ;
#18976 = CARTESIAN_POINT ( 'NONE',  ( -1.058197053496158890, 12.47644286888577270, 44.07533330186774378 ) ) ;
#18977 = CARTESIAN_POINT ( 'NONE',  ( -1.463510566862838091, -44.64091840826481672, 11.94877850058549029 ) ) ;
#18978 = ORIENTED_EDGE ( 'NONE', *, *, #28212, .F. ) ;
#18979 = CARTESIAN_POINT ( 'NONE',  ( 10.93730112725990189, -140.0398180619108075, -56.95489579269887059 ) ) ;
#18980 = CARTESIAN_POINT ( 'NONE',  ( -20.47566338032508426, 1.586617869344308041, 29.82700953060495408 ) ) ;
#18981 = FACE_OUTER_BOUND ( 'NONE', #9736, .T. ) ;
#18982 = CARTESIAN_POINT ( 'NONE',  ( 1.832998868059858122, 117.0819875546706896, -85.72499093307983742 ) ) ;
#18983 = CARTESIAN_POINT ( 'NONE',  ( 25.64700659047696263, 107.3144208978484926, 35.10784848926700619 ) ) ;
#18984 = CARTESIAN_POINT ( 'NONE',  ( -21.81686047589426281, -18.24499610240063419, -33.92779429964196680 ) ) ;
#18985 = CARTESIAN_POINT ( 'NONE',  ( -9.156249394959706578, 8.027840202793937507, -53.90509764945131366 ) ) ;
#18986 = ORIENTED_EDGE ( 'NONE', *, *, #9105, .F. ) ;
#18987 = LINE ( 'NONE', #8472, #15799 ) ;
#18988 = ADVANCED_FACE ( 'NONE', ( #21588 ), #14827, .T. ) ;
#18989 = CARTESIAN_POINT ( 'NONE',  ( 9.884929003653626367, -42.50195158091132441, 144.4113244745770146 ) ) ;
#18990 = CARTESIAN_POINT ( 'NONE',  ( 32.73300124599739291, 105.8473486001057466, -51.32617430724801721 ) ) ;
#18991 = ORIENTED_EDGE ( 'NONE', *, *, #12383, .F. ) ;
#18992 = CARTESIAN_POINT ( 'NONE',  ( -55.24728320129491266, 0.01453410071985307417, -0.0006547948648738343260 ) ) ;
#18993 = ORIENTED_EDGE ( 'NONE', *, *, #7940, .F. ) ;
#18994 = CIRCLE ( 'NONE', #17585, 12.50000000000000178 ) ;
#18995 = ADVANCED_FACE ( 'NONE', ( #18871 ), #27433, .F. ) ;
#18996 = CARTESIAN_POINT ( 'NONE',  ( -1.619063947482197729, -16.67502769180532596, 43.26576862488450104 ) ) ;
#18997 = CARTESIAN_POINT ( 'NONE',  ( 1.893872463202066259, 73.39855082356820049, -125.2243573918626964 ) ) ;
#18998 = EDGE_CURVE ( 'NONE', #17409, #6523, #15115, .T. ) ;
#18999 = CARTESIAN_POINT ( 'NONE',  ( -23.79248802219730052, -13.25839849636379597, -30.42578156345381046 ) ) ;
#19000 = CARTESIAN_POINT ( 'NONE',  ( 8.186469777910561518, 131.0413692044509162, 71.65198614410246591 ) ) ;
#19001 = CARTESIAN_POINT ( 'NONE',  ( -55.25297051322618813, 0.01019003092403517226, 0.01093108995494820879 ) ) ;
#19002 = CARTESIAN_POINT ( 'NONE',  ( 1.833603222531972721, 141.8454679205787272, 30.60504697399260721 ) ) ;
#19003 = DIRECTION ( 'NONE',  ( -0.5946245182733606027, -0.7992853357633878941, 0.08697490616138658925 ) ) ;
#19004 = FACE_OUTER_BOUND ( 'NONE', #25685, .T. ) ;
#19005 = CARTESIAN_POINT ( 'NONE',  ( -28.13707043255157103, 18.06394523322453693, -14.07296284901339334 ) ) ;
#19006 = ORIENTED_EDGE ( 'NONE', *, *, #25532, .F. ) ;
#19007 = ORIENTED_EDGE ( 'NONE', *, *, #22711, .F. ) ;
#19008 = CARTESIAN_POINT ( 'NONE',  ( -1.045287976400365970, -43.05558670614224326, 15.59869763335140469 ) ) ;
#19009 = CARTESIAN_POINT ( 'NONE',  ( -25.21435515916025594, 1.749597353048488237E-16, -4.373993382621220594E-17 ) ) ;
#19010 = CARTESIAN_POINT ( 'NONE',  ( 109.1592201516379674, -0.007780772729122749191, 0.001127733110588196924 ) ) ;
#19011 = CARTESIAN_POINT ( 'NONE',  ( 25.64704443564076897, -83.82001435192574945, -75.65149037849849378 ) ) ;
#19012 = CARTESIAN_POINT ( 'NONE',  ( 25.98552792386796995, -92.15963349013314598, -65.62435323276262977 ) ) ;
#19013 =( BOUNDED_SURFACE ( )  B_SPLINE_SURFACE ( 3, 1, ( 
 ( #11161, #17624 ),
 ( #22089, #26266 ),
 ( #17336, #15315 ),
 ( #19935, #13162 ) ),
 .UNSPECIFIED., .F., .F., .F. ) 
 B_SPLINE_SURFACE_WITH_KNOTS ( ( 4, 4 ),
 ( 2, 2 ),
 ( 0.000000000000000000, 1.000000000000000000 ),
 ( 0.000000000000000000, 1.000000000000000000 ),
 .UNSPECIFIED. ) 
 GEOMETRIC_REPRESENTATION_ITEM ( )  RATIONAL_B_SPLINE_SURFACE ( (
 ( 1.000000000000000000, 1.000000000000000000),
 ( 0.6386103224230316178, 0.9954351624131538845),
 ( 0.6386103224230316178, 0.9954351624131538845),
 ( 1.000000000000000000, 1.000000000000000000) ) ) 
 REPRESENTATION_ITEM ( '' )  SURFACE ( )  );
#19014 = CARTESIAN_POINT ( 'NONE',  ( 25.64699802086725455, -91.48665801621615401, -66.17503410043995871 ) ) ;
#19015 = VERTEX_POINT ( 'NONE', #28200 ) ;
#19016 = CARTESIAN_POINT ( 'NONE',  ( 1.833838850855438407, -144.3241377520101310, 15.07960613928581317 ) ) ;
#19017 = CARTESIAN_POINT ( 'NONE',  ( 2.430230287190592531, 142.0258656395025980, -31.67257033707364400 ) ) ;
#19018 = AXIS2_PLACEMENT_3D ( 'NONE', #2487, #4658, #13571 ) ;
#19019 = DIRECTION ( 'NONE',  ( 0.000000000000000000, 0.000000000000000000, 1.000000000000000000 ) ) ;
#19020 = CARTESIAN_POINT ( 'NONE',  ( -1.045287976400365970, -36.12803364096568259, 28.14015102489869591 ) ) ;
#19021 = FACE_OUTER_BOUND ( 'NONE', #20422, .T. ) ;
#19022 = ORIENTED_EDGE ( 'NONE', *, *, #1982, .T. ) ;
#19023 = CARTESIAN_POINT ( 'NONE',  ( -1.619063947482201282, 16.67502769180561728, -43.26576862488438735 ) ) ;
#19024 = B_SPLINE_CURVE_WITH_KNOTS ( 'NONE', 3,
 ( #15516, #136, #6629, #21880, #24627, #15238, #2137, #415 ),
 .UNSPECIFIED., .F., .F.,
 ( 4, 2, 2, 4 ),
 ( 0.000000000000000000, 0.002761524886576667125, 0.005523049773153334251, 0.01104609954630666677 ),
 .UNSPECIFIED. ) ;
#19025 = FACE_OUTER_BOUND ( 'NONE', #14224, .T. ) ;
#19026 = EDGE_LOOP ( 'NONE', ( #11909, #28339, #9202, #9651 ) ) ;
#19027 = ORIENTED_EDGE ( 'NONE', *, *, #17631, .T. ) ;
#19028 = ADVANCED_FACE ( 'NONE', ( #3753 ), #21558, .F. ) ;
#19029 = ORIENTED_EDGE ( 'NONE', *, *, #4600, .F. ) ;
#19030 = ADVANCED_FACE ( 'NONE', ( #27644 ), #20795, .F. ) ;
#19031 = EDGE_CURVE ( 'NONE', #9431, #1130, #20998, .T. ) ;
#19032 = CARTESIAN_POINT ( 'NONE',  ( 25.64681081121879203, 91.10197563708035773, -66.70335573067774249 ) ) ;
#19033 = FACE_OUTER_BOUND ( 'NONE', #5313, .T. ) ;
#19034 = CARTESIAN_POINT ( 'NONE',  ( 26.11404676487257603, 22.43340081644767636, 110.9778746459747794 ) ) ;
#19035 = CARTESIAN_POINT ( 'NONE',  ( 26.11404676487257603, 110.9778746459746941, 22.43340081644806006 ) ) ;
#19036 = B_SPLINE_CURVE_WITH_KNOTS ( 'NONE', 3,
 ( #14232, #25350, #14389, #19692, #8919, #9481 ),
 .UNSPECIFIED., .F., .F.,
 ( 4, 2, 4 ),
 ( 4.336808689942017255E-19, 0.0006311571484586044880, 0.001262314296917208542 ),
 .UNSPECIFIED. ) ;
#19037 = CARTESIAN_POINT ( 'NONE',  ( 2.263178113027050742, -132.2496129425956042, -60.41552743271091686 ) ) ;
#19038 = CARTESIAN_POINT ( 'NONE',  ( -1.619063947482197729, 2.489035965910801895, 46.30105812165545842 ) ) ;
#19039 = CARTESIAN_POINT ( 'NONE',  ( -22.23226125620944416, 24.24619897613477093, -20.31044300692182603 ) ) ;
#19040 = CARTESIAN_POINT ( 'NONE',  ( 1.833485406944057594, -59.50871042846138437, -132.3460930279897241 ) ) ;
#19041 = CARTESIAN_POINT ( 'NONE',  ( 1.832998868059890096, 72.09222286251259959, -125.9352106559976363 ) ) ;
#19042 = CARTESIAN_POINT ( 'NONE',  ( 1.833485406944057594, -142.0485807715644171, -29.64752363041688454 ) ) ;
#19043 =( BOUNDED_SURFACE ( )  B_SPLINE_SURFACE ( 3, 1, ( 
 ( #1272, #16837 ),
 ( #3153, #18696 ),
 ( #10073, #27605 ),
 ( #22753, #16535 ) ),
 .UNSPECIFIED., .F., .F., .F. ) 
 B_SPLINE_SURFACE_WITH_KNOTS ( ( 4, 4 ),
 ( 2, 2 ),
 ( 0.000000000000000000, 1.000000000000000000 ),
 ( 0.000000000000000000, 1.000000000000000000 ),
 .UNSPECIFIED. ) 
 GEOMETRIC_REPRESENTATION_ITEM ( )  RATIONAL_B_SPLINE_SURFACE ( (
 ( 1.000000000000000000, 1.000000000000000000),
 ( 0.6386103224230316178, 0.9954351624131538845),
 ( 0.6386103224230316178, 0.9954351624131538845),
 ( 1.000000000000000000, 1.000000000000000000) ) ) 
 REPRESENTATION_ITEM ( '' )  SURFACE ( )  );
#19044 = CARTESIAN_POINT ( 'NONE',  ( -1.031422197589716205, -36.13727897780108123, 28.14735071801782951 ) ) ;
#19045 = CARTESIAN_POINT ( 'NONE',  ( 10.93730112725943471, 125.1380233598475229, 84.82621002473483429 ) ) ;
#19047 = CARTESIAN_POINT ( 'NONE',  ( 109.1592201516379674, 0.002134489919774364575, 0.007566779963318560377 ) ) ;
#19046 = CARTESIAN_POINT ( 'NONE',  ( 25.65782528836479770, 112.2379831684172302, 12.37768345530014358 ) ) ;
#19048 = CARTESIAN_POINT ( 'NONE',  ( 10.93730112726006354, 148.8212007290666747, -26.59437931460595905 ) ) ;
#19049 = DIRECTION ( 'NONE',  ( 0.000000000000000000, 0.000000000000000000, 1.000000000000000000 ) ) ;
#19050 = CARTESIAN_POINT ( 'NONE',  ( -55.24728320129491266, -0.008013189884951492717, -0.01214321324517155139 ) ) ;
#19051 = ORIENTED_EDGE ( 'NONE', *, *, #16402, .F. ) ;
#19052 = ADVANCED_FACE ( 'NONE', ( #12380 ), #23607, .F. ) ;
#19053 = ORIENTED_EDGE ( 'NONE', *, *, #3742, .T. ) ;
#19054 = CARTESIAN_POINT ( 'NONE',  ( -20.37983603106073716, 23.16947629293390065, 18.69865230096500852 ) ) ;
#19056 = ORIENTED_EDGE ( 'NONE', *, *, #16584, .T. ) ;
#19055 = CARTESIAN_POINT ( 'NONE',  ( -1.048996300304505747, 27.53442103413745912, 36.59642367107714023 ) ) ;
#19057 = ORIENTED_EDGE ( 'NONE', *, *, #16906, .T. ) ;
#19058 = ADVANCED_FACE ( 'NONE', ( #27798 ), #25621, .F. ) ;
#19059 = ORIENTED_EDGE ( 'NONE', *, *, #15000, .F. ) ;
#19060 = ORIENTED_EDGE ( 'NONE', *, *, #17792, .F. ) ;
#19061 = ADVANCED_FACE ( 'NONE', ( #8927 ), #4985, .F. ) ;
#19062 = ADVANCED_FACE ( 'NONE', ( #4734 ), #26264, .T. ) ;
#19063 = CARTESIAN_POINT ( 'NONE',  ( 5.340103579038266268, -120.6284720963480339, -84.79482754232395791 ) ) ;
#19064 = B_SPLINE_CURVE_WITH_KNOTS ( 'NONE', 3,
 ( #18575, #14233, #22770, #3316, #25351, #5624, #579, #23200 ),
 .UNSPECIFIED., .F., .F.,
 ( 4, 2, 2, 4 ),
 ( 6.938893903907228378E-18, 0.0002429592666046844580, 0.0004859185332093619771, 0.0009718370664186995597 ),
 .UNSPECIFIED. ) ;
#19065 = CARTESIAN_POINT ( 'NONE',  ( 1.833691583653522361, -142.0122737882510080, 29.82175144858052462 ) ) ;
#19066 = CARTESIAN_POINT ( 'NONE',  ( -1.056502255334265339, -27.33667001641142846, 36.75727364034761990 ) ) ;
#19067 = CARTESIAN_POINT ( 'NONE',  ( -20.20612092514784663, 1.137292630518469849, 29.57813644637188233 ) ) ;
#19068 = DIRECTION ( 'NONE',  ( 0.000000000000000000, 0.000000000000000000, -1.000000000000000000 ) ) ;
#19069 = CYLINDRICAL_SURFACE ( 'NONE', #25390, 20.00000000000000000 ) ;
#19070 = DIRECTION ( 'NONE',  ( -1.000000000000000000, -0.000000000000000000, -0.000000000000000000 ) ) ;
#19071 = CARTESIAN_POINT ( 'NONE',  ( -4.780792508754321268, -45.80716263181250980, -18.84172549606854119 ) ) ;
#19072 = ORIENTED_EDGE ( 'NONE', *, *, #19618, .T. ) ;
#19073 = ORIENTED_EDGE ( 'NONE', *, *, #17408, .T. ) ;
#19074 = CARTESIAN_POINT ( 'NONE',  ( 25.64681081121879203, -107.5125461021400355, -34.49579773461893950 ) ) ;
#19075 = CARTESIAN_POINT ( 'NONE',  ( 2.108393763691206235, 133.2474712570801785, -57.92353377304154094 ) ) ;
#19076 = CARTESIAN_POINT ( 'NONE',  ( 25.87036335909429852, 22.53739730344198833, -110.7910326764399542 ) ) ;
#19077 = DIRECTION ( 'NONE',  ( 0.7563875759206388771, 0.3556158456312978888, 0.5490129373055215867 ) ) ;
#19078 = DIRECTION ( 'NONE',  ( 1.000000000000000000, -6.938893903907226837E-18, 1.734723475976806709E-18 ) ) ;
#19079 = VERTEX_POINT ( 'NONE', #13507 ) ;
#19080 = CARTESIAN_POINT ( 'NONE',  ( -28.13707043255157103, -18.06394523322443035, 14.07296284901352479 ) ) ;
#19081 = ADVANCED_FACE ( 'NONE', ( #22154 ), #20626, .F. ) ;
#19082 = CARTESIAN_POINT ( 'NONE',  ( -28.41354790283022069, 22.41474081378008876, 5.969609727607788408 ) ) ;
#19083 = CARTESIAN_POINT ( 'NONE',  ( 1.833838850855474822, -15.25659494068204580, 144.3055354793886806 ) ) ;
#19084 = ORIENTED_EDGE ( 'NONE', *, *, #25056, .T. ) ;
#19085 = ORIENTED_EDGE ( 'NONE', *, *, #2628, .T. ) ;
#19086 = EDGE_CURVE ( 'NONE', #7528, #7658, #18466, .T. ) ;
#19087 = CARTESIAN_POINT ( 'NONE',  ( -1.044556982611274387, -37.98985389331830476, -25.56989963842190150 ) ) ;
#19088 = EDGE_LOOP ( 'NONE', ( #21891, #519, #8015, #24636 ) ) ;
#19089 = VERTEX_POINT ( 'NONE', #15509 ) ;
#19090 = EDGE_CURVE ( 'NONE', #7787, #15835, #6583, .T. ) ;
#19091 = ORIENTED_EDGE ( 'NONE', *, *, #5128, .T. ) ;
#19092 = CARTESIAN_POINT ( 'NONE',  ( 109.1592201516379674, 0.005631912476305695608, 0.005485778713193766379 ) ) ;
#19093 = ORIENTED_EDGE ( 'NONE', *, *, #7756, .F. ) ;
#19094 = CARTESIAN_POINT ( 'NONE',  ( -20.57838717382308147, 7.715628353033680220, -28.96176188950220975 ) ) ;
#19095 = FACE_OUTER_BOUND ( 'NONE', #13752, .T. ) ;
#19096 = CONTEXT_DEPENDENT_SHAPE_REPRESENTATION ( #13028, #2810 ) ;
#19097 = CARTESIAN_POINT ( 'NONE',  ( -1.155031165708891860, -44.25214473648919977, -12.20332162035446366 ) ) ;
#19098 = CARTESIAN_POINT ( 'NONE',  ( -7.078251931573406708, -38.93060825814203696, 34.59014398252958244 ) ) ;
#19099 = CARTESIAN_POINT ( 'NONE',  ( 26.11404676487257603, 112.7148551500680469, 10.71016160607605627 ) ) ;
#19100 = CARTESIAN_POINT ( 'NONE',  ( 1.833485406944043827, 0.5339064996905048543, -145.1085452359073145 ) ) ;
#19101 = CARTESIAN_POINT ( 'NONE',  ( -20.57838717382308147, 29.92853265176831812, 1.611677988432465014 ) ) ;
#19102 = ORIENTED_EDGE ( 'NONE', *, *, #20311, .T. ) ;
#19103 = CARTESIAN_POINT ( 'NONE',  ( 30.58324630866341565, -3.944468862006814458, -120.8793175557613893 ) ) ;
#19105 = CARTESIAN_POINT ( 'NONE',  ( -1.155031165708893415, -45.85732438018708024, 2.068616213631418344 ) ) ;
#19104 = DIRECTION ( 'NONE',  ( 0.7563875759206388771, 0.4122509917856751471, -0.5078650950445667833 ) ) ;
#19106 = CARTESIAN_POINT ( 'NONE',  ( -20.20700224038492721, 24.51628800869048419, -16.58740185276719359 ) ) ;
#19107 = ORIENTED_EDGE ( 'NONE', *, *, #26088, .F. ) ;
#19108 = EDGE_LOOP ( 'NONE', ( #16028, #1741, #3113, #25715 ) ) ;
#19109 = CARTESIAN_POINT ( 'NONE',  ( -25.21435515916043357, 6.169479169075458458, -34.05351380035335751 ) ) ;
#19110 = B_SPLINE_CURVE_WITH_KNOTS ( 'NONE', 3,
 ( #5175, #2436, #20001, #24775, #15671, #20285, #13804, #13950 ),
 .UNSPECIFIED., .F., .F.,
 ( 4, 2, 2, 4 ),
 ( 6.938893903907228378E-18, 0.0002429592666046851085, 0.0004859185332093632782, 0.0009718370664186818872 ),
 .UNSPECIFIED. ) ;
#19111 = CARTESIAN_POINT ( 'NONE',  ( -21.81686047589428057, -26.62923599424948407, 27.83628745321478704 ) ) ;
#19112 = CARTESIAN_POINT ( 'NONE',  ( 109.1592201516379674, -0.007051465909551689858, -0.003476928926125464302 ) ) ;
#19113 = B_SPLINE_CURVE_WITH_KNOTS ( 'NONE', 3,
 ( #27624, #27780, #25496, #9948, #1285, #3451, #12096, #12365, #14667, #5465 ),
 .UNSPECIFIED., .F., .F.,
 ( 4, 3, 3, 4 ),
 ( 1.040834085586084257E-17, 0.0002669560319015703035, 0.0005492286108966372253, 0.0008315040496093471746 ),
 .UNSPECIFIED. ) ;
#19114 = CARTESIAN_POINT ( 'NONE',  ( 2.263178607246643104, 133.3897506477022148, 57.85473702627159298 ) ) ;
#19115 = CARTESIAN_POINT ( 'NONE',  ( 21.16825799904909289, -9.757279788663675291, 135.0813719997368878 ) ) ;
#19116 = ORIENTED_EDGE ( 'NONE', *, *, #2619, .T. ) ;
#19117 = CARTESIAN_POINT ( 'NONE',  ( 2.433796855181205476, 71.49415740225076377, 126.7346379669258312 ) ) ;
#19118 = CARTESIAN_POINT ( 'NONE',  ( -1.113548883309563253, -44.18588492042580640, 12.28732181966563886 ) ) ;
#19119 = EDGE_LOOP ( 'NONE', ( #18530, #23134, #11959, #25338 ) ) ;
#19120 = LINE ( 'NONE', #27759, #4675 ) ;
#19121 = CARTESIAN_POINT ( 'NONE',  ( 109.1586900883932856, -0.006479576224398268976, 0.002995460350188374095 ) ) ;
#19122 = CARTESIAN_POINT ( 'NONE',  ( 109.1587776205901861, 0.005502145856762305151, 0.004842060007769406239 ) ) ;
#19123 = FACE_OUTER_BOUND ( 'NONE', #20123, .T. ) ;
#19124 = CARTESIAN_POINT ( 'NONE',  ( 26.11404676487259024, -55.62948129436313849, 98.61392875273344316 ) ) ;
#19125 = EDGE_CURVE ( 'NONE', #22997, #771, #15855, .T. ) ;
#19126 = ORIENTED_EDGE ( 'NONE', *, *, #17053, .T. ) ;
#19127 = CARTESIAN_POINT ( 'NONE',  ( 109.1721716018069657, -0.01616973485710946484, 0.005466227998629163455 ) ) ;
#19128 = ADVANCED_FACE ( 'NONE', ( #13089 ), #1877, .F. ) ;
#19129 = B_SPLINE_CURVE_WITH_KNOTS ( 'NONE', 3,
 ( #14654, #3577, #12358, #25891, #10228, #12496, #18990 ),
 .UNSPECIFIED., .F., .F.,
 ( 4, 3, 4 ),
 ( 6.687668363004596812E-16, 0.02816610861753246139, 0.04000277880656288865 ),
 .UNSPECIFIED. ) ;
#19130 = CARTESIAN_POINT ( 'NONE',  ( 109.1721716018069657, -0.001984900887706511109, -0.01695288006057378907 ) ) ;
#19131 = EDGE_CURVE ( 'NONE', #654, #16962, #24426, .T. ) ;
#19132 = ORIENTED_EDGE ( 'NONE', *, *, #21445, .T. ) ;
#19133 = CARTESIAN_POINT ( 'NONE',  ( 2.433796855181219243, -28.83182736670634583, 142.6247129145647534 ) ) ;
#19134 = CARTESIAN_POINT ( 'NONE',  ( 1.894214914920939075, -116.8658096527528443, 86.08679174688037961 ) ) ;
#19135 = B_SPLINE_CURVE_WITH_KNOTS ( 'NONE', 3,
 ( #10694, #6105, #14708, #19459 ),
 .UNSPECIFIED., .F., .F.,
 ( 4, 4 ),
 ( 3.469446951953614189E-18, 0.008383560773332719013 ),
 .UNSPECIFIED. ) ;
#19136 = CARTESIAN_POINT ( 'NONE',  ( 26.04756280548352265, -102.9366382251196228, 47.04636360340792578 ) ) ;
#19137 = CARTESIAN_POINT ( 'NONE',  ( -1.056502255334265339, -0.5104472526216820016, 45.80535052436398047 ) ) ;
#19138 = LINE ( 'NONE', #1574, #17611 ) ;
#19139 = CARTESIAN_POINT ( 'NONE',  ( 26.28373643307405771, 60.14387450369989097, -112.4918671811453663 ) ) ;
#19140 = CARTESIAN_POINT ( 'NONE',  ( 8.186469829614221538, 42.84118568057207455, 143.0750865143068040 ) ) ;
#19141 = CARTESIAN_POINT ( 'NONE',  ( 55.79472521941428198, 21.78881894124796403, -69.41463258328491293 ) ) ;
#19142 = CARTESIAN_POINT ( 'NONE',  ( 25.64692232868533139, 112.2580042965358871, -12.12735788170695805 ) ) ;
#19143 = CARTESIAN_POINT ( 'NONE',  ( 2.108985857320902824, -57.92316197981750747, 133.2480631238191791 ) ) ;
#19144 = VERTEX_POINT ( 'NONE', #7630 ) ;
#19145 = ORIENTED_EDGE ( 'NONE', *, *, #25609, .T. ) ;
#19146 = CARTESIAN_POINT ( 'NONE',  ( -22.34422965417122953, 37.30738373203627845, 6.759368364653937533 ) ) ;
#19147 = FACE_OUTER_BOUND ( 'NONE', #13102, .T. ) ;
#19148 = CARTESIAN_POINT ( 'NONE',  ( 109.1589550718174877, -0.006445391216542599791, -0.003980125429499862914 ) ) ;
#19149 = CARTESIAN_POINT ( 'NONE',  ( 28.37603512858447985, -104.0705994281840105, 48.29936889363920471 ) ) ;
#19150 = CARTESIAN_POINT ( 'NONE',  ( 32.73300124599732186, 0.000000000000000000, 0.000000000000000000 ) ) ;
#19151 = CARTESIAN_POINT ( 'NONE',  ( 109.1586900883932856, 0.006561743627145262027, 0.002810909342002427570 ) ) ;
#19152 = CARTESIAN_POINT ( 'NONE',  ( 55.79472521941426777, 66.16469064668298472, 30.25520714117929444 ) ) ;
#19153 = ORIENTED_EDGE ( 'NONE', *, *, #10196, .F. ) ;
#19154 = DIRECTION ( 'NONE',  ( 0.000000000000000000, 0.000000000000000000, 1.000000000000000000 ) ) ;
#19155 = CARTESIAN_POINT ( 'NONE',  ( -1.019300379054419725, 28.53917295602949977, 35.83762006677368106 ) ) ;
#19156 = CARTESIAN_POINT ( 'NONE',  ( -1.058197053496162887, -25.48582931365496762, -38.06270006878843759 ) ) ;
#19157 = EDGE_CURVE ( 'NONE', #6911, #9397, #1765, .T. ) ;
#19158 = LINE ( 'NONE', #3606, #9828 ) ;
#19159 = ORIENTED_EDGE ( 'NONE', *, *, #26567, .T. ) ;
#19160 = CARTESIAN_POINT ( 'NONE',  ( 25.64692872815577473, -112.2585610031152328, -12.12228186621173975 ) ) ;
#19161 = CARTESIAN_POINT ( 'NONE',  ( 26.11404676487259024, -97.48350837663652158, 57.58742681967414256 ) ) ;
#19162 = VERTEX_POINT ( 'NONE', #25320 ) ;
#19163 = VERTEX_POINT ( 'NONE', #23027 ) ;
#19164 = ORIENTED_EDGE ( 'NONE', *, *, #6974, .F. ) ;
#19165 = B_SPLINE_CURVE_WITH_KNOTS ( 'NONE', 3,
 ( #21092, #1378, #8034, #23421, #16802, #25579, #5858, #14619, #13299, #73 ),
 .UNSPECIFIED., .F., .F.,
 ( 4, 3, 3, 4 ),
 ( 3.925231146709437917E-17, 0.0002669559177086215868, 0.0005339118354151091385, 0.001067817517169165117 ),
 .UNSPECIFIED. ) ;
#19166 = B_SPLINE_CURVE_WITH_KNOTS ( 'NONE', 3,
 ( #25918, #14680, #10389, #21307 ),
 .UNSPECIFIED., .F., .F.,
 ( 4, 4 ),
 ( 1.977889076651310254E-16, 0.001982023823822937677 ),
 .UNSPECIFIED. ) ;
#19167 = CARTESIAN_POINT ( 'NONE',  ( 10.93730112725994275, -36.23586118136433498, -146.7718404940647190 ) ) ;
#19168 = CARTESIAN_POINT ( 'NONE',  ( -9.156249394959706578, 24.29252099376491358, -48.78605533024748553 ) ) ;
#19169 =( BOUNDED_SURFACE ( )  B_SPLINE_SURFACE ( 3, 1, ( 
 ( #2376, #21550 ),
 ( #17090, #24015 ),
 ( #4269, #13317 ),
 ( #21972, #8887 ) ),
 .UNSPECIFIED., .F., .F., .F. ) 
 B_SPLINE_SURFACE_WITH_KNOTS ( ( 4, 4 ),
 ( 2, 2 ),
 ( 0.000000000000000000, 1.000000000000000000 ),
 ( 0.000000000000000000, 1.000000000000000000 ),
 .UNSPECIFIED. ) 
 GEOMETRIC_REPRESENTATION_ITEM ( )  RATIONAL_B_SPLINE_SURFACE ( (
 ( 1.000000000000000000, 1.000000000000000000),
 ( 0.9956975270656954757, 0.8568959468854893125),
 ( 0.9956975270656954757, 0.8568959468854893125),
 ( 1.000000000000000000, 1.000000000000000000) ) ) 
 REPRESENTATION_ITEM ( '' )  SURFACE ( )  );
#19170 = CARTESIAN_POINT ( 'NONE',  ( -21.81686047589429123, 26.62923599424970433, -27.83628745321458453 ) ) ;
#19171 = VERTEX_POINT ( 'NONE', #2863 ) ;
#19172 = CARTESIAN_POINT ( 'NONE',  ( -1.031422197589711987, 36.13727897780127307, -28.14735071801756661 ) ) ;
#19173 = CARTESIAN_POINT ( 'NONE',  ( 1.833809397773902283, 59.18399778167309933, -132.4918864201821407 ) ) ;
#19175 = B_SPLINE_CURVE_WITH_KNOTS ( 'NONE', 3,
 ( #26229, #24093, #4356, #7246 ),
 .UNSPECIFIED., .F., .F.,
 ( 4, 4 ),
 ( 3.503851573261294794E-16, 0.01077107486149824281 ),
 .UNSPECIFIED. ) ;
#19174 = CARTESIAN_POINT ( 'NONE',  ( -20.57838717382308147, 1.611677988432778319, 29.92853265176829325 ) ) ;
#19176 = CARTESIAN_POINT ( 'NONE',  ( -20.20700224038492010, 24.51628800869071867, 16.58740185276683832 ) ) ;
#19177 = EDGE_CURVE ( 'NONE', #25165, #4432, #5200, .T. ) ;
#19178 = CARTESIAN_POINT ( 'NONE',  ( -20.90916690077959927, 17.17795951644708907, 35.64494649500667833 ) ) ;
#19179 = CARTESIAN_POINT ( 'NONE',  ( -8.786685647604889127, 9.545808661480615243, -52.67761315067287597 ) ) ;
#19180 = CARTESIAN_POINT ( 'NONE',  ( 1.833838850093440165, -141.9387673160884162, -30.17001281793505996 ) ) ;
#19181 = EDGE_CURVE ( 'NONE', #17575, #21619, #26147, .T. ) ;
#19182 = CARTESIAN_POINT ( 'NONE',  ( 2.063896406836605024, 73.79559738457928120, -125.1295119249431309 ) ) ;
#19183 = ADVANCED_FACE ( 'NONE', ( #24898 ), #27609, .F. ) ;
#19184 = CARTESIAN_POINT ( 'NONE',  ( 26.28373643307440233, 105.5888781856746732, 71.57300207276388448 ) ) ;
#19185 = DIRECTION ( 'NONE',  ( 0.000000000000000000, 0.000000000000000000, 1.000000000000000000 ) ) ;
#19186 = CARTESIAN_POINT ( 'NONE',  ( -6.574463467970654840, -25.96726214983158698, 44.27173031830760408 ) ) ;
#19187 = ORIENTED_EDGE ( 'NONE', *, *, #21359, .F. ) ;
#19188 = ORIENTED_EDGE ( 'NONE', *, *, #3510, .F. ) ;
#19189 = CARTESIAN_POINT ( 'NONE',  ( -1.259972190295298500, 38.49631882650683679, 25.19627397134255986 ) ) ;
#19190 = DIRECTION ( 'NONE',  ( -1.000000000000000000, -0.000000000000000000, -0.000000000000000000 ) ) ;
#19191 = ORIENTED_EDGE ( 'NONE', *, *, #28102, .F. ) ;
#19192 = ORIENTED_EDGE ( 'NONE', *, *, #3162, .F. ) ;
#19193 = ORIENTED_EDGE ( 'NONE', *, *, #27460, .T. ) ;
#19194 = B_SPLINE_CURVE_WITH_KNOTS ( 'NONE', 3,
 ( #19280, #1583, #27788, #23630, #14538, #16979, #10247, #28190 ),
 .UNSPECIFIED., .F., .F.,
 ( 4, 2, 2, 4 ),
 ( 0.000000000000000000, 0.0002429588503611307274, 0.0004859177007222614548, 0.0009718354014445039360 ),
 .UNSPECIFIED. ) ;
#19195 = CARTESIAN_POINT ( 'NONE',  ( 1.833485406944043827, 97.49333871408838093, -107.4794113447399297 ) ) ;
#19196 = CARTESIAN_POINT ( 'NONE',  ( 109.1586059443104944, 0.002447596125914170816, 0.006637156007970161815 ) ) ;
#19197 =( BOUNDED_SURFACE ( )  B_SPLINE_SURFACE ( 3, 1, ( 
 ( #3297, #28025 ),
 ( #5756, #10224 ),
 ( #14513, #23603 ),
 ( #3862, #18837 ) ),
 .UNSPECIFIED., .F., .F., .F. ) 
 B_SPLINE_SURFACE_WITH_KNOTS ( ( 4, 4 ),
 ( 2, 2 ),
 ( 0.000000000000000000, 1.000000000000000000 ),
 ( 0.000000000000000000, 1.000000000000000000 ),
 .UNSPECIFIED. ) 
 GEOMETRIC_REPRESENTATION_ITEM ( )  RATIONAL_B_SPLINE_SURFACE ( (
 ( 1.000000000000000000, 1.000000000000000000),
 ( 0.9956975270656955868, 0.8568959468854907557),
 ( 0.9956975270656955868, 0.8568959468854907557),
 ( 1.000000000000000000, 1.000000000000000000) ) ) 
 REPRESENTATION_ITEM ( '' )  SURFACE ( )  );
#19198 = DIRECTION ( 'NONE',  ( -0.7563875759206388771, -0.1685564395263341175, 0.6320336713238504656 ) ) ;
#19199 = ADVANCED_FACE ( 'NONE', ( #14207 ), #5943, .F. ) ;
#19200 = CARTESIAN_POINT ( 'NONE',  ( 25.64681081121879203, 66.70335573067866619, 91.10197563707968982 ) ) ;
#19201 = CARTESIAN_POINT ( 'NONE',  ( 119.2224693531408946, -90.00000000000005684, -19.99999999999999645 ) ) ;
#19202 = EDGE_CURVE ( 'NONE', #16069, #27652, #24799, .T. ) ;
#19203 = CARTESIAN_POINT ( 'NONE',  ( 9.884929003653608603, 146.3148513795966608, 35.39789245780380611 ) ) ;
#19204 = EDGE_CURVE ( 'NONE', #24734, #13159, #11928, .T. ) ;
#19205 = EDGE_LOOP ( 'NONE', ( #14682, #12513, #17944, #17140 ) ) ;
#19206 = ORIENTED_EDGE ( 'NONE', *, *, #17028, .T. ) ;
#19208 = CARTESIAN_POINT ( 'NONE',  ( 55.79472521941428198, 37.00555938668259870, 62.63970324008273849 ) ) ;
#19207 = CARTESIAN_POINT ( 'NONE',  ( -5.986830583229317604, -43.56094206392958768, -26.01297580803309728 ) ) ;
#19209 = CARTESIAN_POINT ( 'NONE',  ( 55.49584447822657296, -66.16986612640756960, -29.75369869231020914 ) ) ;
#19210 = CARTESIAN_POINT ( 'NONE',  ( -20.20700224038492721, -16.58740185276692358, 24.51628800869065827 ) ) ;
#19211 = VERTEX_POINT ( 'NONE', #13934 ) ;
#19212 = CARTESIAN_POINT ( 'NONE',  ( 25.64708228042122329, 91.37028996123351021, -66.33571787052716218 ) ) ;
#19213 = CARTESIAN_POINT ( 'NONE',  ( -4.178947244162637631, -25.96944194166761832, 41.47292084251660782 ) ) ;
#19214 = CARTESIAN_POINT ( 'NONE',  ( 28.37644542392838432, -120.7150203538607087, -29.80435743554073724 ) ) ;
#19215 = VERTEX_POINT ( 'NONE', #18108 ) ;
#19216 = VERTEX_POINT ( 'NONE', #22747 ) ;
#19217 = DIRECTION ( 'NONE',  ( 0.7637818620346800147, 0.6068965246771059752, 0.2198041754873819864 ) ) ;
#19218 = ORIENTED_EDGE ( 'NONE', *, *, #7729, .T. ) ;
#19219 = VERTEX_POINT ( 'NONE', #24760 ) ;
#19220 = CARTESIAN_POINT ( 'NONE',  ( 30.59141879584280943, -2.701465575440527012, 116.1811685142589567 ) ) ;
#19221 = ORIENTED_EDGE ( 'NONE', *, *, #3029, .F. ) ;
#19222 = CARTESIAN_POINT ( 'NONE',  ( 1.832998868059858122, 29.64765804470268407, -142.0492247521719946 ) ) ;
#19223 = B_SPLINE_CURVE_WITH_KNOTS ( 'NONE', 3,
 ( #22584, #11917, #15943, #22736, #14198, #20548, #13778, #5293, #22880, #9615, #3001, #20685, #7469 ),
 .UNSPECIFIED., .F., .F.,
 ( 4, 3, 3, 3, 4 ),
 ( 1.250926888277100303E-17, 0.0007657099931970619711, 0.001531419946797935418, 0.002296279302920161639, 0.003061450627205739884 ),
 .UNSPECIFIED. ) ;
#19224 = CARTESIAN_POINT ( 'NONE',  ( 2.108393763691185363, 126.4628696952929374, -71.53437599919685397 ) ) ;
#19225 = EDGE_CURVE ( 'NONE', #14349, #174, #22018, .T. ) ;
#19226 = CARTESIAN_POINT ( 'NONE',  ( 109.1592201516379674, -0.006957642258155097119, -0.003661068210032647052 ) ) ;
#19227 = CARTESIAN_POINT ( 'NONE',  ( -28.13707043255157103, 12.83104814250481596, 18.96624908365832596 ) ) ;
#19228 = CARTESIAN_POINT ( 'NONE',  ( -4.473127245936434626, 3.196405119334491562, 49.22197550883364414 ) ) ;
#19229 = CARTESIAN_POINT ( 'NONE',  ( 32.73300124599732186, 0.000000000000000000, 0.000000000000000000 ) ) ;
#19230 = EDGE_CURVE ( 'NONE', #14713, #17827, #17866, .T. ) ;
#19231 = CARTESIAN_POINT ( 'NONE',  ( 55.79472521941426777, -71.31192372336683150, 14.41365263906529748 ) ) ;
#19233 = CARTESIAN_POINT ( 'NONE',  ( -20.37983603106074781, 24.94323704205437409, -16.25728007463414571 ) ) ;
#19232 = CARTESIAN_POINT ( 'NONE',  ( 1.833485406944043827, 84.86072343962726450, -117.7091014914941809 ) ) ;
#19234 = CARTESIAN_POINT ( 'NONE',  ( -20.21097721712959583, 24.14932359587290023, -17.13687106192352161 ) ) ;
#19235 = EDGE_CURVE ( 'NONE', #2712, #13376, #1266, .T. ) ;
#19236 = VERTEX_POINT ( 'NONE', #19251 ) ;
#19237 = VERTEX_POINT ( 'NONE', #26015 ) ;
#19238 = CARTESIAN_POINT ( 'NONE',  ( -28.41354790283022069, -22.41474081378005323, -5.969609727607934957 ) ) ;
#19239 = CARTESIAN_POINT ( 'NONE',  ( -10.86508079875780730, -35.35100740321749413, 36.95527278096565027 ) ) ;
#19241 = CARTESIAN_POINT ( 'NONE',  ( 1.833206310202331712, 45.54896489827154937, 137.7753867363979623 ) ) ;
#19240 = DIRECTION ( 'NONE',  ( 0.5914120900931444380, 0.4674599267565303085, 0.6570486713847291105 ) ) ;
#19242 = CARTESIAN_POINT ( 'NONE',  ( 26.04756280548355107, -76.55292122839982483, -83.36043467252099504 ) ) ;
#19243 = CARTESIAN_POINT ( 'NONE',  ( 109.1592201516379674, 0.0003082430541934987381, -0.007856029051018018419 ) ) ;
#19244 = ORIENTED_EDGE ( 'NONE', *, *, #7937, .T. ) ;
#19245 = CARTESIAN_POINT ( 'NONE',  ( -23.79223135445720771, 22.01133905265687929, -24.83942264280410228 ) ) ;
#19246 = AXIS2_PLACEMENT_3D ( 'NONE', #18465, #22952, #20332 ) ;
#19247 =( BOUNDED_SURFACE ( )  B_SPLINE_SURFACE ( 3, 1, ( 
 ( #24710, #6849 ),
 ( #351, #15903 ),
 ( #2507, #2358 ),
 ( #6998, #17895 ) ),
 .UNSPECIFIED., .F., .F., .F. ) 
 B_SPLINE_SURFACE_WITH_KNOTS ( ( 4, 4 ),
 ( 2, 2 ),
 ( 0.000000000000000000, 1.000000000000000000 ),
 ( 0.000000000000000000, 1.000000000000000000 ),
 .UNSPECIFIED. ) 
 GEOMETRIC_REPRESENTATION_ITEM ( )  RATIONAL_B_SPLINE_SURFACE ( (
 ( 1.000000000000000000, 1.000000000000000000),
 ( 0.9934239774497838349, 0.8357310067453913582),
 ( 0.9934239774497838349, 0.8357310067453913582),
 ( 1.000000000000000000, 1.000000000000000000) ) ) 
 REPRESENTATION_ITEM ( '' )  SURFACE ( )  );
#19249 = EDGE_CURVE ( 'NONE', #27430, #21234, #19120, .T. ) ;
#19248 = CARTESIAN_POINT ( 'NONE',  ( -1.045287976400379737, -25.66401692420040703, -37.92705037016734337 ) ) ;
#19250 = EDGE_LOOP ( 'NONE', ( #25215, #17114, #19006, #19885 ) ) ;
#19251 = CARTESIAN_POINT ( 'NONE',  ( 10.93730112725978287, -140.0398180619114896, 56.95489579269701608 ) ) ;
#19252 = AXIS2_PLACEMENT_3D ( 'NONE', #21650, #5706, #12443 ) ;
#19253 = CARTESIAN_POINT ( 'NONE',  ( 2.430230287190581429, 31.67257033707698710, -142.0258656395018591 ) ) ;
#19254 = FACE_OUTER_BOUND ( 'NONE', #10509, .T. ) ;
#19255 = CARTESIAN_POINT ( 'NONE',  ( -4.473127245936431073, -37.94261489385741015, -31.51789735524179648 ) ) ;
#19256 = CARTESIAN_POINT ( 'NONE',  ( 1.833485406944043827, 117.0814567582544612, 85.72460230293732764 ) ) ;
#19257 = ORIENTED_EDGE ( 'NONE', *, *, #6351, .F. ) ;
#19258 = FACE_OUTER_BOUND ( 'NONE', #26620, .T. ) ;
#19259 = FACE_OUTER_BOUND ( 'NONE', #13907, .T. ) ;
#19260 = ADVANCED_FACE ( 'NONE', ( #6032 ), #26341, .F. ) ;
#19261 = ORIENTED_EDGE ( 'NONE', *, *, #1816, .T. ) ;
#19262 = CARTESIAN_POINT ( 'NONE',  ( -28.13707043255157103, -6.342158660427161365, -22.00298671236737391 ) ) ;
#19263 = ORIENTED_EDGE ( 'NONE', *, *, #15416, .F. ) ;
#19264 = CARTESIAN_POINT ( 'NONE',  ( -1.155001620486255431, -35.88346938217574689, -28.62773628245655644 ) ) ;
#19265 = CARTESIAN_POINT ( 'NONE',  ( 25.64692232868534560, 97.94691534265433575, 56.17236075411980067 ) ) ;
#19266 = CARTESIAN_POINT ( 'NONE',  ( -1.619063947482197729, -38.92136151114888776, 25.20140673341416360 ) ) ;
#19267 = CARTESIAN_POINT ( 'NONE',  ( 2.433796855181219243, -142.0211193075558356, 31.67151202412923894 ) ) ;
#19268 = CIRCLE ( 'NONE', #9640, 53.53553390275978785 ) ;
#19269 = CARTESIAN_POINT ( 'NONE',  ( -4.162674018437153123, 47.46216648493558665, -11.82104147411576989 ) ) ;
#19270 = FACE_OUTER_BOUND ( 'NONE', #13234, .T. ) ;
#19271 = CARTESIAN_POINT ( 'NONE',  ( 2.433796855181219243, -144.8571464219890004, 13.76554153471645847 ) ) ;
#19272 = EDGE_CURVE ( 'NONE', #2848, #8996, #12215, .T. ) ;
#19273 = CARTESIAN_POINT ( 'NONE',  ( 1.833809397773829675, -59.18399778167225378, 132.4918864201826523 ) ) ;
#19274 = CARTESIAN_POINT ( 'NONE',  ( 109.1589550718175161, -0.007571935245608773894, 0.0002241941239326721372 ) ) ;
#19275 = LINE ( 'NONE', #13202, #19877 ) ;
#19276 = CARTESIAN_POINT ( 'NONE',  ( 1.894214914920953730, -58.16536411968030507, 132.9862534094754665 ) ) ;
#19277 = ORIENTED_EDGE ( 'NONE', *, *, #26640, .F. ) ;
#19278 = EDGE_CURVE ( 'NONE', #8700, #20108, #11363, .T. ) ;
#19279 = VERTEX_POINT ( 'NONE', #10219 ) ;
#19280 = CARTESIAN_POINT ( 'NONE',  ( 25.64681081121879203, -97.57530875170564855, -56.81519825470856944 ) ) ;
#19281 = LINE ( 'NONE', #19558, #1951 ) ;
#19282 = CARTESIAN_POINT ( 'NONE',  ( 32.73300124599738581, -97.37344512919901263, 66.00340565729310072 ) ) ;
#19283 = CARTESIAN_POINT ( 'NONE',  ( 109.1592201516379674, 0.001127733110579580769, -0.007780772729118883360 ) ) ;
#19284 = DIRECTION ( 'NONE',  ( 0.000000000000000000, 0.000000000000000000, 1.000000000000000000 ) ) ;
#19285 = CARTESIAN_POINT ( 'NONE',  ( 24.01988960052036148, 69.18817751538470873, -111.2910478357996453 ) ) ;
#19286 = CARTESIAN_POINT ( 'NONE',  ( 1.833485406944043827, 97.49333871408838093, -107.4794113447399297 ) ) ;
#19287 = ORIENTED_EDGE ( 'NONE', *, *, #20019, .F. ) ;
#19288 = CARTESIAN_POINT ( 'NONE',  ( -20.20700224038492010, 8.199606986804733211, 28.44216453106527709 ) ) ;
#19289 = CARTESIAN_POINT ( 'NONE',  ( -55.24271866751342941, -0.001545935011626541761, -0.009369360294294543784 ) ) ;
#19290 = CARTESIAN_POINT ( 'NONE',  ( 109.1586900883932856, -0.001385221016536898869, -0.007002774699553655259 ) ) ;
#19291 = CARTESIAN_POINT ( 'NONE',  ( -20.38016308990358638, -24.94368798801364662, -16.25718651464972098 ) ) ;
#19292 = B_SPLINE_CURVE_WITH_KNOTS ( 'NONE', 3,
 ( #16689, #3298, #11932, #23185 ),
 .UNSPECIFIED., .F., .F.,
 ( 4, 4 ),
 ( 0.000000000000000000, 0.01077107196513861845 ),
 .UNSPECIFIED. ) ;
#19293 = ORIENTED_EDGE ( 'NONE', *, *, #27529, .T. ) ;
#19294 = CARTESIAN_POINT ( 'NONE',  ( 2.433796855181205476, 43.58222566461644476, 138.8296532063089614 ) ) ;
#19295 = DIRECTION ( 'NONE',  ( -1.000000000000000000, -0.000000000000000000, -0.000000000000000000 ) ) ;
#19296 = ORIENTED_EDGE ( 'NONE', *, *, #15477, .T. ) ;
#19297 = ORIENTED_EDGE ( 'NONE', *, *, #24070, .T. ) ;
#19298 = ORIENTED_EDGE ( 'NONE', *, *, #23499, .T. ) ;
#19299 = APPLICATION_CONTEXT ( 'automotive_design' ) ;
#19300 = CARTESIAN_POINT ( 'NONE',  ( 1.831572820252009626, 96.36280042116079869, -108.4969585352545209 ) ) ;
#19301 = CARTESIAN_POINT ( 'NONE',  ( -20.38016308990357928, 10.62413300761025425, 27.81387210821410250 ) ) ;
#19302 = B_SPLINE_CURVE_WITH_KNOTS ( 'NONE', 3,
 ( #21430, #10501, #16548, #19139, #3452, #25630, #23470 ),
 .UNSPECIFIED., .F., .F.,
 ( 4, 3, 4 ),
 ( 6.012562578665078486E-16, 0.02816610861753242670, 0.04000277880656282620 ),
 .UNSPECIFIED. ) ;
#19303 = ADVANCED_FACE ( 'NONE', ( #3711 ), #29, .F. ) ;
#19304 = ORIENTED_EDGE ( 'NONE', *, *, #26351, .F. ) ;
#19305 = CARTESIAN_POINT ( 'NONE',  ( -1.619063947482194177, 25.20140673341374438, -38.92136151114915066 ) ) ;
#19306 = EDGE_CURVE ( 'NONE', #391, #945, #16513, .T. ) ;
#19307 = EDGE_CURVE ( 'NONE', #15221, #14195, #23791, .T. ) ;
#19308 = DIRECTION ( 'NONE',  ( -1.000000000000000000, -0.000000000000000000, -0.000000000000000000 ) ) ;
#19309 = CARTESIAN_POINT ( 'NONE',  ( 26.11404676487259024, 113.2169081140373947, -1.130420376097525326 ) ) ;
#19310 = CARTESIAN_POINT ( 'NONE',  ( 25.64692872815574276, -12.12228186621135428, 112.2585610031153180 ) ) ;
#19311 = CARTESIAN_POINT ( 'NONE',  ( 32.73300124599734318, 97.37344512919861472, 66.00340565729376863 ) ) ;
#19312 = CARTESIAN_POINT ( 'NONE',  ( 109.1624594426973260, -0.01551217196236916694, -0.003771499231549737489 ) ) ;
#19313 = ORIENTED_EDGE ( 'NONE', *, *, #20267, .T. ) ;
#19314 = ORIENTED_EDGE ( 'NONE', *, *, #2283, .F. ) ;
#19315 = CARTESIAN_POINT ( 'NONE',  ( 1.834118845439484335, -141.9759513273466780, 29.99597360113025246 ) ) ;
#19316 = VECTOR ( 'NONE', #7226, 1000.000000000000114 ) ;
#19317 =( BOUNDED_SURFACE ( )  B_SPLINE_SURFACE ( 3, 1, ( 
 ( #12362, #16543 ),
 ( #12093, #20714 ),
 ( #5460, #12231 ),
 ( #5616, #27333 ) ),
 .UNSPECIFIED., .F., .F., .F. ) 
 B_SPLINE_SURFACE_WITH_KNOTS ( ( 4, 4 ),
 ( 2, 2 ),
 ( 0.000000000000000000, 1.000000000000000000 ),
 ( 0.000000000000000000, 1.000000000000000000 ),
 .UNSPECIFIED. ) 
 GEOMETRIC_REPRESENTATION_ITEM ( )  RATIONAL_B_SPLINE_SURFACE ( (
 ( 1.000000000000000000, 1.000000000000000000),
 ( 0.9593753223639863714, 0.9995975284513187731),
 ( 0.9593753223639863714, 0.9995975284513187731),
 ( 1.000000000000000000, 1.000000000000000000) ) ) 
 REPRESENTATION_ITEM ( '' )  SURFACE ( )  );
#19319 = ORIENTED_EDGE ( 'NONE', *, *, #2865, .T. ) ;
#19318 = CARTESIAN_POINT ( 'NONE',  ( 25.98552792386799837, 35.98568266743512112, 107.2612904323490284 ) ) ;
#19320 = VECTOR ( 'NONE', #25515, 1000.000000000000114 ) ;
#19321 = ORIENTED_EDGE ( 'NONE', *, *, #24725, .T. ) ;
#19322 = EDGE_LOOP ( 'NONE', ( #12663, #9050, #3399, #16214 ) ) ;
#19323 = ORIENTED_EDGE ( 'NONE', *, *, #19398, .F. ) ;
#19324 = CONICAL_SURFACE ( 'NONE', #16583, 34.60786435723138510, 0.8559913436420825139 ) ;
#19325 =( BOUNDED_SURFACE ( )  B_SPLINE_SURFACE ( 3, 1, ( 
 ( #23854, #8711 ),
 ( #25992, #4525 ),
 ( #8571, #17767 ),
 ( #19365, #17478 ) ),
 .UNSPECIFIED., .F., .F., .F. ) 
 B_SPLINE_SURFACE_WITH_KNOTS ( ( 4, 4 ),
 ( 2, 2 ),
 ( 0.000000000000000000, 1.000000000000000000 ),
 ( 0.000000000000000000, 1.000000000000000000 ),
 .UNSPECIFIED. ) 
 GEOMETRIC_REPRESENTATION_ITEM ( )  RATIONAL_B_SPLINE_SURFACE ( (
 ( 1.000000000000000000, 1.000000000000000000),
 ( 0.9956975270656954757, 0.8568959468854893125),
 ( 0.9956975270656954757, 0.8568959468854893125),
 ( 1.000000000000000000, 1.000000000000000000) ) ) 
 REPRESENTATION_ITEM ( '' )  SURFACE ( )  );
#19326 = EDGE_CURVE ( 'NONE', #11861, #4018, #12095, .T. ) ;
#19327 = CONICAL_SURFACE ( 'NONE', #16133, 117.6351876552689504, 0.9945805576725580410 ) ;
#19328 = CARTESIAN_POINT ( 'NONE',  ( -22.23226125620930560, 7.677408153694024406, -30.68305173820428067 ) ) ;
#19329 = EDGE_CURVE ( 'NONE', #823, #27505, #14771, .T. ) ;
#19330 = EDGE_CURVE ( 'NONE', #2536, #20059, #1728, .T. ) ;
#19331 = CARTESIAN_POINT ( 'NONE',  ( 94.22246935314088034, -69.99999999999998579, -12.50000000000000888 ) ) ;
#19332 = CARTESIAN_POINT ( 'NONE',  ( 28.37599760073042887, -84.05168479399036130, -78.09498850373492473 ) ) ;
#19333 = VECTOR ( 'NONE', #25709, 999.9999999999998863 ) ;
#19334 = FACE_OUTER_BOUND ( 'NONE', #23293, .T. ) ;
#19335 = CIRCLE ( 'NONE', #22564, 117.6351876552689504 ) ;
#19336 = CARTESIAN_POINT ( 'NONE',  ( -55.24300891470648622, -0.006048736206180239418, 0.007734635432132643158 ) ) ;
#19337 = CARTESIAN_POINT ( 'NONE',  ( 109.1592201516379674, 0.007780772729118878156, 0.001127733110579607657 ) ) ;
#19338 = CARTESIAN_POINT ( 'NONE',  ( -28.13707043255157103, -0.7675454997505393173, 22.88591869784691468 ) ) ;
#19339 = VECTOR ( 'NONE', #8311, 1000.000000000000227 ) ;
#19340 = EDGE_LOOP ( 'NONE', ( #5163, #25713, #20991, #11616 ) ) ;
#19341 = EDGE_LOOP ( 'NONE', ( #4896, #16318, #21377, #3458 ) ) ;
#19342 = B_SPLINE_CURVE_WITH_KNOTS ( 'NONE', 3,
 ( #19100, #1386, #27873, #11907, #20675, #9755, #23291 ),
 .UNSPECIFIED., .F., .F.,
 ( 4, 3, 4 ),
 ( 3.404394821604483923E-17, 0.0002669559177086210989, 0.0005339083821128836910 ),
 .UNSPECIFIED. ) ;
#19344 = DIRECTION ( 'NONE',  ( -0.5914120900931443270, 0.4101107478122070771, 0.6942916636548150944 ) ) ;
#19343 = CARTESIAN_POINT ( 'NONE',  ( 25.64704443564078673, 112.9111375659905292, 0.1334765861207808380 ) ) ;
#19345 = CARTESIAN_POINT ( 'NONE',  ( -1.056502255334265339, 43.72121397317224734, -13.66916755949864637 ) ) ;
#19346 = DIRECTION ( 'NONE',  ( -0.7637818620346800147, 0.6201872550346668733, 0.1788995134688804445 ) ) ;
#19347 = CARTESIAN_POINT ( 'NONE',  ( 25.98107933586726759, 112.6229961579375924, -10.73978443746618439 ) ) ;
#19348 = ORIENTED_EDGE ( 'NONE', *, *, #780, .F. ) ;
#19349 = CARTESIAN_POINT ( 'NONE',  ( 25.64704443564079739, 97.85065179540836766, -56.33997466860298431 ) ) ;
#19350 = CARTESIAN_POINT ( 'NONE',  ( 24.01988960052045741, 90.81495976423938998, -94.47404045191558453 ) ) ;
#19351 = LINE ( 'NONE', #4095, #22207 ) ;
#19352 = ORIENTED_EDGE ( 'NONE', *, *, #3645, .T. ) ;
#19353 = ORIENTED_EDGE ( 'NONE', *, *, #17643, .F. ) ;
#19354 = B_SPLINE_CURVE_WITH_KNOTS ( 'NONE', 3,
 ( #22184, #9086, #17846, #4908, #18139, #15687 ),
 .UNSPECIFIED., .F., .F.,
 ( 4, 2, 4 ),
 ( 9.341771812940338307E-18, 0.003576372551510817021, 0.007152745103021624501 ),
 .UNSPECIFIED. ) ;
#19355 = DIRECTION ( 'NONE',  ( -1.000000000000000000, -0.000000000000000000, -0.000000000000000000 ) ) ;
#19356 = VERTEX_POINT ( 'NONE', #24013 ) ;
#19357 = EDGE_LOOP ( 'NONE', ( #26960, #19978, #18173, #9849 ) ) ;
#19358 = CIRCLE ( 'NONE', #24912, 53.53553390275978785 ) ;
#19359 = AXIS2_PLACEMENT_3D ( 'NONE', #12377, #28058, #28194 ) ;
#19360 = CARTESIAN_POINT ( 'NONE',  ( 32.73300124599735739, -3.836798148479648507, 117.5726003567929610 ) ) ;
#19361 = ADVANCED_FACE ( 'NONE', ( #2526 ), #26504, .F. ) ;
#19362 =( BOUNDED_SURFACE ( )  B_SPLINE_SURFACE ( 3, 1, ( 
 ( #8155, #16922 ),
 ( #3822, #12587 ),
 ( #20812, #1097 ),
 ( #9886, #18651 ) ),
 .UNSPECIFIED., .F., .F., .F. ) 
 B_SPLINE_SURFACE_WITH_KNOTS ( ( 4, 4 ),
 ( 2, 2 ),
 ( 0.000000000000000000, 1.000000000000000000 ),
 ( 0.000000000000000000, 1.000000000000000000 ),
 .UNSPECIFIED. ) 
 GEOMETRIC_REPRESENTATION_ITEM ( )  RATIONAL_B_SPLINE_SURFACE ( (
 ( 1.000000000000000000, 1.000000000000000000),
 ( 0.9934239774497837239, 0.8357310067453919133),
 ( 0.9934239774497837239, 0.8357310067453919133),
 ( 1.000000000000000000, 1.000000000000000000) ) ) 
 REPRESENTATION_ITEM ( '' )  SURFACE ( )  );
#19363 = EDGE_CURVE ( 'NONE', #20199, #21696, #24370, .T. ) ;
#19364 = ORIENTED_EDGE ( 'NONE', *, *, #12705, .T. ) ;
#19365 = CARTESIAN_POINT ( 'NONE',  ( 109.1586900883932856, -0.003656351050331892692, -0.006130969560687349849 ) ) ;
#19366 = CARTESIAN_POINT ( 'NONE',  ( 2.433796855181233454, -125.2830755159759519, 74.00833731765517598 ) ) ;
#19367 = CARTESIAN_POINT ( 'NONE',  ( -1.050229599974486616, 13.90955673306187990, 43.63650726458048013 ) ) ;
#19368 = CARTESIAN_POINT ( 'NONE',  ( -1.239374126674604337, 45.98822239537607004, 2.406737988131282702 ) ) ;
#19369 = CARTESIAN_POINT ( 'NONE',  ( -25.21435515916043713, -34.05351380035328646, 6.169479169075816394 ) ) ;
#19370 = CARTESIAN_POINT ( 'NONE',  ( 26.04756280548352265, 103.8403168215175754, 45.01666824410803258 ) ) ;
#19371 = CARTESIAN_POINT ( 'NONE',  ( 2.433796855181205476, 96.28145139437683042, 109.1007109081229345 ) ) ;
#19372 = CARTESIAN_POINT ( 'NONE',  ( 25.64660436782540387, 98.07256794792336052, 55.95243482911432409 ) ) ;
#19373 = ORIENTED_EDGE ( 'NONE', *, *, #7333, .F. ) ;
#19374 = B_SPLINE_CURVE_WITH_KNOTS ( 'NONE', 3,
 ( #13602, #17779, #21829, #11310, #24141, #362 ),
 .UNSPECIFIED., .F., .F.,
 ( 4, 2, 4 ),
 ( 6.952433221959954168E-18, 0.0006311571484586070901, 0.001262314296917207458 ),
 .UNSPECIFIED. ) ;
#19375 = ORIENTED_EDGE ( 'NONE', *, *, #24563, .T. ) ;
#19376 = FACE_OUTER_BOUND ( 'NONE', #1247, .T. ) ;
#19377 = CARTESIAN_POINT ( 'NONE',  ( -28.41354790283022069, 1.249099604787076601, -23.16239616762931064 ) ) ;
#19379 = CARTESIAN_POINT ( 'NONE',  ( 21.16825799904893302, 18.54093663547828896, 134.1581724640165021 ) ) ;
#19378 = CARTESIAN_POINT ( 'NONE',  ( 9.884929003653608603, -27.17402761732236627, -148.0628878137283380 ) ) ;
#19380 = VECTOR ( 'NONE', #1720, 1000.000000000000000 ) ;
#19381 = CARTESIAN_POINT ( 'NONE',  ( -1.046935749539998906, -43.93230528057173956, 12.93334586714225054 ) ) ;
#19382 = B_SPLINE_CURVE_WITH_KNOTS ( 'NONE', 3,
 ( #9082, #9383, #26913, #6933, #24786, #4763, #3320, #3460, #12244, #23479 ),
 .UNSPECIFIED., .F., .F.,
 ( 4, 2, 2, 2, 4 ),
 ( 4.210279659405072890E-18, 0.0003346267210630959280, 0.0006692534421261876277, 0.001003880163189279110, 0.001338506884252370919 ),
 .UNSPECIFIED. ) ;
#19383 = CARTESIAN_POINT ( 'NONE',  ( -2.265401668238148591, 2.645701981445804929, -46.93990709177545995 ) ) ;
#19384 = EDGE_CURVE ( 'NONE', #13723, #12509, #4469, .T. ) ;
#19385 = CARTESIAN_POINT ( 'NONE',  ( -1.019300379054419725, -42.90269154183418010, 16.06793277092037187 ) ) ;
#19386 = EDGE_LOOP ( 'NONE', ( #7743, #7349, #9068, #25912 ) ) ;
#19387 = CARTESIAN_POINT ( 'NONE',  ( 32.73300124599734318, 99.90245962373836619, 62.10906484417276374 ) ) ;
#19388 = CYLINDRICAL_SURFACE ( 'NONE', #22582, 37.50000000000001421 ) ;
#19389 = CARTESIAN_POINT ( 'NONE',  ( 25.64700659047694487, 112.2686754657455168, 12.02873506870207443 ) ) ;
#19390 = CARTESIAN_POINT ( 'NONE',  ( -20.47566262905010248, -1.586617686065349808, 29.82700878811085232 ) ) ;
#19391 = ORIENTED_EDGE ( 'NONE', *, *, #3912, .T. ) ;
#19392 = CARTESIAN_POINT ( 'NONE',  ( -55.24390624410018802, -0.004896917417131185259, 0.009209468562452437224 ) ) ;
#19393 = ADVANCED_FACE ( 'NONE', ( #15052 ), #7975, .F. ) ;
#19394 = CARTESIAN_POINT ( 'NONE',  ( 2.063896406836609909, -13.84738934186288084, 144.6078654718901362 ) ) ;
#19395 = EDGE_CURVE ( 'NONE', #18219, #14717, #14790, .T. ) ;
#19396 = ORIENTED_EDGE ( 'NONE', *, *, #2533, .T. ) ;
#19397 = CARTESIAN_POINT ( 'NONE',  ( 13.84597867724966669, -94.55652763153750584, -112.1633818588836107 ) ) ;
#19398 = EDGE_CURVE ( 'NONE', #28326, #10330, #4200, .T. ) ;
#19399 = CARTESIAN_POINT ( 'NONE',  ( -25.21435515916025594, 1.749597353048488237E-16, -4.373993382621220594E-17 ) ) ;
#19400 = B_SPLINE_CURVE_WITH_KNOTS ( 'NONE', 3,
 ( #25604, #20973, #25172, #9918 ),
 .UNSPECIFIED., .F., .F.,
 ( 4, 4 ),
 ( 3.105545673626859933E-16, 0.01077107486149834689 ),
 .UNSPECIFIED. ) ;
#19401 = FACE_OUTER_BOUND ( 'NONE', #14712, .T. ) ;
#19402 = B_SPLINE_CURVE_WITH_KNOTS ( 'NONE', 3,
 ( #249, #25027, #2692, #3128 ),
 .UNSPECIFIED., .F., .F.,
 ( 4, 4 ),
 ( 1.847623020647441449E-16, 0.001982023823822945483 ),
 .UNSPECIFIED. ) ;
#19403 = CARTESIAN_POINT ( 'NONE',  ( 1.833485406944057594, -72.09189602597798796, 125.9346397303433065 ) ) ;
#19404 = VECTOR ( 'NONE', #1114, 1000.000000000000114 ) ;
#19405 = CARTESIAN_POINT ( 'NONE',  ( -1.049817751779888786, 36.75003908324330837, 27.33161971822157810 ) ) ;
#19406 = EDGE_CURVE ( 'NONE', #23707, #25959, #5501, .T. ) ;
#19407 = CARTESIAN_POINT ( 'NONE',  ( -55.24271866751342941, -0.006671293903667674559, -0.006757859501010194010 ) ) ;
#19408 = CARTESIAN_POINT ( 'NONE',  ( 1.833485406944043827, -132.7804117027891948, 58.53321471326832182 ) ) ;
#19409 = CARTESIAN_POINT ( 'NONE',  ( 1.833750490713655479, -137.9248034078894989, -45.09517546033787738 ) ) ;
#19410 = PLANE ( 'NONE',  #9690 ) ;
#19411 = CARTESIAN_POINT ( 'NONE',  ( -4.162674018437130030, 3.424137510344948510, -48.79210541969630555 ) ) ;
#19412 = CARTESIAN_POINT ( 'NONE',  ( -25.21435515916043357, -16.39063784838764093, -30.48034229288631991 ) ) ;
#19413 =( BOUNDED_SURFACE ( )  B_SPLINE_SURFACE ( 3, 1, ( 
 ( #4353, #8826 ),
 ( #19895, #17584 ),
 ( #21628, #8968 ),
 ( #26369, #6672 ) ),
 .UNSPECIFIED., .F., .F., .F. ) 
 B_SPLINE_SURFACE_WITH_KNOTS ( ( 4, 4 ),
 ( 2, 2 ),
 ( 0.000000000000000000, 1.000000000000000000 ),
 ( 0.000000000000000000, 1.000000000000000000 ),
 .UNSPECIFIED. ) 
 GEOMETRIC_REPRESENTATION_ITEM ( )  RATIONAL_B_SPLINE_SURFACE ( (
 ( 1.000000000000000000, 1.000000000000000000),
 ( 0.9956975270656954757, 0.8568959468854893125),
 ( 0.9956975270656954757, 0.8568959468854893125),
 ( 1.000000000000000000, 1.000000000000000000) ) ) 
 REPRESENTATION_ITEM ( '' )  SURFACE ( )  );
#19414 = CARTESIAN_POINT ( 'NONE',  ( -9.156249394959706578, -9.022661520478157726, -53.74753343182698728 ) ) ;
#19415 = CARTESIAN_POINT ( 'NONE',  ( 5.340103579038259163, -17.70136536264566729, -146.3832392131353402 ) ) ;
#19416 = CARTESIAN_POINT ( 'NONE',  ( -20.47566338032535782, -10.72601609985042792, -27.87687989047296355 ) ) ;
#19417 = ORIENTED_EDGE ( 'NONE', *, *, #2993, .F. ) ;
#19418 = B_SPLINE_CURVE_WITH_KNOTS ( 'NONE', 3,
 ( #6657, #15404, #6796, #443 ),
 .UNSPECIFIED., .F., .F.,
 ( 4, 4 ),
 ( 0.000000000000000000, 0.008383560773332705135 ),
 .UNSPECIFIED. ) ;
#19419 = ORIENTED_EDGE ( 'NONE', *, *, #21419, .T. ) ;
#19420 = CARTESIAN_POINT ( 'NONE',  ( 109.1586059443104944, 0.0002768082440288753641, 0.007068659269321312354 ) ) ;
#19421 = CARTESIAN_POINT ( 'NONE',  ( -8.786685647604898008, 48.22796981442765940, -23.24040270374399952 ) ) ;
#19422 = CARTESIAN_POINT ( 'NONE',  ( -8.786685647604885574, 6.096987947571466530E-17, -1.524246986892866633E-17 ) ) ;
#19423 = FACE_OUTER_BOUND ( 'NONE', #6662, .T. ) ;
#19424 = CARTESIAN_POINT ( 'NONE',  ( 10.93730112726005999, 136.0306644680993600, -65.95960219662998725 ) ) ;
#19425 = CARTESIAN_POINT ( 'NONE',  ( -9.156249394959713683, 48.32878616081047340, 25.18996226954561735 ) ) ;
#19426 = CARTESIAN_POINT ( 'NONE',  ( -1.049819825607587465, 26.50610175068268859, -37.34982882986852815 ) ) ;
#19427 = ORIENTED_EDGE ( 'NONE', *, *, #26088, .T. ) ;
#19428 = DIRECTION ( 'NONE',  ( 0.000000000000000000, 0.000000000000000000, 1.000000000000000000 ) ) ;
#19429 = CARTESIAN_POINT ( 'NONE',  ( 109.1778270068192853, 0.004106684808172231596, -0.008360410075186628168 ) ) ;
#19430 = DIRECTION ( 'NONE',  ( 0.000000000000000000, 5.223019709707975211E-21, -1.000000000000000000 ) ) ;
#19431 = CARTESIAN_POINT ( 'NONE',  ( 25.64681081121879203, 0.4157506337727869816, 112.9102952884414464 ) ) ;
#19432 = AXIS2_PLACEMENT_3D ( 'NONE', #2189, #19757, #50 ) ;
#19433 = AXIS2_PLACEMENT_3D ( 'NONE', #6306, #28161, #1820 ) ;
#19434 = ORIENTED_EDGE ( 'NONE', *, *, #1696, .F. ) ;
#19435 = CARTESIAN_POINT ( 'NONE',  ( -20.57838717382308147, 7.715628353034087894, 28.96176188950209962 ) ) ;
#19436 = DIRECTION ( 'NONE',  ( 0.000000000000000000, 0.000000000000000000, 1.000000000000000000 ) ) ;
#19437 = ORIENTED_EDGE ( 'NONE', *, *, #27770, .F. ) ;
#19438 = EDGE_CURVE ( 'NONE', #26175, #12942, #26981, .T. ) ;
#19439 = EDGE_LOOP ( 'NONE', ( #5739, #3466, #4945, #20529 ) ) ;
#19440 = ORIENTED_EDGE ( 'NONE', *, *, #11499, .F. ) ;
#19441 = EDGE_CURVE ( 'NONE', #24512, #1061, #2746, .T. ) ;
#19442 = B_SPLINE_CURVE_WITH_KNOTS ( 'NONE', 3,
 ( #24714, #15597, #26416, #20077, #15907, #9014 ),
 .UNSPECIFIED., .F., .F.,
 ( 4, 2, 4 ),
 ( 6.505213034913026604E-19, 0.0004335151646191478343, 0.0008670303292382950180 ),
 .UNSPECIFIED. ) ;
#19443 = AXIS2_PLACEMENT_3D ( 'NONE', #14727, #24098, #26230 ) ;
#19444 = FACE_OUTER_BOUND ( 'NONE', #17476, .T. ) ;
#19445 = CONICAL_SURFACE ( 'NONE', #7053, 117.6351876552689504, 0.9945805576725580410 ) ;
#19446 = DIRECTION ( 'NONE',  ( 1.000000000000000000, -6.938893903907226837E-18, 1.734723475976806709E-18 ) ) ;
#19447 = VECTOR ( 'NONE', #17293, 1000.000000000000000 ) ;
#19448 = CARTESIAN_POINT ( 'NONE',  ( -55.24198130335446422, 0.008310594958151115014, 0.004163123460805739397 ) ) ;
#19449 = VECTOR ( 'NONE', #12140, 1000.000000000000000 ) ;
#19450 =( BOUNDED_SURFACE ( )  B_SPLINE_SURFACE ( 3, 1, ( 
 ( #22220, #9263 ),
 ( #24538, #26811 ),
 ( #17598, #4801 ),
 ( #13565, #7120 ) ),
 .UNSPECIFIED., .F., .F., .F. ) 
 B_SPLINE_SURFACE_WITH_KNOTS ( ( 4, 4 ),
 ( 2, 2 ),
 ( 0.000000000000000000, 1.000000000000000000 ),
 ( 0.000000000000000000, 1.000000000000000000 ),
 .UNSPECIFIED. ) 
 GEOMETRIC_REPRESENTATION_ITEM ( )  RATIONAL_B_SPLINE_SURFACE ( (
 ( 1.000000000000000000, 1.000000000000000000),
 ( 0.9934239774497837239, 0.8357310067453919133),
 ( 0.9934239774497837239, 0.8357310067453919133),
 ( 1.000000000000000000, 1.000000000000000000) ) ) 
 REPRESENTATION_ITEM ( '' )  SURFACE ( )  );
#19451 = CARTESIAN_POINT ( 'NONE',  ( 2.433796855181219243, -43.58222566461740399, 138.8296532063086772 ) ) ;
#19452 = ORIENTED_EDGE ( 'NONE', *, *, #6891, .T. ) ;
#19453 = CARTESIAN_POINT ( 'NONE',  ( -8.786685647604706162, -38.68584556812290032, 37.00619870957955015 ) ) ;
#19454 = CARTESIAN_POINT ( 'NONE',  ( -1.031422197589716205, -12.69107518035533211, -44.01264471863842687 ) ) ;
#19455 = CARTESIAN_POINT ( 'NONE',  ( 109.1721716018069657, 0.01695288006057379254, -0.001984900887706451695 ) ) ;
#19456 = DIRECTION ( 'NONE',  ( 0.000000000000000000, 0.000000000000000000, 1.000000000000000000 ) ) ;
#19457 = CARTESIAN_POINT ( 'NONE',  ( -55.24198130335446422, -0.006527480770973291720, -0.006617369590172134802 ) ) ;
#19458 = B_SPLINE_CURVE_WITH_KNOTS ( 'NONE', 3,
 ( #20730, #17844, #587, #22334, #2596, #26915, #11380 ),
 .UNSPECIFIED., .F., .F.,
 ( 4, 3, 4 ),
 ( 0.000000000000000000, 0.02398743853561338679, 0.04000277880656215312 ),
 .UNSPECIFIED. ) ;
#19459 = CARTESIAN_POINT ( 'NONE',  ( 32.73300124599735028, 110.6325518752274206, 39.98094346392350218 ) ) ;
#19460 = B_SPLINE_CURVE_WITH_KNOTS ( 'NONE', 3,
 ( #22908, #22467, #3168, #11945, #20717, #27036, #22322 ),
 .UNSPECIFIED., .F., .F.,
 ( 4, 3, 4 ),
 ( 0.000000000000000000, 0.02398743853561350475, 0.04000277880656220864 ),
 .UNSPECIFIED. ) ;
#19461 = CARTESIAN_POINT ( 'NONE',  ( 6.224689322667647851, -111.7293398381258243, -97.14981701196437314 ) ) ;
#19462 = B_SPLINE_CURVE_WITH_KNOTS ( 'NONE', 3,
 ( #11207, #20118, #2558, #5004, #26881, #17808, #4578, #13641, #266, #22587 ),
 .UNSPECIFIED., .F., .F.,
 ( 4, 2, 2, 2, 4 ),
 ( 2.799429325053882983E-16, 0.0003346187017559012328, 0.0006692374035115225247, 0.001003856105267143762, 0.001338474807022765108 ),
 .UNSPECIFIED. ) ;
#19463 = CARTESIAN_POINT ( 'NONE',  ( 2.430230287190572103, 118.5711603495692827, -84.35270093935136515 ) ) ;
#19464 = ORIENTED_EDGE ( 'NONE', *, *, #11837, .T. ) ;
#19465 = ORIENTED_EDGE ( 'NONE', *, *, #4130, .T. ) ;
#19466 = CARTESIAN_POINT ( 'NONE',  ( 1.834118845439484335, 14.99112450600438429, -144.3336252355295528 ) ) ;
#19467 = CARTESIAN_POINT ( 'NONE',  ( 25.87036335909427365, 35.87755773825718109, 107.2165474610295490 ) ) ;
#19468 = ORIENTED_EDGE ( 'NONE', *, *, #909, .F. ) ;
#19469 = ADVANCED_FACE ( 'NONE', ( #14037 ), #17508, .F. ) ;
#19470 = VERTEX_POINT ( 'NONE', #11452 ) ;
#19471 = ORIENTED_EDGE ( 'NONE', *, *, #14854, .F. ) ;
#19472 = EDGE_CURVE ( 'NONE', #9093, #14545, #2363, .T. ) ;
#19473 = EDGE_CURVE ( 'NONE', #20885, #14674, #10667, .T. ) ;
#19474 = CARTESIAN_POINT ( 'NONE',  ( 2.263178607246656426, -145.3892423243864584, 1.401567185705964169 ) ) ;
#19475 = CARTESIAN_POINT ( 'NONE',  ( -22.23342874802668589, 26.81018246605539446, -16.78332232459650797 ) ) ;
#19476 = FACE_OUTER_BOUND ( 'NONE', #1939, .T. ) ;
#19477 = VECTOR ( 'NONE', #17888, 1000.000000000000000 ) ;
#19478 = CARTESIAN_POINT ( 'NONE',  ( -1.048172774974290622, 43.86067135048637766, 13.17853518375252442 ) ) ;
#19479 = CARTESIAN_POINT ( 'NONE',  ( 5.340103579038033565, 147.4316330314911738, -2.303180387975705123 ) ) ;
#19480 = CARTESIAN_POINT ( 'NONE',  ( 28.37603512858450117, 84.05169593519829618, -78.09501335733503424 ) ) ;
#19481 = CARTESIAN_POINT ( 'NONE',  ( 2.263178113027048521, 108.9830942735805905, -96.24282436106508953 ) ) ;
#19482 = FACE_OUTER_BOUND ( 'NONE', #17516, .T. ) ;
#19483 = CARTESIAN_POINT ( 'NONE',  ( -1.050229599974492833, 37.20249516760172526, -26.71319688967646755 ) ) ;
#19484 = VERTEX_POINT ( 'NONE', #24856 ) ;
#19485 = ORIENTED_EDGE ( 'NONE', *, *, #26191, .F. ) ;
#19487 = CARTESIAN_POINT ( 'NONE',  ( 25.65782528836480836, -56.95887699624806544, 97.50004228081037638 ) ) ;
#19486 = CARTESIAN_POINT ( 'NONE',  ( 109.1587776205901861, -0.003592288931003392340, 0.006388631651935879063 ) ) ;
#19488 = CARTESIAN_POINT ( 'NONE',  ( 25.64703792032466367, -103.2099561461821793, -45.78915563622668117 ) ) ;
#19489 = B_SPLINE_CURVE_WITH_KNOTS ( 'NONE', 3,
 ( #15801, #2549, #17939, #9475 ),
 .UNSPECIFIED., .F., .F.,
 ( 4, 4 ),
 ( 3.313460909250643119E-16, 0.01077107486149829832 ),
 .UNSPECIFIED. ) ;
#19490 = CARTESIAN_POINT ( 'NONE',  ( -20.37983603106074426, 10.62371319148641291, -27.81368274044714539 ) ) ;
#19491 = CARTESIAN_POINT ( 'NONE',  ( -2.265401668238157473, 39.53028715828234851, -25.45016726748328040 ) ) ;
#19492 = CARTESIAN_POINT ( 'NONE',  ( 25.64670758986457955, 91.63870681572909405, -65.96397693491071834 ) ) ;
#19493 = EDGE_CURVE ( 'NONE', #9341, #11691, #15789, .T. ) ;
#19494 = VERTEX_POINT ( 'NONE', #2670 ) ;
#19495 = CARTESIAN_POINT ( 'NONE',  ( -8.786685647604890903, 25.35688121747502066, -47.14957014837363403 ) ) ;
#19496 = CARTESIAN_POINT ( 'NONE',  ( -1.049819825607600121, -37.34982882986862052, -26.50610175068254293 ) ) ;
#19497 = ORIENTED_EDGE ( 'NONE', *, *, #1905, .T. ) ;
#19498 = EDGE_LOOP ( 'NONE', ( #11782, #1808, #4096, #13983 ) ) ;
#19499 = EDGE_CURVE ( 'NONE', #16228, #17548, #17518, .T. ) ;
#19500 = FACE_OUTER_BOUND ( 'NONE', #23770, .T. ) ;
#19501 =( BOUNDED_SURFACE ( )  B_SPLINE_SURFACE ( 3, 1, ( 
 ( #26619, #155 ),
 ( #22175, #8796 ),
 ( #8650, #9220 ),
 ( #8946, #20147 ) ),
 .UNSPECIFIED., .F., .F., .F. ) 
 B_SPLINE_SURFACE_WITH_KNOTS ( ( 4, 4 ),
 ( 2, 2 ),
 ( 0.000000000000000000, 1.000000000000000000 ),
 ( 0.000000000000000000, 1.000000000000000000 ),
 .UNSPECIFIED. ) 
 GEOMETRIC_REPRESENTATION_ITEM ( )  RATIONAL_B_SPLINE_SURFACE ( (
 ( 1.000000000000000000, 1.000000000000000000),
 ( 0.7789835883360576307, 0.9689951854195403280),
 ( 0.7789835883360576307, 0.9689951854195403280),
 ( 1.000000000000000000, 1.000000000000000000) ) ) 
 REPRESENTATION_ITEM ( '' )  SURFACE ( )  );
#19502 = CARTESIAN_POINT ( 'NONE',  ( -23.79223135445719350, -3.207301057648115350, 33.03345552685149755 ) ) ;
#19503 = VERTEX_POINT ( 'NONE', #803 ) ;
#19504 = CARTESIAN_POINT ( 'NONE',  ( -8.786685647604885574, 6.096987947571466530E-17, -1.524246986892866633E-17 ) ) ;
#19505 = VERTEX_POINT ( 'NONE', #23275 ) ;
#19506 = FACE_OUTER_BOUND ( 'NONE', #13948, .T. ) ;
#19507 = CARTESIAN_POINT ( 'NONE',  ( 2.430230287190572103, -16.65331920325837345, 144.5585181921885294 ) ) ;
#19508 = CARTESIAN_POINT ( 'NONE',  ( 109.1592201516379674, 0.003661068210032671338, -0.006957642258155084976 ) ) ;
#19509 = CARTESIAN_POINT ( 'NONE',  ( -8.786685647604890903, -53.04920435127188938, -7.199674155858766689 ) ) ;
#19510 = CARTESIAN_POINT ( 'NONE',  ( -25.21435515916043713, -30.48034229288650820, -16.39063784838731053 ) ) ;
#19511 = CARTESIAN_POINT ( 'NONE',  ( 109.1589550718174877, 0.007453082872776639785, -0.001354998915261358293 ) ) ;
#19512 = DIRECTION ( 'NONE',  ( 0.5914120900931444380, 0.1754905759872898430, -0.7870418015781041055 ) ) ;
#19513 = ORIENTED_EDGE ( 'NONE', *, *, #27619, .F. ) ;
#19514 = CARTESIAN_POINT ( 'NONE',  ( -20.47566262905010248, 7.708089517695595028, 28.85746289809567600 ) ) ;
#19515 = CARTESIAN_POINT ( 'NONE',  ( -24.53239521893647179, -33.71193723315173685, -3.868435622621356096 ) ) ;
#19516 = CARTESIAN_POINT ( 'NONE',  ( -1.019300379054419947, -12.21833869579496579, -44.15350047934394695 ) ) ;
#19517 = ORIENTED_EDGE ( 'NONE', *, *, #20738, .F. ) ;
#19518 = VERTEX_POINT ( 'NONE', #27856 ) ;
#19519 = CARTESIAN_POINT ( 'NONE',  ( 2.433796855181233454, -96.28145139437756939, 109.1007109081222666 ) ) ;
#19520 = B_SPLINE_CURVE_WITH_KNOTS ( 'NONE', 3,
 ( #26896, #24059, #13095, #21881, #11080, #24192, #13224, #22012, #2274, #139 ),
 .UNSPECIFIED., .F., .F.,
 ( 4, 3, 3, 4 ),
 ( 7.850462293418877066E-17, 0.0002669559177086319409, 0.0005339118354151246425, 0.001067817517169165117 ),
 .UNSPECIFIED. ) ;
#19521 = CARTESIAN_POINT ( 'NONE',  ( 1.833721034905666958, -72.24642519953862063, 125.8463597577924276 ) ) ;
#19523 = CARTESIAN_POINT ( 'NONE',  ( 1.833485406944043827, -117.0814567582538501, -85.72460230293812344 ) ) ;
#19522 = CARTESIAN_POINT ( 'NONE',  ( 10.93730112725969938, 79.81734490845904872, 128.3908183996593948 ) ) ;
#19524 = FACE_OUTER_BOUND ( 'NONE', #21846, .T. ) ;
#19525 = CARTESIAN_POINT ( 'NONE',  ( 25.73574536432415272, 97.42965068311228549, 57.18187897120832019 ) ) ;
#19526 = CARTESIAN_POINT ( 'NONE',  ( 30.59141879584273482, 113.0806649571965465, 26.79785525806430968 ) ) ;
#19527 = ADVANCED_FACE ( 'NONE', ( #18939 ), #961, .F. ) ;
#19528 = EDGE_LOOP ( 'NONE', ( #16459, #12064, #22496, #14010 ) ) ;
#19529 = CARTESIAN_POINT ( 'NONE',  ( 1.833750490713653480, -45.09517546033740842, 137.9248034078896410 ) ) ;
#19530 = ADVANCED_FACE ( 'NONE', ( #25570 ), #7799, .F. ) ;
#19531 = CARTESIAN_POINT ( 'NONE',  ( 1.833485406944057594, -144.3694338680884073, -14.63699153649508311 ) ) ;
#19532 = CARTESIAN_POINT ( 'NONE',  ( 25.70243777736188662, -91.80600962488439620, 65.79472741891235898 ) ) ;
#19533 = CARTESIAN_POINT ( 'NONE',  ( -1.619063947482194177, -46.30105812165547974, 2.489035965910640247 ) ) ;
#19535 = EDGE_CURVE ( 'NONE', #7680, #21385, #4653, .T. ) ;
#19534 = ORIENTED_EDGE ( 'NONE', *, *, #3196, .F. ) ;
#19536 = CARTESIAN_POINT ( 'NONE',  ( 2.430230287190581429, 28.83279105684427535, 142.6294793592098813 ) ) ;
#19537 =( BOUNDED_SURFACE ( )  B_SPLINE_SURFACE ( 3, 1, ( 
 ( #3068, #27519 ),
 ( #7688, #20612 ),
 ( #18607, #20755 ),
 ( #2926, #14266 ) ),
 .UNSPECIFIED., .F., .F., .F. ) 
 B_SPLINE_SURFACE_WITH_KNOTS ( ( 4, 4 ),
 ( 2, 2 ),
 ( 0.000000000000000000, 1.000000000000000000 ),
 ( 0.000000000000000000, 1.000000000000000000 ),
 .UNSPECIFIED. ) 
 GEOMETRIC_REPRESENTATION_ITEM ( )  RATIONAL_B_SPLINE_SURFACE ( (
 ( 1.000000000000000000, 1.000000000000000000),
 ( 0.9934239774497838349, 0.8357310067453913582),
 ( 0.9934239774497838349, 0.8357310067453913582),
 ( 1.000000000000000000, 1.000000000000000000) ) ) 
 REPRESENTATION_ITEM ( '' )  SURFACE ( )  );
#19538 = CARTESIAN_POINT ( 'NONE',  ( 109.1721716018069515, 0.01368917435590588996, 0.01019541462303041185 ) ) ;
#19539 = EDGE_LOOP ( 'NONE', ( #23476, #3682, #16341, #16172 ) ) ;
#19540 = CARTESIAN_POINT ( 'NONE',  ( -4.473127245936431073, -12.17046501147550153, -47.80062405537796622 ) ) ;
#19541 = CARTESIAN_POINT ( 'NONE',  ( -15.02187109954783750, -6.234056423739195552, 45.93032478317469725 ) ) ;
#19542 = ORIENTED_EDGE ( 'NONE', *, *, #25561, .T. ) ;
#19543 = CARTESIAN_POINT ( 'NONE',  ( 25.64699802086723679, 97.90265915240027539, 56.24956056770054147 ) ) ;
#19544 = DIRECTION ( 'NONE',  ( -1.000000000000000000, -0.000000000000000000, -0.000000000000000000 ) ) ;
#19545 = CARTESIAN_POINT ( 'NONE',  ( -1.539760825549691958, 35.94320866319490193, -29.16712717142773315 ) ) ;
#19546 = CARTESIAN_POINT ( 'NONE',  ( 26.11404676487257603, -10.71016160607490875, -112.7148551500681606 ) ) ;
#19547 = CARTESIAN_POINT ( 'NONE',  ( -8.786685647604931759, 47.14957014837394667, 25.35688121747446999 ) ) ;
#19548 = CARTESIAN_POINT ( 'NONE',  ( -1.045287976400351981, 36.12803364096590997, -28.14015102489844011 ) ) ;
#19549 = CARTESIAN_POINT ( 'NONE',  ( 1.833721034905622549, -132.4192200895886629, 59.34646046113731899 ) ) ;
#19550 = CARTESIAN_POINT ( 'NONE',  ( 25.81918753295379076, 110.7464580477338245, 22.58534689649710003 ) ) ;
#19551 = FACE_OUTER_BOUND ( 'NONE', #20380, .T. ) ;
#19552 = DIRECTION ( 'NONE',  ( -0.5946245182733607137, 0.1642747008466300118, -0.7870422510449638365 ) ) ;
#19553 = CARTESIAN_POINT ( 'NONE',  ( -8.259864102781676820, 22.52209142945002895, 47.98931516265572128 ) ) ;
#19554 = VERTEX_POINT ( 'NONE', #18649 ) ;
#19555 = EDGE_CURVE ( 'NONE', #19834, #28309, #25754, .T. ) ;
#19556 = ORIENTED_EDGE ( 'NONE', *, *, #11904, .T. ) ;
#19557 = CARTESIAN_POINT ( 'NONE',  ( -8.786685647604887350, 53.04920435127183254, -7.199674155859138835 ) ) ;
#19558 = CARTESIAN_POINT ( 'NONE',  ( 55.49584447822657296, 58.53775398922257978, 42.86099773636560428 ) ) ;
#19559 = CARTESIAN_POINT ( 'NONE',  ( 1.832998868059858122, 144.3700883710216942, 14.63705790014056163 ) ) ;
#19560 = CARTESIAN_POINT ( 'NONE',  ( 109.1589550718174877, 0.0002241941239240469565, -0.007571935245604908930 ) ) ;
#19561 = CARTESIAN_POINT ( 'NONE',  ( 25.87036335909424878, -92.04585932622728706, -65.65170964736225301 ) ) ;
#19562 = DIRECTION ( 'NONE',  ( -0.5914120900931443270, 0.4804373588864766509, 0.6476200150380201359 ) ) ;
#19563 = CARTESIAN_POINT ( 'NONE',  ( -7.078251931573406708, -50.86685171665420313, -11.16394717458656949 ) ) ;
#19564 = ORIENTED_EDGE ( 'NONE', *, *, #27579, .F. ) ;
#19565 = CARTESIAN_POINT ( 'NONE',  ( 1.833485406944043827, 132.3460930279890704, 59.50871042846269177 ) ) ;
#19566 = CARTESIAN_POINT ( 'NONE',  ( -5.986830583229484581, -11.27873876172107437, 49.46736940480268174 ) ) ;
#19567 = DIRECTION ( 'NONE',  ( 0.000000000000000000, 5.223019709707975211E-21, -1.000000000000000000 ) ) ;
#19568 = EDGE_CURVE ( 'NONE', #27747, #7819, #12931, .T. ) ;
#19569 = B_SPLINE_CURVE_WITH_KNOTS ( 'NONE', 3,
 ( #6501, #15250, #8945, #24069, #9076, #4330, #22025, #17277 ),
 .UNSPECIFIED., .F., .F.,
 ( 4, 2, 2, 4 ),
 ( 2.193594746808674791E-16, 0.002761568181852864200, 0.005523136363705508957, 0.01104627272741079240 ),
 .UNSPECIFIED. ) ;
#19570 = B_SPLINE_CURVE_WITH_KNOTS ( 'NONE', 3,
 ( #4287, #8477, #19134, #4003, #12643, #1833 ),
 .UNSPECIFIED., .F., .F.,
 ( 4, 2, 4 ),
 ( 0.000000000000000000, 0.0006311571484586011270, 0.001262314296917202037 ),
 .UNSPECIFIED. ) ;
#19571 = CARTESIAN_POINT ( 'NONE',  ( 26.11404676487257603, 47.08215554553657256, -102.9690087468796662 ) ) ;
#19572 = EDGE_CURVE ( 'NONE', #23418, #9221, #10449, .T. ) ;
#19573 = PRODUCT_DEFINITION_SHAPE ( 'NONE', 'NONE',  #9653 ) ;
#19574 = EDGE_LOOP ( 'NONE', ( #4455, #13836, #17282, #19791 ) ) ;
#19575 = CARTESIAN_POINT ( 'NONE',  ( 1.833485406944057594, -45.34878176254139248, -137.8414413349090637 ) ) ;
#19576 = ORIENTED_EDGE ( 'NONE', *, *, #4993, .T. ) ;
#19577 = ORIENTED_EDGE ( 'NONE', *, *, #21460, .F. ) ;
#19578 = VERTEX_POINT ( 'NONE', #8023 ) ;
#19579 = B_SPLINE_CURVE_WITH_KNOTS ( 'NONE', 3,
 ( #23676, #3792, #8667, #24085, #21486, #21910 ),
 .UNSPECIFIED., .F., .F.,
 ( 4, 2, 4 ),
 ( 1.965608005753612659E-17, 0.0006311571484586143543, 0.001262314296917209193 ),
 .UNSPECIFIED. ) ;
#19580 = DIRECTION ( 'NONE',  ( -0.5914120900931443270, -0.09226095020377388101, -0.8010740644654246179 ) ) ;
#19581 =( BOUNDED_SURFACE ( )  B_SPLINE_SURFACE ( 3, 1, ( 
 ( #2362, #19641 ),
 ( #6852, #10882 ),
 ( #19939, #9011 ),
 ( #8715, #17771 ) ),
 .UNSPECIFIED., .F., .F., .F. ) 
 B_SPLINE_SURFACE_WITH_KNOTS ( ( 4, 4 ),
 ( 2, 2 ),
 ( 0.000000000000000000, 1.000000000000000000 ),
 ( 0.000000000000000000, 1.000000000000000000 ),
 .UNSPECIFIED. ) 
 GEOMETRIC_REPRESENTATION_ITEM ( )  RATIONAL_B_SPLINE_SURFACE ( (
 ( 1.000000000000000000, 1.000000000000000000),
 ( 0.7789835883360576307, 0.9689951854195403280),
 ( 0.7789835883360576307, 0.9689951854195403280),
 ( 1.000000000000000000, 1.000000000000000000) ) ) 
 REPRESENTATION_ITEM ( '' )  SURFACE ( )  );
#19582 = CARTESIAN_POINT ( 'NONE',  ( -25.21435515916044423, -16.39063784838720395, 30.48034229288656505 ) ) ;
#19583 = CARTESIAN_POINT ( 'NONE',  ( 109.1624594426973118, -0.009004164758064462162, 0.01318243916935004680 ) ) ;
#19584 = CARTESIAN_POINT ( 'NONE',  ( -10.86508079875781618, 35.35100740321776414, -36.95527278096538737 ) ) ;
#19585 = ORIENTED_EDGE ( 'NONE', *, *, #26378, .F. ) ;
#19586 = EDGE_CURVE ( 'NONE', #12242, #5301, #1367, .T. ) ;
#19587 = ORIENTED_EDGE ( 'NONE', *, *, #4816, .F. ) ;
#19588 = CARTESIAN_POINT ( 'NONE',  ( -1.045287976400362417, -44.00138577190658395, -12.68782741917276446 ) ) ;
#19589 = EDGE_CURVE ( 'NONE', #142, #21070, #9284, .T. ) ;
#19590 = CARTESIAN_POINT ( 'NONE',  ( -28.13707043255157103, 21.52861750560949972, 7.802116958608778852 ) ) ;
#19591 = CARTESIAN_POINT ( 'NONE',  ( 109.1778270068192853, 0.007323887274081532055, -0.005755170886745342509 ) ) ;
#19592 = CARTESIAN_POINT ( 'NONE',  ( -55.24198130335446422, -0.008310594958150379491, -0.004163123460805868634 ) ) ;
#19593 = CARTESIAN_POINT ( 'NONE',  ( 2.430230287190572103, -84.35270093935176305, -118.5711603495689985 ) ) ;
#19594 = CARTESIAN_POINT ( 'NONE',  ( -1.048171036023500369, -27.73816396939538009, 36.44209502233739073 ) ) ;
#19595 = EDGE_CURVE ( 'NONE', #17548, #16728, #9264, .T. ) ;
#19596 = CARTESIAN_POINT ( 'NONE',  ( 109.1586900883932856, -0.005236795036868193212, -0.004851151255031836522 ) ) ;
#19597 = DIRECTION ( 'NONE',  ( 0.000000000000000000, 0.000000000000000000, -1.000000000000000000 ) ) ;
#19598 = CARTESIAN_POINT ( 'NONE',  ( 2.430230287190592531, 71.49654683843687053, -126.7388733285337281 ) ) ;
#19599 = EDGE_CURVE ( 'NONE', #14920, #18597, #23728, .T. ) ;
#19600 = ORIENTED_EDGE ( 'NONE', *, *, #4676, .F. ) ;
#19601 = ORIENTED_EDGE ( 'NONE', *, *, #1306, .T. ) ;
#19602 = CARTESIAN_POINT ( 'NONE',  ( 109.1586900883932856, 0.0006456433529162510171, 0.007109207791181754860 ) ) ;
#19603 = VERTEX_POINT ( 'NONE', #23704 ) ;
#19604 = EDGE_LOOP ( 'NONE', ( #16736, #24885, #16641, #14721 ) ) ;
#19605 = ORIENTED_EDGE ( 'NONE', *, *, #15192, .T. ) ;
#19606 = CARTESIAN_POINT ( 'NONE',  ( 32.73300124599732186, 0.000000000000000000, 0.000000000000000000 ) ) ;
#19607 = CARTESIAN_POINT ( 'NONE',  ( -90.83090735639699176, 0.000000000000000000, 0.000000000000000000 ) ) ;
#19608 =( BOUNDED_SURFACE ( )  B_SPLINE_SURFACE ( 3, 1, ( 
 ( #20017, #19593 ),
 ( #15689, #26210 ),
 ( #11245, #17847 ),
 ( #2299, #26628 ) ),
 .UNSPECIFIED., .F., .F., .F. ) 
 B_SPLINE_SURFACE_WITH_KNOTS ( ( 4, 4 ),
 ( 2, 2 ),
 ( 0.000000000000000000, 1.000000000000000000 ),
 ( 0.000000000000000000, 1.000000000000000000 ),
 .UNSPECIFIED. ) 
 GEOMETRIC_REPRESENTATION_ITEM ( )  RATIONAL_B_SPLINE_SURFACE ( (
 ( 1.000000000000000000, 1.000000000000000000),
 ( 0.6386103224230302855, 0.9954351624131538845),
 ( 0.6386103224230302855, 0.9954351624131538845),
 ( 1.000000000000000000, 1.000000000000000000) ) ) 
 REPRESENTATION_ITEM ( '' )  SURFACE ( )  );
#19609 = CARTESIAN_POINT ( 'NONE',  ( 25.65782528836481546, -83.52701600504825308, -75.98558751977860481 ) ) ;
#19610 = CARTESIAN_POINT ( 'NONE',  ( -8.786685647604890903, -53.04920435127188938, -7.199674155858766689 ) ) ;
#19611 = B_SPLINE_CURVE_WITH_KNOTS ( 'NONE', 3,
 ( #8836, #190, #20042, #17596, #6682, #4495, #1195 ),
 .UNSPECIFIED., .F., .F.,
 ( 4, 3, 4 ),
 ( 5.852680391678861476E-16, 0.02816610861753249262, 0.04000277880656273599 ),
 .UNSPECIFIED. ) ;
#19612 = CARTESIAN_POINT ( 'NONE',  ( -55.24271866751342941, 0.008488649505346579707, -0.004256484107793386679 ) ) ;
#19613 = CARTESIAN_POINT ( 'NONE',  ( 55.79472521941428198, 30.25520714117905996, 66.16469064668309841 ) ) ;
#19614 = CARTESIAN_POINT ( 'NONE',  ( -12.94347594948484037, 48.30328466416762723, 6.555928820869474372 ) ) ;
#19615 = EDGE_CURVE ( 'NONE', #13110, #15665, #1365, .T. ) ;
#19616 = CARTESIAN_POINT ( 'NONE',  ( 25.64708228042118421, -110.4520805602537337, 23.43704872438724962 ) ) ;
#19617 = CARTESIAN_POINT ( 'NONE',  ( -21.81686047589431965, 5.181745222995449929, -38.17230180719251820 ) ) ;
#19619 = ORIENTED_EDGE ( 'NONE', *, *, #16694, .T. ) ;
#19618 = EDGE_CURVE ( 'NONE', #10231, #2725, #18182, .T. ) ;
#19620 = ORIENTED_EDGE ( 'NONE', *, *, #15796, .T. ) ;
#19621 = CARTESIAN_POINT ( 'NONE',  ( -1.056502255334264895, 36.75727364034733569, -27.33667001641181926 ) ) ;
#19622 = DIRECTION ( 'NONE',  ( 0.000000000000000000, 0.000000000000000000, 1.000000000000000000 ) ) ;
#19623 = CARTESIAN_POINT ( 'NONE',  ( -20.47566262905010603, 10.72601569609896366, -27.87687924095551750 ) ) ;
#19624 = CARTESIAN_POINT ( 'NONE',  ( -1.259920593601971950, -43.01175804832021043, -16.33409644610535594 ) ) ;
#19625 = CARTESIAN_POINT ( 'NONE',  ( -1.539760825549691958, 35.94320866319490193, -29.16712717142773315 ) ) ;
#19626 = ORIENTED_EDGE ( 'NONE', *, *, #5810, .T. ) ;
#19627 = CARTESIAN_POINT ( 'NONE',  ( -55.24390624410018802, 0.001811362924359719581, 0.01027195578987765215 ) ) ;
#19628 = CARTESIAN_POINT ( 'NONE',  ( 1.833206308920080740, -144.2348261777515006, -15.90849808442029101 ) ) ;
#19629 = CARTESIAN_POINT ( 'NONE',  ( -1.048994561756799060, -26.29622118251707619, -37.49601524795400564 ) ) ;
#19630 = ORIENTED_EDGE ( 'NONE', *, *, #14828, .F. ) ;
#19631 = ORIENTED_EDGE ( 'NONE', *, *, #22480, .T. ) ;
#19632 = LINE ( 'NONE', #22239, #1103 ) ;
#19634 = ORIENTED_EDGE ( 'NONE', *, *, #16799, .F. ) ;
#19633 = B_SPLINE_CURVE_WITH_KNOTS ( 'NONE', 3,
 ( #14174, #21085, #16060, #3256, #18652, #24860 ),
 .UNSPECIFIED., .F., .F.,
 ( 4, 2, 4 ),
 ( 3.467809420226820728E-16, 0.003576372551511154425, 0.007152745103021954098 ),
 .UNSPECIFIED. ) ;
#19635 = ORIENTED_EDGE ( 'NONE', *, *, #25233, .T. ) ;
#19636 = FACE_OUTER_BOUND ( 'NONE', #16678, .T. ) ;
#19637 = EDGE_LOOP ( 'NONE', ( #26450, #6930, #8470, #5884 ) ) ;
#19638 = CARTESIAN_POINT ( 'NONE',  ( 8.186469829614237526, -77.65916164626425200, 127.5731248499974129 ) ) ;
#19639 = CARTESIAN_POINT ( 'NONE',  ( 6.224689322667630975, -48.18553814190126872, 139.9988794244330563 ) ) ;
#19640 = CARTESIAN_POINT ( 'NONE',  ( 13.36082413113061307, -70.90215303572030336, -135.4964217943314679 ) ) ;
#19641 = CARTESIAN_POINT ( 'NONE',  ( -1.583189561560253589, -38.94740041318312507, -25.21827308671218049 ) ) ;
#19642 = CARTESIAN_POINT ( 'NONE',  ( 25.64670758986457599, 56.02376616805423026, 98.03181353150503696 ) ) ;
#19643 = CARTESIAN_POINT ( 'NONE',  ( 16.75465622695657686, -10.24707101927944031, -141.8562168210794994 ) ) ;
#19644 = B_SPLINE_CURVE_WITH_KNOTS ( 'NONE', 3,
 ( #19914, #11001, #6396, #8846 ),
 .UNSPECIFIED., .F., .F.,
 ( 4, 4 ),
 ( 0.000000000000000000, 0.01077107196513851436 ),
 .UNSPECIFIED. ) ;
#19645 = EDGE_CURVE ( 'NONE', #25619, #17840, #12033, .T. ) ;
#19646 = CARTESIAN_POINT ( 'NONE',  ( 25.98552792386801613, -103.7897946223262693, -45.02923844025588096 ) ) ;
#19648 = CARTESIAN_POINT ( 'NONE',  ( 2.108393763691148948, -118.2927144690665102, 84.36147263237538141 ) ) ;
#19647 = CARTESIAN_POINT ( 'NONE',  ( 1.833838850093517658, 1.769966374633376447E-14, 145.1097630783160923 ) ) ;
#19649 = DIRECTION ( 'NONE',  ( -1.000000000000000000, -0.000000000000000000, -0.000000000000000000 ) ) ;
#19651 = ORIENTED_EDGE ( 'NONE', *, *, #5803, .T. ) ;
#19650 = ADVANCED_FACE ( 'NONE', ( #57 ), #27656, .T. ) ;
#19652 = CARTESIAN_POINT ( 'NONE',  ( 8.186469829614399174, -12.15801983495520133, -148.8557359502364079 ) ) ;
#19653 = CARTESIAN_POINT ( 'NONE',  ( 2.430230287190589422, -86.70145658344578976, -116.8646894862420993 ) ) ;
#19654 = CARTESIAN_POINT ( 'NONE',  ( -1.048172774974295285, -26.08722459372758706, 37.64158596421241043 ) ) ;
#19655 = ADVANCED_FACE ( 'NONE', ( #13013 ), #13649, .F. ) ;
#19656 = CARTESIAN_POINT ( 'NONE',  ( 10.93730112725969938, 71.28103789254939215, 133.3192575531800799 ) ) ;
#19657 = CARTESIAN_POINT ( 'NONE',  ( 28.37644542392850511, 122.4011828058666538, -21.87158679436075204 ) ) ;
#19658 = CARTESIAN_POINT ( 'NONE',  ( -7.733045908741340568, 21.80378472388487054, -47.75066202881800592 ) ) ;
#19659 =( BOUNDED_SURFACE ( )  B_SPLINE_SURFACE ( 3, 1, ( 
 ( #13322, #19667 ),
 ( #21841, #4412 ),
 ( #15199, #26155 ),
 ( #373, #19536 ) ),
 .UNSPECIFIED., .F., .F., .F. ) 
 B_SPLINE_SURFACE_WITH_KNOTS ( ( 4, 4 ),
 ( 2, 2 ),
 ( 0.000000000000000000, 1.000000000000000000 ),
 ( 0.000000000000000000, 1.000000000000000000 ),
 .UNSPECIFIED. ) 
 GEOMETRIC_REPRESENTATION_ITEM ( )  RATIONAL_B_SPLINE_SURFACE ( (
 ( 1.000000000000000000, 1.000000000000000000),
 ( 0.9956975270656955868, 0.8568959468854907557),
 ( 0.9956975270656955868, 0.8568959468854907557),
 ( 1.000000000000000000, 1.000000000000000000) ) ) 
 REPRESENTATION_ITEM ( '' )  SURFACE ( )  );
#19660 = ORIENTED_EDGE ( 'NONE', *, *, #23655, .F. ) ;
#19661 = CARTESIAN_POINT ( 'NONE',  ( -1.045287976400365970, 15.59869763335068171, -43.05558670614252037 ) ) ;
#19662 = CARTESIAN_POINT ( 'NONE',  ( -1.619063947482197729, 25.20140673341430571, 38.92136151114879539 ) ) ;
#19663 = CARTESIAN_POINT ( 'NONE',  ( -8.786685647604885574, 6.096987947571466530E-17, -1.524246986892866633E-17 ) ) ;
#19664 = CARTESIAN_POINT ( 'NONE',  ( -55.24300891470650754, 0.008142823778062566187, 0.005486913146700293786 ) ) ;
#19665 = CARTESIAN_POINT ( 'NONE',  ( 1.833838850093452599, 117.3962664098823439, 85.29337590730578711 ) ) ;
#19666 = ORIENTED_EDGE ( 'NONE', *, *, #20094, .F. ) ;
#19667 = CARTESIAN_POINT ( 'NONE',  ( 1.832998868059858122, 29.64765804470072652, 142.0492247521723925 ) ) ;
#19668 = CARTESIAN_POINT ( 'NONE',  ( 109.1592201516379674, 0.007566779963325568660, 0.002134489919768169444 ) ) ;
#19669 = ORIENTED_EDGE ( 'NONE', *, *, #23124, .F. ) ;
#19670 = CARTESIAN_POINT ( 'NONE',  ( -25.21435515916043357, -15.02493970636125198, 31.17620025257602379 ) ) ;
#19671 = ORIENTED_EDGE ( 'NONE', *, *, #1572, .F. ) ;
#19672 = CARTESIAN_POINT ( 'NONE',  ( -1.323830074806774837, -35.86387698262934265, -28.92190886481852274 ) ) ;
#19673 = CARTESIAN_POINT ( 'NONE',  ( 10.93730112725996229, -20.69552240458240888, -149.7554878793151545 ) ) ;
#19674 = ORIENTED_EDGE ( 'NONE', *, *, #4502, .F. ) ;
#19675 = DIRECTION ( 'NONE',  ( 1.000000000000000000, -6.938893903907226837E-18, 1.734723475976806709E-18 ) ) ;
#19676 = EDGE_CURVE ( 'NONE', #14235, #9093, #4113, .T. ) ;
#19677 = DIRECTION ( 'NONE',  ( -0.5914120900931443270, 0.008020494142996235920, 0.8063295922669343474 ) ) ;
#19678 = DIRECTION ( 'NONE',  ( 0.000000000000000000, 6.938893903907228378E-16, 1.000000000000000000 ) ) ;
#19679 = CARTESIAN_POINT ( 'NONE',  ( 25.64681081121879203, 23.06870491922322230, 110.5293738517609228 ) ) ;
#19680 = FACE_OUTER_BOUND ( 'NONE', #11329, .T. ) ;
#19681 = EDGE_CURVE ( 'NONE', #27586, #28027, #11676, .T. ) ;
#19682 = DIRECTION ( 'NONE',  ( -0.7563875759206389882, 0.03500244528123006016, 0.6531865459554675457 ) ) ;
#19683 = CARTESIAN_POINT ( 'NONE',  ( -20.21097721650786738, -24.14932365326965069, -17.13687097598128517 ) ) ;
#19684 = CARTESIAN_POINT ( 'NONE',  ( 32.73300124599732186, 0.000000000000000000, 0.000000000000000000 ) ) ;
#19685 = AXIS2_PLACEMENT_3D ( 'NONE', #5266, #16642, #26986 ) ;
#19686 = CARTESIAN_POINT ( 'NONE',  ( 28.37644542392829194, -105.5967537682339525, -65.64862111872180606 ) ) ;
#19687 = EDGE_LOOP ( 'NONE', ( #23848, #13259, #4998, #14522 ) ) ;
#19688 = ORIENTED_EDGE ( 'NONE', *, *, #2151, .T. ) ;
#19689 = ORIENTED_EDGE ( 'NONE', *, *, #4641, .T. ) ;
#19690 = CARTESIAN_POINT ( 'NONE',  ( 25.64700659047695552, 103.0567718204601846, 46.13293552475826687 ) ) ;
#19691 = CARTESIAN_POINT ( 'NONE',  ( -20.90916690077966322, 35.64494649500682755, -17.17795951644668762 ) ) ;
#19693 = DIRECTION ( 'NONE',  ( 1.000000000000000000, -6.938893903907226837E-18, 1.734723475976806709E-18 ) ) ;
#19692 = CARTESIAN_POINT ( 'NONE',  ( 2.108985857320929025, 98.16869034643305270, 107.1123114102931595 ) ) ;
#19694 = CARTESIAN_POINT ( 'NONE',  ( 2.430230287190592531, -138.8342928068217077, -43.58368230469531568 ) ) ;
#19695 = CARTESIAN_POINT ( 'NONE',  ( -1.539763995773681282, 43.19716353142356269, 16.63252574782999460 ) ) ;
#19696 = CARTESIAN_POINT ( 'NONE',  ( 8.186469829614374305, -42.84118568057105847, -143.0750865143072588 ) ) ;
#19697 = CARTESIAN_POINT ( 'NONE',  ( -1.050229599974477734, 27.12684363859256109, -36.90196321294305193 ) ) ;
#19698 = ORIENTED_EDGE ( 'NONE', *, *, #25949, .F. ) ;
#19699 = CARTESIAN_POINT ( 'NONE',  ( 1.894214914920919757, 31.11059045489134789, 141.7768822502887929 ) ) ;
#19700 = CARTESIAN_POINT ( 'NONE',  ( -7.078251931573400491, -50.86685171665403260, 11.16394717458729957 ) ) ;
#19701 =( BOUNDED_SURFACE ( )  B_SPLINE_SURFACE ( 3, 1, ( 
 ( #24453, #13773 ),
 ( #11338, #9610 ),
 ( #396, #7041 ),
 ( #24607, #16078 ) ),
 .UNSPECIFIED., .F., .F., .F. ) 
 B_SPLINE_SURFACE_WITH_KNOTS ( ( 4, 4 ),
 ( 2, 2 ),
 ( 0.000000000000000000, 1.000000000000000000 ),
 ( 0.000000000000000000, 1.000000000000000000 ),
 .UNSPECIFIED. ) 
 GEOMETRIC_REPRESENTATION_ITEM ( )  RATIONAL_B_SPLINE_SURFACE ( (
 ( 1.000000000000000000, 1.000000000000000000),
 ( 0.9934239774497837239, 0.8357310067453919133),
 ( 0.9934239774497837239, 0.8357310067453919133),
 ( 1.000000000000000000, 1.000000000000000000) ) ) 
 REPRESENTATION_ITEM ( '' )  SURFACE ( )  );
#19702 = CARTESIAN_POINT ( 'NONE',  ( -19.53423201713129842, 1.355459634611817431E-16, -3.388649086529543578E-17 ) ) ;
#19703 = DIRECTION ( 'NONE',  ( -0.5914120900931443270, -0.5335794202785262286, 0.6045864222316693626 ) ) ;
#19704 = B_SPLINE_CURVE_WITH_KNOTS ( 'NONE', 3,
 ( #15278, #21919, #24373, #11126, #22358, #2177, #4358, #10986, #19746, #8971 ),
 .UNSPECIFIED., .F., .F.,
 ( 4, 2, 2, 2, 4 ),
 ( 2.884421207865725401E-16, 0.0003346187017559067080, 0.0006692374035115243678, 0.001003856105267142028, 0.001338474807022759687 ),
 .UNSPECIFIED. ) ;
#19705 = B_SPLINE_CURVE_WITH_KNOTS ( 'NONE', 3,
 ( #8306, #18813, #21103, #10469 ),
 .UNSPECIFIED., .F., .F.,
 ( 4, 4 ),
 ( 1.892757412642747523E-16, 0.001982023823822947652 ),
 .UNSPECIFIED. ) ;
#19706 = ORIENTED_EDGE ( 'NONE', *, *, #18220, .T. ) ;
#19707 = CARTESIAN_POINT ( 'NONE',  ( -10.86508079875781618, 50.67624451685635734, 6.877801422380954044 ) ) ;
#19708 = CARTESIAN_POINT ( 'NONE',  ( 2.430230287190589422, 43.58368230469574911, -138.8342928068215656 ) ) ;
#19709 = ORIENTED_EDGE ( 'NONE', *, *, #10988, .F. ) ;
#19710 = B_SPLINE_CURVE_WITH_KNOTS ( 'NONE', 3,
 ( #24846, #9441, #13738, #27116, #2812, #15908, #11588 ),
 .UNSPECIFIED., .F., .F.,
 ( 4, 3, 4 ),
 ( 0.000000000000000000, 0.02398743853561358455, 0.04000277880656216700 ),
 .UNSPECIFIED. ) ;
#19711 = EDGE_LOOP ( 'NONE', ( #12378, #20682, #19193, #12700 ) ) ;
#19712 = ORIENTED_EDGE ( 'NONE', *, *, #15067, .F. ) ;
#19713 = CARTESIAN_POINT ( 'NONE',  ( -55.24198130335446422, -0.009170435128244796077, 0.001516807524704069481 ) ) ;
#19714 = CARTESIAN_POINT ( 'NONE',  ( 109.1587776205901861, -0.002904816147412016356, 0.006729130500864200642 ) ) ;
#19715 = ADVANCED_FACE ( 'NONE', ( #22074 ), #2984, .F. ) ;
#19716 = CARTESIAN_POINT ( 'NONE',  ( -2.904412668506665351, 17.42365698954698061, -44.35433137608945486 ) ) ;
#19717 = EDGE_CURVE ( 'NONE', #10457, #9181, #344, .T. ) ;
#19718 = VERTEX_POINT ( 'NONE', #24394 ) ;
#19719 = LINE ( 'NONE', #21892, #10203 ) ;
#19720 = CARTESIAN_POINT ( 'NONE',  ( -1.323830074806773061, -12.01461446423233781, -44.47857376182264488 ) ) ;
#19721 = ORIENTED_EDGE ( 'NONE', *, *, #7823, .F. ) ;
#19722 = CARTESIAN_POINT ( 'NONE',  ( -20.47566262905010603, 10.72601569609896366, -27.87687924095551750 ) ) ;
#19723 = CARTESIAN_POINT ( 'NONE',  ( 1.833809397773840777, 141.9756687985006636, -29.99591688576947845 ) ) ;
#19724 = FACE_OUTER_BOUND ( 'NONE', #16894, .T. ) ;
#19725 = CARTESIAN_POINT ( 'NONE',  ( 5.340103556456518241, -96.93942141425988268, -111.1041836730288708 ) ) ;
#19726 = FACE_OUTER_BOUND ( 'NONE', #21107, .T. ) ;
#19727 = CARTESIAN_POINT ( 'NONE',  ( -20.20612092514784663, 18.30568145913877132, 23.26073121129616439 ) ) ;
#19728 = DIRECTION ( 'NONE',  ( -0.000000000000000000, 1.000000000000000000, -0.000000000000000000 ) ) ;
#19729 = DIRECTION ( 'NONE',  ( 1.000000000000000000, -6.938893903907226837E-18, 1.734723475976806709E-18 ) ) ;
#19730 = CYLINDRICAL_SURFACE ( 'NONE', #21286, 80.00000000000000000 ) ;
#19731 = CARTESIAN_POINT ( 'NONE',  ( 1.834118845439484335, 97.22976650547425947, 107.7186227765457858 ) ) ;
#19732 = ORIENTED_EDGE ( 'NONE', *, *, #23843, .F. ) ;
#19733 = ORIENTED_EDGE ( 'NONE', *, *, #22395, .F. ) ;
#19734 = CARTESIAN_POINT ( 'NONE',  ( 1.833485406944057594, -142.0485807715644171, -29.64752363041688454 ) ) ;
#19735 = CARTESIAN_POINT ( 'NONE',  ( 2.433796855181233454, -84.34988187691011774, 118.5671979538053904 ) ) ;
#19736 = ORIENTED_EDGE ( 'NONE', *, *, #20786, .F. ) ;
#19737 =( BOUNDED_SURFACE ( )  B_SPLINE_SURFACE ( 3, 1, ( 
 ( #10738, #19931 ),
 ( #21132, #15162 ),
 ( #13296, #28404 ),
 ( #24121, #4238 ) ),
 .UNSPECIFIED., .F., .F., .F. ) 
 B_SPLINE_SURFACE_WITH_KNOTS ( ( 4, 4 ),
 ( 2, 2 ),
 ( 0.000000000000000000, 1.000000000000000000 ),
 ( 0.000000000000000000, 1.000000000000000000 ),
 .UNSPECIFIED. ) 
 GEOMETRIC_REPRESENTATION_ITEM ( )  RATIONAL_B_SPLINE_SURFACE ( (
 ( 1.000000000000000000, 1.000000000000000000),
 ( 0.9956975270656954757, 0.8568959468854893125),
 ( 0.9956975270656954757, 0.8568959468854893125),
 ( 1.000000000000000000, 1.000000000000000000) ) ) 
 REPRESENTATION_ITEM ( '' )  SURFACE ( )  );
#19738 = VERTEX_POINT ( 'NONE', #24547 ) ;
#19739 = ORIENTED_EDGE ( 'NONE', *, *, #12808, .F. ) ;
#19740 = EDGE_CURVE ( 'NONE', #17200, #9116, #526, .T. ) ;
#19741 = EDGE_CURVE ( 'NONE', #6430, #6599, #7249, .T. ) ;
#19742 = CARTESIAN_POINT ( 'NONE',  ( 1.833485406944043827, 144.2578170162065021, -15.69895494453236395 ) ) ;
#19743 = EDGE_CURVE ( 'NONE', #4329, #20108, #11716, .T. ) ;
#19744 = B_SPLINE_CURVE_WITH_KNOTS ( 'NONE', 3,
 ( #21405, #19242, #4263, #28015, #10612, #10478, #21965, #15186 ),
 .UNSPECIFIED., .F., .F.,
 ( 4, 2, 2, 4 ),
 ( 0.000000000000000000, 0.0002429592666046696586, 0.0004859185332093393173, 0.0009718370664186723462 ),
 .UNSPECIFIED. ) ;
#19745 = B_SPLINE_CURVE_WITH_KNOTS ( 'NONE', 3,
 ( #11895, #20663, #18080, #377, #19808, #11043, #19961, #2680, #24021, #13476 ),
 .UNSPECIFIED., .F., .F.,
 ( 4, 2, 2, 2, 4 ),
 ( 2.884421207865724908E-16, 0.0003346187017559065996, 0.0006692374035115252352, 0.001003856105267143979, 0.001338474807022762723 ),
 .UNSPECIFIED. ) ;
#19746 = CARTESIAN_POINT ( 'NONE',  ( -1.539763995773684835, -46.22267697748605997, -2.469814354917328370 ) ) ;
#19747 = ADVANCED_FACE ( 'NONE', ( #7128 ), #7023, .F. ) ;
#19748 = CARTESIAN_POINT ( 'NONE',  ( 1.832998868059858122, -142.0492247521724778, 29.64765804470026467 ) ) ;
#19749 = CARTESIAN_POINT ( 'NONE',  ( -1.619063947482197729, 25.20140673341430571, 38.92136151114879539 ) ) ;
#19750 = CARTESIAN_POINT ( 'NONE',  ( -16.86833981943425442, 30.57013526701963713, 31.95666732167528323 ) ) ;
#19751 = DIRECTION ( 'NONE',  ( 0.8320502949607718746, 6.793118186493350437E-17, 0.5547001952908368061 ) ) ;
#19752 = CARTESIAN_POINT ( 'NONE',  ( 1.833485406944043827, 145.1085452359073145, 0.5339064996889848480 ) ) ;
#19753 = CARTESIAN_POINT ( 'NONE',  ( -1.048996300304507523, 36.59642367107745997, -27.53442103413706477 ) ) ;
#19754 = CARTESIAN_POINT ( 'NONE',  ( 1.833838848569429913, -117.2916552720324432, 85.43736077718830302 ) ) ;
#19755 = VERTEX_POINT ( 'NONE', #26668 ) ;
#19756 = ORIENTED_EDGE ( 'NONE', *, *, #19235, .F. ) ;
#19758 = CARTESIAN_POINT ( 'NONE',  ( 2.433796855181205476, 132.3327394885231456, 60.50726454507948660 ) ) ;
#19757 = DIRECTION ( 'NONE',  ( 1.000000000000000000, -6.938893903907226837E-18, 1.734723475976806709E-18 ) ) ;
#19759 = VECTOR ( 'NONE', #19512, 1000.000000000000114 ) ;
#19760 = CARTESIAN_POINT ( 'NONE',  ( -1.463510566862824991, -29.09194585123808707, 35.90603835816536815 ) ) ;
#19761 = CARTESIAN_POINT ( 'NONE',  ( -55.24271866751342941, 0.008433070970614320663, 0.004365563123939306990 ) ) ;
#19762 = CARTESIAN_POINT ( 'NONE',  ( -20.24399999263414429, 10.36954246768245547, -27.76448601145544259 ) ) ;
#19763 = CARTESIAN_POINT ( 'NONE',  ( -2.911734481061404534, -30.23325065583388138, -36.84482841982639911 ) ) ;
#19764 = ORIENTED_EDGE ( 'NONE', *, *, #9436, .F. ) ;
#19765 = CARTESIAN_POINT ( 'NONE',  ( -55.25297051322618813, 0.01306918787467309905, 0.007247191603128975632 ) ) ;
#19766 = ORIENTED_EDGE ( 'NONE', *, *, #7137, .T. ) ;
#19767 = CARTESIAN_POINT ( 'NONE',  ( -5.986830583229481029, 26.01297580803325360, -43.56094206392965873 ) ) ;
#19768 = CARTESIAN_POINT ( 'NONE',  ( -1.050231094221210526, -27.12595454131532691, -36.90262059116457038 ) ) ;
#19769 = ORIENTED_EDGE ( 'NONE', *, *, #10128, .F. ) ;
#19770 = EDGE_LOOP ( 'NONE', ( #12588, #22152, #23727, #5676 ) ) ;
#19771 = CARTESIAN_POINT ( 'NONE',  ( 109.1586059443104944, -0.0004635842312890466835, -0.007058870754606107710 ) ) ;
#19772 = ORIENTED_EDGE ( 'NONE', *, *, #22969, .F. ) ;
#19773 = CARTESIAN_POINT ( 'NONE',  ( -25.21435515916043713, -31.17620025257576799, 15.02493970636179377 ) ) ;
#19774 = VERTEX_POINT ( 'NONE', #481 ) ;
#19775 = EDGE_CURVE ( 'NONE', #6247, #8074, #20625, .T. ) ;
#19776 = CARTESIAN_POINT ( 'NONE',  ( 32.73300124599735028, 72.21147546950551543, 92.86301839380053025 ) ) ;
#19777 = ORIENTED_EDGE ( 'NONE', *, *, #16820, .F. ) ;
#19778 = EDGE_CURVE ( 'NONE', #28093, #11774, #16168, .T. ) ;
#19779 = CIRCLE ( 'NONE', #1847, 34.60786435723138510 ) ;
#19780 = VECTOR ( 'NONE', #6593, 1000.000000000000114 ) ;
#19781 = DIRECTION ( 'NONE',  ( 0.000000000000000000, 5.223019709707975211E-21, -1.000000000000000000 ) ) ;
#19782 = CARTESIAN_POINT ( 'NONE',  ( -1.044556982611274387, -37.98985389331830476, -25.56989963842190150 ) ) ;
#19783 = CIRCLE ( 'NONE', #28064, 37.50000000000001421 ) ;
#19784 = CARTESIAN_POINT ( 'NONE',  ( 109.1721716018069657, 0.01368917435591433980, -0.01019541462303498285 ) ) ;
#19785 = CARTESIAN_POINT ( 'NONE',  ( 1.833206310202335265, 144.2348262833783963, -15.90849712171590902 ) ) ;
#19786 = CARTESIAN_POINT ( 'NONE',  ( 28.37599760073042532, 45.02094138570584647, 105.5302221302108165 ) ) ;
#19787 = B_SPLINE_CURVE_WITH_KNOTS ( 'NONE', 3,
 ( #6299, #12894, #11033, #6435, #24008, #17497, #26283 ),
 .UNSPECIFIED., .F., .F.,
 ( 4, 3, 4 ),
 ( 1.430489624538199204E-17, 0.009512539173626433087, 0.02506242213020844906 ),
 .UNSPECIFIED. ) ;
#19788 = CARTESIAN_POINT ( 'NONE',  ( 25.69398547355838502, -103.4778695380286138, -45.25878216557533307 ) ) ;
#19789 = CARTESIAN_POINT ( 'NONE',  ( -1.259972190295296057, 45.95417440459617353, -2.243354636025928439 ) ) ;
#19790 = CYLINDRICAL_SURFACE ( 'NONE', #17058, 12.50000000000000178 ) ;
#19791 = ORIENTED_EDGE ( 'NONE', *, *, #20573, .F. ) ;
#19792 = CARTESIAN_POINT ( 'NONE',  ( 25.64704443564077252, 56.57116289738743120, -97.71717520928621070 ) ) ;
#19794 = CARTESIAN_POINT ( 'NONE',  ( 25.98107933586719298, 45.01656174308578784, 103.7920584735895346 ) ) ;
#19793 = CARTESIAN_POINT ( 'NONE',  ( -22.23226125620930205, 31.55376588768478285, -2.179935373562563061 ) ) ;
#19795 = CARTESIAN_POINT ( 'NONE',  ( 26.11404676487257603, 65.63269960453364149, -92.25884714080342519 ) ) ;
#19796 = CARTESIAN_POINT ( 'NONE',  ( 32.73300124599738581, 108.9684813982494092, -44.31599526637845798 ) ) ;
#19797 = CARTESIAN_POINT ( 'NONE',  ( -1.323830074806763957, 12.01461446423264690, 44.47857376182257383 ) ) ;
#19798 = CARTESIAN_POINT ( 'NONE',  ( 25.64700659047694487, -34.67498789830372630, -107.4550658295754886 ) ) ;
#19799 = AXIS2_PLACEMENT_3D ( 'NONE', #18314, #16023, #2343 ) ;
#19800 = CARTESIAN_POINT ( 'NONE',  ( 2.063896406836605024, -60.31174178979897960, 132.1577797566303900 ) ) ;
#19801 = CARTESIAN_POINT ( 'NONE',  ( 32.73300124599732186, 0.000000000000000000, 0.000000000000000000 ) ) ;
#19802 = CARTESIAN_POINT ( 'NONE',  ( 21.16825799904902894, 75.99073816868455822, -112.1052598354958008 ) ) ;
#19803 = VECTOR ( 'NONE', #23732, 1000.000000000000000 ) ;
#19804 = VERTEX_POINT ( 'NONE', #4944 ) ;
#19805 = B_SPLINE_CURVE_WITH_KNOTS ( 'NONE', 3,
 ( #3494, #25393, #10135, #27532, #18905, #7990, #16755 ),
 .UNSPECIFIED., .F., .F.,
 ( 4, 3, 4 ),
 ( 8.890457814381136359E-18, 0.0002669560319015655330, 0.0004157520161266013833 ),
 .UNSPECIFIED. ) ;
#19806 = CARTESIAN_POINT ( 'NONE',  ( -9.156249394959713683, -24.29252099376526530, -48.78605533024730789 ) ) ;
#19807 = AXIS2_PLACEMENT_3D ( 'NONE', #4530, #17485, #24569 ) ;
#19808 = CARTESIAN_POINT ( 'NONE',  ( -1.155001620486253877, 45.85729774065937647, 2.068551059060488750 ) ) ;
#19809 = ADVANCED_FACE ( 'NONE', ( #3081 ), #16606, .F. ) ;
#19810 = VERTEX_POINT ( 'NONE', #7555 ) ;
#19811 = CARTESIAN_POINT ( 'NONE',  ( -40.00000000000000000, 0.000000000000000000, 0.000000000000000000 ) ) ;
#19812 = EDGE_CURVE ( 'NONE', #23901, #17967, #24740, .T. ) ;
#19813 = CARTESIAN_POINT ( 'NONE',  ( 30.59138290137872929, 95.58039132682516481, 66.10404757334093517 ) ) ;
#19814 = B_SPLINE_CURVE_WITH_KNOTS ( 'NONE', 3,
 ( #14836, #1598, #28210, #17269, #25787, #6083, #13518, #2429 ),
 .UNSPECIFIED., .F., .F.,
 ( 4, 2, 2, 4 ),
 ( 0.000000000000000000, 0.002761524886576653681, 0.005523049773153307362, 0.01104609954630661472 ),
 .UNSPECIFIED. ) ;
#19815 = LINE ( 'NONE', #6598, #23987 ) ;
#19816 = ORIENTED_EDGE ( 'NONE', *, *, #12468, .F. ) ;
#19817 = EDGE_CURVE ( 'NONE', #9726, #12126, #26091, .T. ) ;
#19818 = CARTESIAN_POINT ( 'NONE',  ( -4.473127245936431073, 49.22197550883368677, 3.196405119333978639 ) ) ;
#19819 = CARTESIAN_POINT ( 'NONE',  ( -1.619063947482201282, 35.99532424477380488, -29.22875152547769062 ) ) ;
#19820 = VECTOR ( 'NONE', #27739, 1000.000000000000000 ) ;
#19821 = CARTESIAN_POINT ( 'NONE',  ( 25.64670758986457955, 46.37945960492014308, -102.9458331681480843 ) ) ;
#19822 = CARTESIAN_POINT ( 'NONE',  ( 2.108985857320901047, -138.5727354014054811, -43.67763756616795945 ) ) ;
#19823 = CARTESIAN_POINT ( 'NONE',  ( 10.93730112725982373, -142.1801301103788262, 51.37919228020236773 ) ) ;
#19824 = CARTESIAN_POINT ( 'NONE',  ( 109.1624594426973260, 0.007576898892904877086, 0.01405141589343896456 ) ) ;
#19825 = AXIS2_PLACEMENT_3D ( 'NONE', #5986, #12582, #1363 ) ;
#19826 = ORIENTED_EDGE ( 'NONE', *, *, #13577, .F. ) ;
#19827 = CARTESIAN_POINT ( 'NONE',  ( 13.36082413113063083, -106.9547846563628042, -109.3026516754243431 ) ) ;
#19828 = DIRECTION ( 'NONE',  ( 0.000000000000000000, 5.223019709708233256E-21, -1.000000000000000000 ) ) ;
#19829 = LINE ( 'NONE', #26311, #13441 ) ;
#19830 = CARTESIAN_POINT ( 'NONE',  ( -1.619063947482197729, 16.67502769180622835, 43.26576862488415287 ) ) ;
#19831 = VERTEX_POINT ( 'NONE', #22378 ) ;
#19832 = CIRCLE ( 'NONE', #10651, 53.53553390275978785 ) ;
#19833 = ORIENTED_EDGE ( 'NONE', *, *, #12675, .T. ) ;
#19834 = VERTEX_POINT ( 'NONE', #14441 ) ;
#19835 = ORIENTED_EDGE ( 'NONE', *, *, #23491, .T. ) ;
#19836 = CARTESIAN_POINT ( 'NONE',  ( -1.046936909428679785, -43.14407378092982981, 15.35929614323710801 ) ) ;
#19837 = CARTESIAN_POINT ( 'NONE',  ( 10.93730112725978287, -136.0306644680987915, 65.95960219663069779 ) ) ;
#19838 = CARTESIAN_POINT ( 'NONE',  ( -6.588769196390751759, -34.04709086065287238, 38.42957692275880532 ) ) ;
#19839 = CARTESIAN_POINT ( 'NONE',  ( -21.81686047589429833, -37.90526371014251339, 6.867757412721077870 ) ) ;
#19840 = DIRECTION ( 'NONE',  ( -1.000000000000000000, -0.000000000000000000, -0.000000000000000000 ) ) ;
#19841 = EDGE_CURVE ( 'NONE', #3526, #21162, #22638, .T. ) ;
#19842 = CARTESIAN_POINT ( 'NONE',  ( -20.20700224038492721, 0.9908225410478516126, -29.58392382092673145 ) ) ;
#19843 = ORIENTED_EDGE ( 'NONE', *, *, #25438, .T. ) ;
#19844 = CARTESIAN_POINT ( 'NONE',  ( -55.24271866751342941, 0.009369360294294836952, -0.001545935011626992572 ) ) ;
#19845 = CARTESIAN_POINT ( 'NONE',  ( -1.583189561560252701, -44.83405390829663872, 11.94859433442948493 ) ) ;
#19846 = CARTESIAN_POINT ( 'NONE',  ( 5.340103556456495149, 75.71042922800717179, -126.5279493230351875 ) ) ;
#19847 = DIRECTION ( 'NONE',  ( 0.5946245182733607137, -0.8039981203473692828, -0.002950380665387635458 ) ) ;
#19848 = B_SPLINE_CURVE_WITH_KNOTS ( 'NONE', 3,
 ( #26448, #8352, #6751, #15495, #1843, #15078, #25908, #6200 ),
 .UNSPECIFIED., .F., .F.,
 ( 4, 2, 2, 4 ),
 ( 0.000000000000000000, 0.0002429592666046706344, 0.0004859185332093412689, 0.0009718370664186825377 ),
 .UNSPECIFIED. ) ;
#19849 = CARTESIAN_POINT ( 'NONE',  ( 1.833206308920097394, 45.54896581797642341, -137.7753864329220619 ) ) ;
#19850 = EDGE_CURVE ( 'NONE', #23016, #12412, #20770, .T. ) ;
#19851 = CARTESIAN_POINT ( 'NONE',  ( 26.28373643307403285, 9.189598927293648245, -127.2291519022770956 ) ) ;
#19852 = CARTESIAN_POINT ( 'NONE',  ( -7.078251931573406708, 26.33626633876224332, -44.92740138729174504 ) ) ;
#19853 = ORIENTED_EDGE ( 'NONE', *, *, #10957, .T. ) ;
#19854 = ADVANCED_FACE ( 'NONE', ( #16458 ), #92, .T. ) ;
#19855 = AXIS2_PLACEMENT_3D ( 'NONE', #11510, #27337, #9507 ) ;
#19856 = EDGE_CURVE ( 'NONE', #21416, #20163, #27098, .T. ) ;
#19857 = ORIENTED_EDGE ( 'NONE', *, *, #253, .T. ) ;
#19858 = EDGE_LOOP ( 'NONE', ( #24206, #2589, #16519, #27613 ) ) ;
#19859 = CIRCLE ( 'NONE', #23566, 151.1787379149930359 ) ;
#19860 = CARTESIAN_POINT ( 'NONE',  ( -55.24198130335446422, -0.009170435128244797812, -0.001516807524708348827 ) ) ;
#19861 = DIRECTION ( 'NONE',  ( -1.000000000000000000, -0.000000000000000000, -0.000000000000000000 ) ) ;
#19862 = B_SPLINE_CURVE_WITH_KNOTS ( 'NONE', 3,
 ( #21253, #1246, #18958, #7609, #25727, #27578 ),
 .UNSPECIFIED., .F., .F.,
 ( 4, 2, 4 ),
 ( 1.536381426628689196E-16, 0.003570751334075638293, 0.007141502668151123064 ),
 .UNSPECIFIED. ) ;
#19863 = ORIENTED_EDGE ( 'NONE', *, *, #11541, .T. ) ;
#19864 = CARTESIAN_POINT ( 'NONE',  ( -20.20700224038492721, -28.44216453106531617, 8.199606986804630182 ) ) ;
#19865 = CARTESIAN_POINT ( 'NONE',  ( -2.265401668238147259, 43.82493763960408728, 17.02144111536834004 ) ) ;
#19866 = ORIENTED_EDGE ( 'NONE', *, *, #24913, .F. ) ;
#19867 = CARTESIAN_POINT ( 'NONE',  ( -1.259972190295307604, -25.19627397134270197, 38.49631882650675152 ) ) ;
#19868 = VERTEX_POINT ( 'NONE', #20916 ) ;
#19869 = CARTESIAN_POINT ( 'NONE',  ( 1.833750490713681458, 141.9939712933758642, -29.90883416717475640 ) ) ;
#19870 = CARTESIAN_POINT ( 'NONE',  ( -55.24390624410018802, -0.007503127514281482044, 0.007245494385991411469 ) ) ;
#19871 = CARTESIAN_POINT ( 'NONE',  ( -1.056502255334264895, -43.40574022158763512, 14.64009593116146846 ) ) ;
#19872 = LINE ( 'NONE', #26074, #5173 ) ;
#19873 = FACE_OUTER_BOUND ( 'NONE', #13279, .T. ) ;
#19874 = VECTOR ( 'NONE', #4562, 1000.000000000000114 ) ;
#19875 = CARTESIAN_POINT ( 'NONE',  ( -20.57838717382308147, 18.89542499756533545, 23.26537097894084383 ) ) ;
#19876 = CARTESIAN_POINT ( 'NONE',  ( -55.24728320129491266, -0.01362040845703352439, -0.005114031043468804730 ) ) ;
#19877 = VECTOR ( 'NONE', #1991, 1000.000000000000000 ) ;
#19878 = B_SPLINE_CURVE_WITH_KNOTS ( 'NONE', 3,
 ( #10669, #4036, #12671, #5933, #28208, #8509, #1730, #23647 ),
 .UNSPECIFIED., .F., .F.,
 ( 4, 2, 2, 4 ),
 ( 2.193594746808674791E-16, 0.002761568181852864200, 0.005523136363705508957, 0.01104627272741079240 ),
 .UNSPECIFIED. ) ;
#19879 = CARTESIAN_POINT ( 'NONE',  ( 1.832998868059890096, 107.4798986104873109, -97.49378069860691198 ) ) ;
#19880 = CARTESIAN_POINT ( 'NONE',  ( -20.20700224038492721, -24.51628800869059432, -16.58740185276701951 ) ) ;
#19881 = FACE_OUTER_BOUND ( 'NONE', #1355, .T. ) ;
#19882 = CARTESIAN_POINT ( 'NONE',  ( -21.41430102051752016, 28.68859753627394582, -11.22990201072285466 ) ) ;
#19883 = CARTESIAN_POINT ( 'NONE',  ( 26.11404676487259024, -1.130420376096339385, -113.2169081140374232 ) ) ;
#19884 = EDGE_CURVE ( 'NONE', #24940, #17233, #27536, .T. ) ;
#19885 = ORIENTED_EDGE ( 'NONE', *, *, #18625, .F. ) ;
#19886 = ADVANCED_FACE ( 'NONE', ( #25397 ), #23422, .F. ) ;
#19887 = EDGE_LOOP ( 'NONE', ( #5253, #16825, #6667, #15032 ) ) ;
#19888 = CARTESIAN_POINT ( 'NONE',  ( -1.259972190295307382, 44.39825172539712383, 12.06706380853646188 ) ) ;
#19889 = FACE_OUTER_BOUND ( 'NONE', #23281, .T. ) ;
#19890 = ORIENTED_EDGE ( 'NONE', *, *, #3434, .T. ) ;
#19891 = EDGE_CURVE ( 'NONE', #20281, #15583, #11013, .T. ) ;
#19892 = VERTEX_POINT ( 'NONE', #7505 ) ;
#19893 = ORIENTED_EDGE ( 'NONE', *, *, #3422, .F. ) ;
#19894 = AXIS2_PLACEMENT_3D ( 'NONE', #6059, #5774, #14813 ) ;
#19895 = CARTESIAN_POINT ( 'NONE',  ( 109.1589550718174877, 0.007270618150629033077, -0.002126635388725490582 ) ) ;
#19896 = VECTOR ( 'NONE', #4699, 1000.000000000000000 ) ;
#19897 = CARTESIAN_POINT ( 'NONE',  ( 109.1589550718175161, -0.007553890059316987690, -0.0005685167901217184081 ) ) ;
#19898 = EDGE_CURVE ( 'NONE', #11599, #10661, #17459, .T. ) ;
#19899 = CARTESIAN_POINT ( 'NONE',  ( -1.045287976400379737, -25.66401692420040703, -37.92705037016734337 ) ) ;
#19900 = CARTESIAN_POINT ( 'NONE',  ( -55.24390624410018802, -0.001451500391950358120, -0.01032895241567008057 ) ) ;
#19901 = CARTESIAN_POINT ( 'NONE',  ( -22.34422965417125795, 33.39267070835848017, 17.95715691811010828 ) ) ;
#19902 = CARTESIAN_POINT ( 'NONE',  ( -25.21435515916043713, 23.92354251275973809, 25.00736669480994934 ) ) ;
#19903 = CARTESIAN_POINT ( 'NONE',  ( 6.224689322667647851, -146.9579047224770818, 18.02516478984095372 ) ) ;
#19904 = CARTESIAN_POINT ( 'NONE',  ( -1.259972190295312267, 12.06706380853692551, -44.39825172539698883 ) ) ;
#19905 = CARTESIAN_POINT ( 'NONE',  ( 13.36082413113061307, -129.1512766091115623, -81.89226687792222492 ) ) ;
#19906 = CARTESIAN_POINT ( 'NONE',  ( -1.048172774974299282, 36.44231470008717366, -27.73787987941021171 ) ) ;
#19907 = CARTESIAN_POINT ( 'NONE',  ( -2.904412668506672457, -2.864640348250298008, 47.56768199507434502 ) ) ;
#19908 = EDGE_CURVE ( 'NONE', #10454, #16841, #649, .T. ) ;
#19909 = ORIENTED_EDGE ( 'NONE', *, *, #17794, .F. ) ;
#19910 = VERTEX_POINT ( 'NONE', #2736 ) ;
#19911 = CARTESIAN_POINT ( 'NONE',  ( 30.59141879584289825, -115.2623358717302295, -14.83090566979546487 ) ) ;
#19912 = CARTESIAN_POINT ( 'NONE',  ( 25.65782528836479770, -22.91156770660721520, -110.5695798068305606 ) ) ;
#19913 = CARTESIAN_POINT ( 'NONE',  ( -20.20700224038492010, -0.9908225410480588913, -29.58392382092672435 ) ) ;
#19914 = CARTESIAN_POINT ( 'NONE',  ( 10.93730112725971715, -20.69552240458431314, 149.7554878793147282 ) ) ;
#19915 = CARTESIAN_POINT ( 'NONE',  ( 25.64681081121879203, -107.2555980796238657, -35.28660243342658731 ) ) ;
#19917 =( BOUNDED_SURFACE ( )  B_SPLINE_SURFACE ( 3, 1, ( 
 ( #2473, #15560 ),
 ( #24372, #20033 ),
 ( #24528, #34 ),
 ( #22357, #15710 ) ),
 .UNSPECIFIED., .F., .F., .F. ) 
 B_SPLINE_SURFACE_WITH_KNOTS ( ( 4, 4 ),
 ( 2, 2 ),
 ( 0.000000000000000000, 1.000000000000000000 ),
 ( 0.000000000000000000, 1.000000000000000000 ),
 .UNSPECIFIED. ) 
 GEOMETRIC_REPRESENTATION_ITEM ( )  RATIONAL_B_SPLINE_SURFACE ( (
 ( 1.000000000000000000, 1.000000000000000000),
 ( 0.9934239774497837239, 0.8357310067453919133),
 ( 0.9934239774497837239, 0.8357310067453919133),
 ( 1.000000000000000000, 1.000000000000000000) ) ) 
 REPRESENTATION_ITEM ( '' )  SURFACE ( )  );
#19916 = VECTOR ( 'NONE', #7118, 1000.000000000000000 ) ;
#19918 = EDGE_LOOP ( 'NONE', ( #12039, #28031 ) ) ;
#19919 = CARTESIAN_POINT ( 'NONE',  ( -1.031422197589711987, -15.60268798220668707, -43.06660437151302290 ) ) ;
#19920 = AXIS2_PLACEMENT_3D ( 'NONE', #14204, #27168, #5748 ) ;
#19921 = ADVANCED_FACE ( 'NONE', ( #20581 ), #11643, .F. ) ;
#19922 = ORIENTED_EDGE ( 'NONE', *, *, #287, .T. ) ;
#19923 = CARTESIAN_POINT ( 'NONE',  ( 2.063896406836605024, 84.29612368209153317, 118.3103904147684631 ) ) ;
#19924 = ORIENTED_EDGE ( 'NONE', *, *, #12549, .F. ) ;
#19925 = B_SPLINE_CURVE_WITH_KNOTS ( 'NONE', 3,
 ( #12367, #23471, #25195, #20871 ),
 .UNSPECIFIED., .F., .F.,
 ( 4, 4 ),
 ( 1.729163450533575901E-16, 0.008383748772659649698 ),
 .UNSPECIFIED. ) ;
#19926 = VERTEX_POINT ( 'NONE', #20146 ) ;
#19927 = B_SPLINE_CURVE_WITH_KNOTS ( 'NONE', 3,
 ( #14523, #16843, #11803, #18848, #14222, #3026, #20994, #27777, #23046, #14380, #11942, #10081, #9942 ),
 .UNSPECIFIED., .F., .F.,
 ( 4, 3, 3, 3, 4 ),
 ( 1.105886215935214523E-17, 0.0007657099931970556828, 0.001531419946797917854, 0.002296279302920152532, 0.003061450627205755497 ),
 .UNSPECIFIED. ) ;
#19928 = DIRECTION ( 'NONE',  ( 0.7071067811865465735, 0.000000000000000000, 0.7071067811865485719 ) ) ;
#19929 = EDGE_CURVE ( 'NONE', #2978, #1180, #11303, .T. ) ;
#19930 = ORIENTED_EDGE ( 'NONE', *, *, #12160, .T. ) ;
#19931 = CARTESIAN_POINT ( 'NONE',  ( 2.430230287190589422, 118.5711603495681459, 84.35270093935295677 ) ) ;
#19932 = ORIENTED_EDGE ( 'NONE', *, *, #18354, .T. ) ;
#19933 = CARTESIAN_POINT ( 'NONE',  ( 109.1592201516379674, 0.005027640251764384401, -0.006044422199831492315 ) ) ;
#19934 = ORIENTED_EDGE ( 'NONE', *, *, #12738, .F. ) ;
#19935 = CARTESIAN_POINT ( 'NONE',  ( 109.1592201516379674, 0.002913740842108636896, 0.007302213399779935825 ) ) ;
#19936 = CARTESIAN_POINT ( 'NONE',  ( -1.050231094221204087, -14.39477892760331024, -43.47885872350351377 ) ) ;
#19937 = CARTESIAN_POINT ( 'NONE',  ( 9.884929003653608603, -50.49804566712222709, 141.8132360130356062 ) ) ;
#19938 = CARTESIAN_POINT ( 'NONE',  ( -24.53239521893646824, 3.868435622621471115, -33.71193723315172264 ) ) ;
#19939 = CARTESIAN_POINT ( 'NONE',  ( -55.25297051322618813, -0.01019003092403672657, 0.01093108995495161231 ) ) ;
#19940 = CARTESIAN_POINT ( 'NONE',  ( 1.832998868059890096, 108.1944082009157455, 96.70023740551157232 ) ) ;
#19941 = B_SPLINE_CURVE_WITH_KNOTS ( 'NONE', 3,
 ( #7253, #18016, #26805, #7115, #11704, #20475, #15872 ),
 .UNSPECIFIED., .F., .F.,
 ( 4, 3, 4 ),
 ( 5.285450785082491170E-16, 0.02816610861753246486, 0.04000277880656266660 ),
 .UNSPECIFIED. ) ;
#19942 = B_SPLINE_CURVE_WITH_KNOTS ( 'NONE', 3,
 ( #26466, #11355, #2869, #6768, #9357, #15515, #24328, #13358 ),
 .UNSPECIFIED., .F., .F.,
 ( 4, 2, 2, 4 ),
 ( 0.000000000000000000, 0.0002429588503611265532, 0.0004859177007222531064, 0.0009718354014444913593 ),
 .UNSPECIFIED. ) ;
#19943 = DIRECTION ( 'NONE',  ( -0.000000000000000000, 1.000000000000000000, 0.000000000000000000 ) ) ;
#19944 = CARTESIAN_POINT ( 'NONE',  ( -25.21435515916043002, -4.655591116594591128, -34.29329011225954105 ) ) ;
#19945 = CARTESIAN_POINT ( 'NONE',  ( 25.64681081121880624, -56.09509703373412748, 97.99105938547904771 ) ) ;
#19946 = ADVANCED_FACE ( 'NONE', ( #433 ), #1143, .F. ) ;
#19947 = ORIENTED_EDGE ( 'NONE', *, *, #4637, .F. ) ;
#19948 = CARTESIAN_POINT ( 'NONE',  ( 1.832998868059858122, 144.3700883710219216, -14.63705790013859875 ) ) ;
#19949 = EDGE_CURVE ( 'NONE', #7747, #5592, #14755, .T. ) ;
#19950 = DIRECTION ( 'NONE',  ( 0.7563875759206388771, 0.5078650950445714463, 0.4122509917856694850 ) ) ;
#19951 = CARTESIAN_POINT ( 'NONE',  ( 109.1592201516379674, 0.006044422199822535938, -0.005027640251767235419 ) ) ;
#19952 = CARTESIAN_POINT ( 'NONE',  ( 25.98552792386799837, 90.89136171349180415, -67.36997957637572654 ) ) ;
#19953 = CARTESIAN_POINT ( 'NONE',  ( 1.833838850855462388, -44.92600961247758562, 137.9800888515322299 ) ) ;
#19954 = EDGE_CURVE ( 'NONE', #4838, #26195, #18713, .T. ) ;
#19955 = CARTESIAN_POINT ( 'NONE',  ( 1.834118845439484335, 145.1099497418795750, -0.1779704863075349530 ) ) ;
#19956 = CARTESIAN_POINT ( 'NONE',  ( -1.019300379054419725, -45.76814864815089123, 2.023851374323154761 ) ) ;
#19957 = CARTESIAN_POINT ( 'NONE',  ( 55.79472521941428198, -66.16469064668319788, 30.25520714117883259 ) ) ;
#19958 = ORIENTED_EDGE ( 'NONE', *, *, #3773, .F. ) ;
#19959 = CARTESIAN_POINT ( 'NONE',  ( -55.25719721206881729, -0.004044147484874425005, 0.01041086141212271658 ) ) ;
#19960 = CARTESIAN_POINT ( 'NONE',  ( 109.1778270068192853, 0.003465086990427089769, 0.008646067828078128972 ) ) ;
#19961 = CARTESIAN_POINT ( 'NONE',  ( -1.323830074806771506, 46.01435746200691312, 2.318057800980871885 ) ) ;
#19962 = ORIENTED_EDGE ( 'NONE', *, *, #3484, .T. ) ;
#19963 = CARTESIAN_POINT ( 'NONE',  ( 25.64692872815577473, -112.9107203549055498, -0.3216598674795657642 ) ) ;
#19964 = DIRECTION ( 'NONE',  ( -0.7637818620346800147, -0.1788995134688828315, 0.6201872550346662072 ) ) ;
#19965 = ORIENTED_EDGE ( 'NONE', *, *, #12440, .T. ) ;
#19966 = CARTESIAN_POINT ( 'NONE',  ( -7.078251931573400491, 11.16394717458747898, 50.86685171665398997 ) ) ;
#19967 = CARTESIAN_POINT ( 'NONE',  ( -1.464342487929859660, -46.14921266389556820, 2.431462367721817230 ) ) ;
#19968 = CARTESIAN_POINT ( 'NONE',  ( 2.433796855181219243, 144.5536872373191670, 16.65276281464612396 ) ) ;
#19969 = CARTESIAN_POINT ( 'NONE',  ( -8.786685647604896232, 9.545808661481343549, 52.67761315067276229 ) ) ;
#19970 = CARTESIAN_POINT ( 'NONE',  ( 25.87036335909427365, -113.0557711752706211, 0.9898498320583746235 ) ) ;
#19971 = VERTEX_POINT ( 'NONE', #23764 ) ;
#19972 = CARTESIAN_POINT ( 'NONE',  ( 25.64681081121879203, -34.49579773461710630, -107.5125461021406181 ) ) ;
#19973 = CARTESIAN_POINT ( 'NONE',  ( 13.36082413113063083, 152.6206443696328563, 9.660980093455210138 ) ) ;
#19974 = DIRECTION ( 'NONE',  ( 1.000000000000000000, -6.938893903907226837E-18, 1.734723475976806709E-18 ) ) ;
#19975 = CARTESIAN_POINT ( 'NONE',  ( 26.11404676487257603, -98.61392875273325842, -55.62948129436350087 ) ) ;
#19976 = ORIENTED_EDGE ( 'NONE', *, *, #99, .T. ) ;
#19977 = ORIENTED_EDGE ( 'NONE', *, *, #24451, .F. ) ;
#19978 = ORIENTED_EDGE ( 'NONE', *, *, #13305, .F. ) ;
#19979 = CARTESIAN_POINT ( 'NONE',  ( -1.049817751779885233, -26.50542916749595435, -37.35030165458165641 ) ) ;
#19980 = FACE_OUTER_BOUND ( 'NONE', #18880, .T. ) ;
#19981 = EDGE_CURVE ( 'NONE', #14674, #27787, #7203, .T. ) ;
#19982 = CARTESIAN_POINT ( 'NONE',  ( -21.41430102051744200, -1.815007301162189446, -30.75470819672111134 ) ) ;
#19983 = CARTESIAN_POINT ( 'NONE',  ( -1.056502255334264895, 36.75727364034733569, -27.33667001641181926 ) ) ;
#19984 = CARTESIAN_POINT ( 'NONE',  ( -20.20700224038492721, -10.08426345511609235, -27.82980252387815767 ) ) ;
#19985 = DIRECTION ( 'NONE',  ( -0.5914120900931443270, -0.8027508043202530308, -0.07630783613001643206 ) ) ;
#19986 = ORIENTED_EDGE ( 'NONE', *, *, #4532, .T. ) ;
#19987 = CARTESIAN_POINT ( 'NONE',  ( 2.263178607246655982, 31.59906277834222266, 141.9207363487295481 ) ) ;
#19988 = CARTESIAN_POINT ( 'NONE',  ( -55.25297051322618813, -0.006313402748431807057, -0.01354497706059512932 ) ) ;
#19989 = CARTESIAN_POINT ( 'NONE',  ( 14.74894986621300319, -1.023413983156987147E-16, 2.558534957892467869E-17 ) ) ;
#19990 = EDGE_CURVE ( 'NONE', #106, #16635, #16708, .T. ) ;
#19991 = EDGE_CURVE ( 'NONE', #22163, #14951, #9571, .T. ) ;
#19992 = ORIENTED_EDGE ( 'NONE', *, *, #3645, .F. ) ;
#19993 = CARTESIAN_POINT ( 'NONE',  ( -1.045287976400365970, -43.05558670614224326, 15.59869763335140469 ) ) ;
#19994 = ORIENTED_EDGE ( 'NONE', *, *, #31, .T. ) ;
#19995 = CARTESIAN_POINT ( 'NONE',  ( -20.20612092514785019, 29.57813644637190365, -1.137292630518160097 ) ) ;
#19996 = CARTESIAN_POINT ( 'NONE',  ( -1.056502255334264895, -14.64009593116132457, -43.40574022158768486 ) ) ;
#19997 = ORIENTED_EDGE ( 'NONE', *, *, #27615, .F. ) ;
#19998 = ORIENTED_EDGE ( 'NONE', *, *, #23883, .T. ) ;
#19999 = ORIENTED_EDGE ( 'NONE', *, *, #10334, .F. ) ;
#20000 = LINE ( 'NONE', #11365, #7771 ) ;
#20001 = CARTESIAN_POINT ( 'NONE',  ( 25.98552792386801968, 84.79516057869876988, 74.89816102339737824 ) ) ;
#20002 = CARTESIAN_POINT ( 'NONE',  ( 8.186469777910533097, 146.7694294853781116, 27.65107827750139435 ) ) ;
#20003 = ORIENTED_EDGE ( 'NONE', *, *, #14754, .F. ) ;
#20004 = CARTESIAN_POINT ( 'NONE',  ( -55.24271866751342941, 0.009388511352198142604, 0.001425019990782173561 ) ) ;
#20005 = CARTESIAN_POINT ( 'NONE',  ( -1.619063947482197729, 43.26576862488456499, 16.67502769180516964 ) ) ;
#20006 = ORIENTED_EDGE ( 'NONE', *, *, #15856, .T. ) ;
#20007 = CARTESIAN_POINT ( 'NONE',  ( -8.786685647604890903, 38.68584556812300690, -37.00619870957947910 ) ) ;
#20008 = ORIENTED_EDGE ( 'NONE', *, *, #8140, .T. ) ;
#20009 = DIRECTION ( 'NONE',  ( -0.7637818620346800147, -0.5345501402766327237, -0.3617919495470695579 ) ) ;
#20010 = B_SPLINE_CURVE_WITH_KNOTS ( 'NONE', 3,
 ( #11419, #3078, #631, #5370 ),
 .UNSPECIFIED., .F., .F.,
 ( 4, 4 ),
 ( 1.734723475976807094E-17, 0.008383560773332731156 ),
 .UNSPECIFIED. ) ;
#20011 = CARTESIAN_POINT ( 'NONE',  ( 25.64704443564079739, -45.80316013050762791, -103.2037466592378507 ) ) ;
#20012 = EDGE_CURVE ( 'NONE', #23708, #25105, #18896, .T. ) ;
#20013 = CARTESIAN_POINT ( 'NONE',  ( -1.619063947482197729, 46.30105812165548684, 2.489035965910320503 ) ) ;
#20014 = FACE_OUTER_BOUND ( 'NONE', #15243, .T. ) ;
#20015 = CARTESIAN_POINT ( 'NONE',  ( 109.1592201516379674, 0.006174480289200316024, 0.004867031887010233454 ) ) ;
#20016 = CARTESIAN_POINT ( 'NONE',  ( 109.1586900883932856, 0.0008465529156635116835, 0.007088091345229658585 ) ) ;
#20017 = CARTESIAN_POINT ( 'NONE',  ( 109.1592201516379674, 0.007302213399787552996, 0.002913740842103208079 ) ) ;
#20018 = CARTESIAN_POINT ( 'NONE',  ( -20.57838717382308147, 16.28767523336121315, -25.16001208503110931 ) ) ;
#20019 = EDGE_CURVE ( 'NONE', #8700, #10668, #8082, .T. ) ;
#20020 = CARTESIAN_POINT ( 'NONE',  ( -40.00000000000000000, 0.000000000000000000, 0.000000000000000000 ) ) ;
#20021 = CARTESIAN_POINT ( 'NONE',  ( 25.73574536432414561, -65.74844932374591622, -91.86645484851379706 ) ) ;
#20022 = CARTESIAN_POINT ( 'NONE',  ( -55.24340739397742084, 0.002421372372454598174, 0.009842732675352095298 ) ) ;
#20023 = CARTESIAN_POINT ( 'NONE',  ( 26.11404676487257603, -10.71016160607644174, 112.7148551500680185 ) ) ;
#20024 = ORIENTED_EDGE ( 'NONE', *, *, #17672, .T. ) ;
#20025 = ORIENTED_EDGE ( 'NONE', *, *, #525, .F. ) ;
#20026 = CARTESIAN_POINT ( 'NONE',  ( -7.078251931573406708, -26.33626633876190937, 44.92740138729193689 ) ) ;
#20027 = ORIENTED_EDGE ( 'NONE', *, *, #17222, .F. ) ;
#20028 = ORIENTED_EDGE ( 'NONE', *, *, #14289, .T. ) ;
#20029 = VERTEX_POINT ( 'NONE', #10380 ) ;
#20030 = DIRECTION ( 'NONE',  ( 0.5946245182733608248, -0.7858154137795719807, -0.1700465163848226269 ) ) ;
#20031 = CARTESIAN_POINT ( 'NONE',  ( -1.050229599974492833, 37.20249516760172526, -26.71319688967646755 ) ) ;
#20032 = B_SPLINE_CURVE_WITH_KNOTS ( 'NONE', 3,
 ( #540, #18371, #9338, #18095, #26873, #27153, #24747 ),
 .UNSPECIFIED., .F., .F.,
 ( 4, 3, 4 ),
 ( 0.000000000000000000, 0.02398743853561372680, 0.04000277880656215312 ),
 .UNSPECIFIED. ) ;
#20033 = CARTESIAN_POINT ( 'NONE',  ( -1.239374126674604337, -44.48112152129338170, 11.92219841463876229 ) ) ;
#20034 = CARTESIAN_POINT ( 'NONE',  ( -1.113548883309547266, -25.34012683631582519, -38.22628252420800976 ) ) ;
#20035 = EDGE_CURVE ( 'NONE', #28149, #19505, #18531, .T. ) ;
#20036 = CARTESIAN_POINT ( 'NONE',  ( -1.049817751779883457, 43.39729912094399822, 14.63752841325003295 ) ) ;
#20037 = ADVANCED_FACE ( 'NONE', ( #17110 ), #3911, .F. ) ;
#20038 = CARTESIAN_POINT ( 'NONE',  ( 1.833206310202335265, -144.3905118062893109, -14.42724831649501560 ) ) ;
#20039 = CARTESIAN_POINT ( 'NONE',  ( 24.01988960052050359, -44.53753990739600255, 123.2441023955617254 ) ) ;
#20040 = CARTESIAN_POINT ( 'NONE',  ( 1.833485406944043827, 108.1939177044938560, -96.69979900902059455 ) ) ;
#20041 = EDGE_CURVE ( 'NONE', #13623, #17999, #13694, .T. ) ;
#20042 = CARTESIAN_POINT ( 'NONE',  ( 21.16825799904898631, -115.0183107335394368, 71.50503315297841311 ) ) ;
#20043 = FACE_OUTER_BOUND ( 'NONE', #18504, .T. ) ;
#20044 = DIRECTION ( 'NONE',  ( 0.000000000000000000, 5.223019709707975211E-21, -1.000000000000000000 ) ) ;
#20045 = VERTEX_POINT ( 'NONE', #17525 ) ;
#20047 = CARTESIAN_POINT ( 'NONE',  ( 28.37599760073042532, -113.9023239246301955, -13.77583212279449398 ) ) ;
#20046 = CARTESIAN_POINT ( 'NONE',  ( 30.59141879584322510, 115.8270959620731873, -9.457572341075218603 ) ) ;
#20048 = CARTESIAN_POINT ( 'NONE',  ( 109.1778270068192853, -0.008646067828078141115, 0.003465086990427058110 ) ) ;
#20049 = CARTESIAN_POINT ( 'NONE',  ( 13.84597867724971998, 90.05293531772780113, -115.8103190066264006 ) ) ;
#20050 = FACE_OUTER_BOUND ( 'NONE', #17853, .T. ) ;
#20051 = CARTESIAN_POINT ( 'NONE',  ( 25.64681081121880624, -56.09509703373412748, 97.99105938547904771 ) ) ;
#20052 = ORIENTED_EDGE ( 'NONE', *, *, #22681, .T. ) ;
#20053 = CARTESIAN_POINT ( 'NONE',  ( 1.833838850093465700, -15.16810397409683198, -144.3148362521193633 ) ) ;
#20054 = ORIENTED_EDGE ( 'NONE', *, *, #525, .T. ) ;
#20055 = DIRECTION ( 'NONE',  ( 1.000000000000000000, -6.938893903907226837E-18, 1.734723475976806709E-18 ) ) ;
#20056 = CARTESIAN_POINT ( 'NONE',  ( 1.833206308920068306, 141.7818018507502416, 30.89799439741674192 ) ) ;
#20057 = ORIENTED_EDGE ( 'NONE', *, *, #28266, .F. ) ;
#20058 = B_SPLINE_CURVE_WITH_KNOTS ( 'NONE', 3,
 ( #2923, #4425, #24033, #17244 ),
 .UNSPECIFIED., .F., .F.,
 ( 4, 4 ),
 ( 0.000000000000000000, 0.008383560773332705135 ),
 .UNSPECIFIED. ) ;
#20059 = VERTEX_POINT ( 'NONE', #19972 ) ;
#20060 = CARTESIAN_POINT ( 'NONE',  ( 28.37603512858445853, 25.60641750873904954, 111.8384105897142859 ) ) ;
#20061 = ORIENTED_EDGE ( 'NONE', *, *, #25296, .T. ) ;
#20062 = CARTESIAN_POINT ( 'NONE',  ( 109.1592201516379674, 0.007566779963325568660, 0.002134489919768169444 ) ) ;
#20063 = ORIENTED_EDGE ( 'NONE', *, *, #25291, .T. ) ;
#20064 = B_SPLINE_CURVE_WITH_KNOTS ( 'NONE', 3,
 ( #19945, #8875, #15464, #24137, #4398, #9015, #21825, #11030, #26551, #4257 ),
 .UNSPECIFIED., .F., .F.,
 ( 4, 3, 3, 4 ),
 ( 6.938893903907228378E-18, 0.0002669560319015819587, 0.0005492286108966481758, 0.0008315040496093573661 ),
 .UNSPECIFIED. ) ;
#20065 = CARTESIAN_POINT ( 'NONE',  ( 109.1586900883932856, 0.006231977675082106191, -0.003481399864227394114 ) ) ;
#20066 = ADVANCED_FACE ( 'NONE', ( #15630 ), #4697, .T. ) ;
#20067 = CARTESIAN_POINT ( 'NONE',  ( 8.186469829614351212, -84.95702201190461267, -122.8338389144555549 ) ) ;
#20068 = EDGE_CURVE ( 'NONE', #25305, #211, #22166, .T. ) ;
#20069 = CARTESIAN_POINT ( 'NONE',  ( -1.239374126674604337, -25.08410696974215170, 38.61989855450968179 ) ) ;
#20070 = CARTESIAN_POINT ( 'NONE',  ( -4.178947244162637631, 47.46809051147737080, 11.88256963646688824 ) ) ;
#20071 = ADVANCED_FACE ( 'NONE', ( #1988 ), #9982, .F. ) ;
#20072 = CARTESIAN_POINT ( 'NONE',  ( 1.833721034905634539, -72.86293192427403653, -125.4904194343092172 ) ) ;
#20073 = CARTESIAN_POINT ( 'NONE',  ( 5.340103556456447187, -62.06990747183774459, 133.7487107983441490 ) ) ;
#20074 = CARTESIAN_POINT ( 'NONE',  ( 30.58324630866351512, 63.85566901681615093, 102.7123253644116829 ) ) ;
#20075 =( BOUNDED_SURFACE ( )  B_SPLINE_SURFACE ( 3, 1, ( 
 ( #5569, #16502 ),
 ( #3408, #14334 ),
 ( #16931, #3832 ),
 ( #27731, #19222 ) ),
 .UNSPECIFIED., .F., .F., .F. ) 
 B_SPLINE_SURFACE_WITH_KNOTS ( ( 4, 4 ),
 ( 2, 2 ),
 ( 0.000000000000000000, 1.000000000000000000 ),
 ( 0.000000000000000000, 1.000000000000000000 ),
 .UNSPECIFIED. ) 
 GEOMETRIC_REPRESENTATION_ITEM ( )  RATIONAL_B_SPLINE_SURFACE ( (
 ( 1.000000000000000000, 1.000000000000000000),
 ( 0.9956975270656954757, 0.8568959468854893125),
 ( 0.9956975270656954757, 0.8568959468854893125),
 ( 1.000000000000000000, 1.000000000000000000) ) ) 
 REPRESENTATION_ITEM ( '' )  SURFACE ( )  );
#20076 = CARTESIAN_POINT ( 'NONE',  ( -1.045287976400365970, 44.00138577190666922, 12.68782741917247670 ) ) ;
#20077 = CARTESIAN_POINT ( 'NONE',  ( -20.24399999263415850, -29.60996018918693551, -1.282322917263360340 ) ) ;
#20078 = FACE_OUTER_BOUND ( 'NONE', #5109, .T. ) ;
#20079 = LINE ( 'NONE', #796, #23056 ) ;
#20080 = CARTESIAN_POINT ( 'NONE',  ( -23.79248802219723302, 33.03370827286732947, -3.207402715357277057 ) ) ;
#20081 = CARTESIAN_POINT ( 'NONE',  ( 25.64681081121879203, -84.18689316040098447, 75.24277141833462679 ) ) ;
#20082 = CARTESIAN_POINT ( 'NONE',  ( 1.834118845439484335, -45.01070051384685655, 137.9527673765103941 ) ) ;
#20083 = CARTESIAN_POINT ( 'NONE',  ( 2.263178607246674190, -125.2099936970372767, 73.90841395012540715 ) ) ;
#20084 = CARTESIAN_POINT ( 'NONE',  ( 1.833485406944043827, -107.4794113447402566, -97.49333871408801144 ) ) ;
#20085 = CARTESIAN_POINT ( 'NONE',  ( 2.063896406836609909, -125.1295119249444241, 73.79559738457707851 ) ) ;
#20086 = DIRECTION ( 'NONE',  ( 0.5946245182733607137, 0.2456431038754758323, 0.7655593692109030624 ) ) ;
#20087 = CARTESIAN_POINT ( 'NONE',  ( 25.64708228042121263, 75.58165863986150157, -83.88307475435979654 ) ) ;
#20088 = VERTEX_POINT ( 'NONE', #9043 ) ;
#20089 = CARTESIAN_POINT ( 'NONE',  ( -8.786685647604706162, -38.68584556812290032, 37.00619870957955015 ) ) ;
#20090 = CARTESIAN_POINT ( 'NONE',  ( -20.57838717382308147, -28.96176188950224528, -7.715628353033566533 ) ) ;
#20091 = CARTESIAN_POINT ( 'NONE',  ( -1.113427685307003534, -35.91272432484637278, 28.52429901637207266 ) ) ;
#20092 = ORIENTED_EDGE ( 'NONE', *, *, #6646, .F. ) ;
#20093 = CARTESIAN_POINT ( 'NONE',  ( 5.340103556456524458, 32.90561046456912919, -143.7310399800114737 ) ) ;
#20094 = EDGE_CURVE ( 'NONE', #4882, #18134, #28182, .T. ) ;
#20095 = ORIENTED_EDGE ( 'NONE', *, *, #17887, .T. ) ;
#20096 = CARTESIAN_POINT ( 'NONE',  ( -24.53237795827027767, -29.54731592868574808, -16.68575684089485023 ) ) ;
#20097 = CARTESIAN_POINT ( 'NONE',  ( -1.019300379054419725, -16.06793277092022976, -42.90269154183422984 ) ) ;
#20098 = EDGE_CURVE ( 'NONE', #11372, #21365, #23005, .T. ) ;
#20099 = VERTEX_POINT ( 'NONE', #6607 ) ;
#20100 = CARTESIAN_POINT ( 'NONE',  ( 2.433796855181219243, -144.8571464219890004, 13.76554153471645847 ) ) ;
#20101 = DIRECTION ( 'NONE',  ( -0.000000000000000000, -1.000000000000000000, -3.122502256758243304E-15 ) ) ;
#20102 = EDGE_CURVE ( 'NONE', #22079, #3709, #17800, .T. ) ;
#20103 = DIRECTION ( 'NONE',  ( -0.5946245182733607137, 0.7858154137795742011, -0.1700465163848121908 ) ) ;
#20104 = B_SPLINE_CURVE_WITH_KNOTS ( 'NONE', 3,
 ( #9291, #18048, #23758, #644, #5529, #10010, #7716 ),
 .UNSPECIFIED., .F., .F.,
 ( 4, 3, 4 ),
 ( 8.845388854693243284E-18, 0.009512539173626379310, 0.02506242213020843518 ),
 .UNSPECIFIED. ) ;
#20105 = CARTESIAN_POINT ( 'NONE',  ( 55.79472521941426777, -28.92526238350430390, -66.75682020267559835 ) ) ;
#20106 = CARTESIAN_POINT ( 'NONE',  ( -1.058197053496171325, 15.81317659443684143, -42.99116279335158453 ) ) ;
#20107 = CARTESIAN_POINT ( 'NONE',  ( 109.1586900883932856, 0.001582822706024251871, -0.006960773163856037206 ) ) ;
#20108 = VERTEX_POINT ( 'NONE', #4427 ) ;
#20109 = EDGE_CURVE ( 'NONE', #23222, #27304, #26393, .T. ) ;
#20110 = CARTESIAN_POINT ( 'NONE',  ( 25.64706015949228046, 0.09919735511166506703, 112.9111942614907491 ) ) ;
#20111 = CARTESIAN_POINT ( 'NONE',  ( 1.833485406944043827, -96.69979900902241354, 108.1939177044922786 ) ) ;
#20112 = DIRECTION ( 'NONE',  ( 0.7563875759206388771, 0.1685564395263429993, 0.6320336713238481341 ) ) ;
#20113 = ORIENTED_EDGE ( 'NONE', *, *, #2945, .T. ) ;
#20114 =( BOUNDED_SURFACE ( )  B_SPLINE_SURFACE ( 3, 1, ( 
 ( #28282, #8719 ),
 ( #8581, #26135 ),
 ( #6425, #21823 ),
 ( #2084, #10887 ) ),
 .UNSPECIFIED., .F., .F., .F. ) 
 B_SPLINE_SURFACE_WITH_KNOTS ( ( 4, 4 ),
 ( 2, 2 ),
 ( 0.000000000000000000, 1.000000000000000000 ),
 ( 0.000000000000000000, 1.000000000000000000 ),
 .UNSPECIFIED. ) 
 GEOMETRIC_REPRESENTATION_ITEM ( )  RATIONAL_B_SPLINE_SURFACE ( (
 ( 1.000000000000000000, 1.000000000000000000),
 ( 0.9956975270656955868, 0.8568959468854907557),
 ( 0.9956975270656955868, 0.8568959468854907557),
 ( 1.000000000000000000, 1.000000000000000000) ) ) 
 REPRESENTATION_ITEM ( '' )  SURFACE ( )  );
#20115 = ORIENTED_EDGE ( 'NONE', *, *, #22095, .T. ) ;
#20116 = CARTESIAN_POINT ( 'NONE',  ( -22.34422965417106965, 37.57019010019570260, -5.100074259622762618 ) ) ;
#20117 = CARTESIAN_POINT ( 'NONE',  ( -20.20700224038492010, -10.08426345511570332, 27.82980252387829623 ) ) ;
#20118 = CARTESIAN_POINT ( 'NONE',  ( -1.044557008772710516, -37.98985164565307571, 25.56990300677022177 ) ) ;
#20119 = CARTESIAN_POINT ( 'NONE',  ( -2.265401668238148591, 46.93990709177546705, 2.645701981445969686 ) ) ;
#20120 = CARTESIAN_POINT ( 'NONE',  ( 94.22246935314088034, -69.99999999999998579, -6.938893903907228378E-15 ) ) ;
#20121 = CARTESIAN_POINT ( 'NONE',  ( -20.20700224038492721, 29.58392382092673500, -0.9908225410479557516 ) ) ;
#20122 = CARTESIAN_POINT ( 'NONE',  ( 25.64708228042120908, -91.32398912286983261, -66.39944550735367557 ) ) ;
#20123 = EDGE_LOOP ( 'NONE', ( #24087, #11739, #7950, #25008 ) ) ;
#20124 = CARTESIAN_POINT ( 'NONE',  ( 10.93730112725977932, -108.9902118373748863, 104.7670965581006755 ) ) ;
#20125 = CARTESIAN_POINT ( 'NONE',  ( 2.430230287190589422, 132.3371620660959138, -60.50928654924622663 ) ) ;
#20126 = CARTESIAN_POINT ( 'NONE',  ( 24.22246935314087324, 0.000000000000000000, -111.9614997405030152 ) ) ;
#20127 = CARTESIAN_POINT ( 'NONE',  ( -55.24271866751342941, 0.009388511352198142604, 0.001425019990782173561 ) ) ;
#20128 = B_SPLINE_CURVE_WITH_KNOTS ( 'NONE', 3,
 ( #9662, #7667, #2901, #11960, #27205, #9818, #23067, #7518 ),
 .UNSPECIFIED., .F., .F.,
 ( 4, 2, 2, 4 ),
 ( 0.000000000000000000, 0.0002429588503611202919, 0.0004859177007222405839, 0.0009718354014444863720 ),
 .UNSPECIFIED. ) ;
#20129 = CARTESIAN_POINT ( 'NONE',  ( 25.98107933586707219, 102.9042679418251964, 47.01057192495316883 ) ) ;
#20130 = CARTESIAN_POINT ( 'NONE',  ( 2.433796855181219243, 118.5671979538068257, -84.34988187690807138 ) ) ;
#20131 = CARTESIAN_POINT ( 'NONE',  ( 109.1586059443104944, -0.002622205828288729987, -0.006570129623060863393 ) ) ;
#20132 = CARTESIAN_POINT ( 'NONE',  ( 1.894214914920970605, -142.1734439042095630, -29.24491455759085667 ) ) ;
#20133 = ORIENTED_EDGE ( 'NONE', *, *, #19595, .F. ) ;
#20134 = B_SPLINE_CURVE_WITH_KNOTS ( 'NONE', 3,
 ( #26078, #2301, #10968, #14079 ),
 .UNSPECIFIED., .F., .F.,
 ( 4, 4 ),
 ( 0.000000000000000000, 0.01077107196513851610 ),
 .UNSPECIFIED. ) ;
#20135 = ORIENTED_EDGE ( 'NONE', *, *, #12566, .F. ) ;
#20136 = ORIENTED_EDGE ( 'NONE', *, *, #25823, .F. ) ;
#20137 = EDGE_CURVE ( 'NONE', #19171, #17689, #16134, .T. ) ;
#20138 = CARTESIAN_POINT ( 'NONE',  ( -28.13707043255157103, -22.00298671236744497, -6.342158660426917116 ) ) ;
#20139 = DIRECTION ( 'NONE',  ( -1.000000000000000000, 6.938893903907226837E-18, -1.734723475976806709E-18 ) ) ;
#20140 = CARTESIAN_POINT ( 'NONE',  ( 6.224689322667647851, 141.5842213414013600, 43.30635742325425497 ) ) ;
#20141 = AXIS2_PLACEMENT_3D ( 'NONE', #7261, #2937, #13715 ) ;
#20142 = ADVANCED_FACE ( 'NONE', ( #26445 ), #24516, .F. ) ;
#20143 = CARTESIAN_POINT ( 'NONE',  ( 109.1592201516379674, 0.002134489919774364575, 0.007566779963318560377 ) ) ;
#20144 = VERTEX_POINT ( 'NONE', #10645 ) ;
#20145 = CARTESIAN_POINT ( 'NONE',  ( -25.21435515916043713, 25.00736669481056751, 23.92354251275909505 ) ) ;
#20146 = CARTESIAN_POINT ( 'NONE',  ( 26.11404676487257603, 74.91683232330973397, 84.89295829319517850 ) ) ;
#20147 = CARTESIAN_POINT ( 'NONE',  ( -9.156249394959713683, 38.89149400288408032, -38.17928057392006025 ) ) ;
#20148 = VERTEX_POINT ( 'NONE', #19412 ) ;
#20149 = CARTESIAN_POINT ( 'NONE',  ( -25.21435515916025594, 34.29329011225976132, 4.655591116594488099 ) ) ;
#20150 = ORIENTED_EDGE ( 'NONE', *, *, #11120, .F. ) ;
#20151 = CARTESIAN_POINT ( 'NONE',  ( 1.833721034905586800, 141.8643653601974961, -30.51809396650877559 ) ) ;
#20152 = CARTESIAN_POINT ( 'NONE',  ( 32.73300124599738581, -55.46353551261936587, -103.7392577722181812 ) ) ;
#20153 = CARTESIAN_POINT ( 'NONE',  ( 109.1586900883932856, 0.007137750914550311347, -0.0001010081143976270922 ) ) ;
#20154 = CARTESIAN_POINT ( 'NONE',  ( -28.13707043255157103, 7.802116958609309094, 21.52861750560930432 ) ) ;
#20155 = CARTESIAN_POINT ( 'NONE',  ( 1.833838848569429469, 132.4919773286277405, -59.18404309081229542 ) ) ;
#20156 = CARTESIAN_POINT ( 'NONE',  ( -9.156249394959713683, 8.027840202794694235, 53.90509764945120708 ) ) ;
#20157 = FACE_OUTER_BOUND ( 'NONE', #26622, .T. ) ;
#20158 = CARTESIAN_POINT ( 'NONE',  ( -20.21097721712958517, -9.464413111084555297, 28.05863618200118381 ) ) ;
#20159 = CARTESIAN_POINT ( 'NONE',  ( 2.063896406836605024, 107.0521644432417503, 98.19887492195893230 ) ) ;
#20160 = CARTESIAN_POINT ( 'NONE',  ( -12.82751273423880356, -6.573887447703164355, -48.43568301531138331 ) ) ;
#20161 = VECTOR ( 'NONE', #24959, 1000.000000000000000 ) ;
#20162 = CARTESIAN_POINT ( 'NONE',  ( 25.64681081121879203, -107.2555980796243773, 35.28660243342513070 ) ) ;
#20163 = VERTEX_POINT ( 'NONE', #8484 ) ;
#20164 = VECTOR ( 'NONE', #19847, 1000.000000000000341 ) ;
#20165 = VERTEX_POINT ( 'NONE', #21717 ) ;
#20166 = CARTESIAN_POINT ( 'NONE',  ( 1.893872463202055378, -96.41404152942862993, -108.5026245911428475 ) ) ;
#20167 = CARTESIAN_POINT ( 'NONE',  ( -1.046935749539997573, 45.77872888003167162, 1.275486069320633353 ) ) ;
#20168 = ORIENTED_EDGE ( 'NONE', *, *, #9707, .T. ) ;
#20169 = B_SPLINE_CURVE_WITH_KNOTS ( 'NONE', 3,
 ( #7472, #1127, #7765, #5881, #14353, #16523, #1257 ),
 .UNSPECIFIED., .F., .F.,
 ( 4, 3, 4 ),
 ( 0.000000000000000000, 0.02398743853561364700, 0.04000277880656215312 ),
 .UNSPECIFIED. ) ;
#20170 = ORIENTED_EDGE ( 'NONE', *, *, #2658, .F. ) ;
#20171 = ORIENTED_EDGE ( 'NONE', *, *, #27400, .F. ) ;
#20172 = CARTESIAN_POINT ( 'NONE',  ( 2.063896406836609909, 86.47093297169000436, 116.7302989755740725 ) ) ;
#20173 = CARTESIAN_POINT ( 'NONE',  ( 2.433796855181233454, -126.7346379669250780, -71.49415740225209959 ) ) ;
#20174 = EDGE_CURVE ( 'NONE', #24273, #16312, #26288, .T. ) ;
#20175 = CARTESIAN_POINT ( 'NONE',  ( -1.031422197589711987, 1.530725436378101989, 45.78027046666441180 ) ) ;
#20176 = EDGE_CURVE ( 'NONE', #23697, #26503, #5103, .T. ) ;
#20177 = ADVANCED_FACE ( 'NONE', ( #25122 ), #8687, .F. ) ;
#20178 = CARTESIAN_POINT ( 'NONE',  ( 25.64670758986459376, -107.2298587623393047, -35.36461833156630519 ) ) ;
#20179 = CARTESIAN_POINT ( 'NONE',  ( 32.73300124599735739, -39.98094346392385745, 110.6325518752272501 ) ) ;
#20180 = CARTESIAN_POINT ( 'NONE',  ( 32.73300124599735739, -72.21147546950616913, 92.86301839379999024 ) ) ;
#20181 = CARTESIAN_POINT ( 'NONE',  ( 55.49584447822657296, -42.42793568432998086, 58.85239198729172472 ) ) ;
#20182 = CARTESIAN_POINT ( 'NONE',  ( 24.22246935314087324, 1.371132922849442231E-14, 111.9614997405030152 ) ) ;
#20183 = CARTESIAN_POINT ( 'NONE',  ( 109.1589550718175161, 0.002126635388718530872, -0.007270618150635357012 ) ) ;
#20184 = CARTESIAN_POINT ( 'NONE',  ( 26.28373643307403640, 91.96212244992503315, -88.40064398363983855 ) ) ;
#20185 = ORIENTED_EDGE ( 'NONE', *, *, #18654, .F. ) ;
#20186 = CARTESIAN_POINT ( 'NONE',  ( 26.11404676487257603, -112.4785329405481065, -12.95861723607569438 ) ) ;
#20187 = CARTESIAN_POINT ( 'NONE',  ( 1.833838848569417701, -144.3334397096298005, -14.99110384899675807 ) ) ;
#20188 = DIRECTION ( 'NONE',  ( -0.5946245182733608248, -0.6521823330502958260, -0.4701913299128841484 ) ) ;
#20189 = CARTESIAN_POINT ( 'NONE',  ( -55.24271866751342941, -0.004365563123939050251, 0.008433070970613824532 ) ) ;
#20190 = CARTESIAN_POINT ( 'NONE',  ( -25.21435515916043713, -30.48034229288627017, 16.39063784838775462 ) ) ;
#20191 = ORIENTED_EDGE ( 'NONE', *, *, #2155, .T. ) ;
#20192 = CARTESIAN_POINT ( 'NONE',  ( 32.73300124599735739, -16.10546300444903167, 116.5274707358854869 ) ) ;
#20193 = ORIENTED_EDGE ( 'NONE', *, *, #25079, .T. ) ;
#20194 = CARTESIAN_POINT ( 'NONE',  ( -8.786685647604885574, 6.096987947571466530E-17, -1.524246986892866633E-17 ) ) ;
#20195 = CARTESIAN_POINT ( 'NONE',  ( 26.11404676487257603, -98.61392875273402581, 55.62948129436210110 ) ) ;
#20196 = EDGE_LOOP ( 'NONE', ( #724, #24772, #3635, #27541 ) ) ;
#20197 = CARTESIAN_POINT ( 'NONE',  ( -18.41936578851710493, -5.707900577127883679, 42.05131332928132082 ) ) ;
#20198 = EDGE_CURVE ( 'NONE', #24626, #19219, #21066, .T. ) ;
#20199 = VERTEX_POINT ( 'NONE', #14303 ) ;
#20200 = CARTESIAN_POINT ( 'NONE',  ( -25.21435515916043713, -34.05351380035337883, -6.169479169075319014 ) ) ;
#20201 = ORIENTED_EDGE ( 'NONE', *, *, #22784, .T. ) ;
#20202 = ADVANCED_FACE ( 'NONE', ( #7421 ), #8867, .F. ) ;
#20203 = VERTEX_POINT ( 'NONE', #3096 ) ;
#20204 = FACE_OUTER_BOUND ( 'NONE', #13262, .T. ) ;
#20205 = CARTESIAN_POINT ( 'NONE',  ( 1.893872463202042500, 125.2243573918634638, 73.39855082356687888 ) ) ;
#20206 = CARTESIAN_POINT ( 'NONE',  ( 1.833206308920111827, 137.7753864329225166, 45.54896581797505917 ) ) ;
#20207 = CARTESIAN_POINT ( 'NONE',  ( 25.64699802086726521, -66.17503410043964607, 91.48665801621639559 ) ) ;
#20208 = CARTESIAN_POINT ( 'NONE',  ( 1.833485406944043827, -73.01664920992880070, -125.4007332306553195 ) ) ;
#20209 = CARTESIAN_POINT ( 'NONE',  ( 55.49584447822657296, 7.849835876628332265, 72.12568090333346049 ) ) ;
#20210 = CIRCLE ( 'NONE', #11491, 151.1787379149930359 ) ;
#20211 = CARTESIAN_POINT ( 'NONE',  ( 6.224689322667630975, -141.5842213414016157, 43.30635742325330284 ) ) ;
#20212 = CARTESIAN_POINT ( 'NONE',  ( 28.37603512858452959, -86.45299531409403926, -75.42810021528178765 ) ) ;
#20213 = CARTESIAN_POINT ( 'NONE',  ( -1.048172774974291066, 1.020161070261757841, 45.78636862970791555 ) ) ;
#20214 = ORIENTED_EDGE ( 'NONE', *, *, #16587, .F. ) ;
#20215 = CARTESIAN_POINT ( 'NONE',  ( -1.045287976400365970, -43.05558670614224326, 15.59869763335140469 ) ) ;
#20217 = CARTESIAN_POINT ( 'NONE',  ( -1.619063947482197729, -38.92136151114925724, -25.20140673341360227 ) ) ;
#20216 = CARTESIAN_POINT ( 'NONE',  ( -20.21097721712959228, -29.61001327235739566, -0.3305963429841727863 ) ) ;
#20218 = CARTESIAN_POINT ( 'NONE',  ( -22.23226125620929139, 2.179935373562892131, 31.55376588768475798 ) ) ;
#20219 = CARTESIAN_POINT ( 'NONE',  ( 28.37603512858447274, -109.6581134439365570, -33.74339723237898880 ) ) ;
#20220 = CARTESIAN_POINT ( 'NONE',  ( -24.53239521893648245, -33.25736993155760501, 6.738460611583118265 ) ) ;
#20221 = CARTESIAN_POINT ( 'NONE',  ( 10.93730112725990189, -140.0398180619108075, -56.95489579269887059 ) ) ;
#20222 = CARTESIAN_POINT ( 'NONE',  ( 109.1586900883932856, -0.0008465529156546314172, 0.007088091345232576390 ) ) ;
#20223 = ORIENTED_EDGE ( 'NONE', *, *, #4713, .F. ) ;
#20224 = CARTESIAN_POINT ( 'NONE',  ( 25.64708228042117355, 110.4520805602538758, -23.43704872438652131 ) ) ;
#20225 = ORIENTED_EDGE ( 'NONE', *, *, #6162, .F. ) ;
#20226 = CARTESIAN_POINT ( 'NONE',  ( -1.323439229708149867, -16.42345129173367013, -43.04565903621277556 ) ) ;
#20227 = ADVANCED_FACE ( 'NONE', ( #9569 ), #11815, .F. ) ;
#20228 = EDGE_CURVE ( 'NONE', #28300, #22454, #24024, .T. ) ;
#20229 = AXIS2_PLACEMENT_3D ( 'NONE', #441, #22920, #3178 ) ;
#20230 = CARTESIAN_POINT ( 'NONE',  ( -8.786685647604896232, 25.35688121747570278, 47.14957014837326454 ) ) ;
#20231 = B_SPLINE_CURVE_WITH_KNOTS ( 'NONE', 3,
 ( #8762, #26178, #6756, #8916, #13080, #2261 ),
 .UNSPECIFIED., .F., .F.,
 ( 4, 2, 4 ),
 ( 8.673617379884034509E-19, 0.0004335184443140208837, 0.0008670368886280409000 ),
 .UNSPECIFIED. ) ;
#20232 = VERTEX_POINT ( 'NONE', #3512 ) ;
#20233 = CARTESIAN_POINT ( 'NONE',  ( -55.24390624410018802, 0.009374879212971231821, -0.004572280736701976080 ) ) ;
#20234 = AXIS2_PLACEMENT_3D ( 'NONE', #2767, #6526, #11547 ) ;
#20235 = VERTEX_POINT ( 'NONE', #14157 ) ;
#20236 = CARTESIAN_POINT ( 'NONE',  ( 1.834118845439484335, 138.0627591860429959, 44.67218053242439879 ) ) ;
#20237 = ORIENTED_EDGE ( 'NONE', *, *, #7896, .T. ) ;
#20238 =( NAMED_UNIT ( * ) SI_UNIT ( $, .STERADIAN. ) SOLID_ANGLE_UNIT ( ) );
#20239 =( BOUNDED_SURFACE ( )  B_SPLINE_SURFACE ( 3, 1, ( 
 ( #25968, #25206 ),
 ( #3179, #14103 ),
 ( #3322, #870 ),
 ( #27350, #24928 ) ),
 .UNSPECIFIED., .F., .F., .F. ) 
 B_SPLINE_SURFACE_WITH_KNOTS ( ( 4, 4 ),
 ( 2, 2 ),
 ( 0.000000000000000000, 1.000000000000000000 ),
 ( 0.000000000000000000, 1.000000000000000000 ),
 .UNSPECIFIED. ) 
 GEOMETRIC_REPRESENTATION_ITEM ( )  RATIONAL_B_SPLINE_SURFACE ( (
 ( 1.000000000000000000, 1.000000000000000000),
 ( 0.9960225298536222738, 0.9999952330161893110),
 ( 0.9960225298536222738, 0.9999952330161893110),
 ( 1.000000000000000000, 1.000000000000000000) ) ) 
 REPRESENTATION_ITEM ( '' )  SURFACE ( )  );
#20240 = CARTESIAN_POINT ( 'NONE',  ( -21.41427618760457818, -19.54551635498111395, 23.81423075802604217 ) ) ;
#20241 = CONICAL_SURFACE ( 'NONE', #6488, 117.6351876552689504, 0.9945805576725580410 ) ;
#20242 = CARTESIAN_POINT ( 'NONE',  ( 25.64692872815576408, 107.4838747185725651, -34.58541472378539794 ) ) ;
#20243 = CARTESIAN_POINT ( 'NONE',  ( -20.57838717382308147, -28.96176188950224528, -7.715628353033566533 ) ) ;
#20244 = CARTESIAN_POINT ( 'NONE',  ( 30.59141879584290891, -75.73279557183244037, -88.14706749784132001 ) ) ;
#20245 = CARTESIAN_POINT ( 'NONE',  ( 25.69398547355838147, -112.9401428107247654, 0.7422864227361197775 ) ) ;
#20246 = VERTEX_POINT ( 'NONE', #27702 ) ;
#20247 = ADVANCED_FACE ( 'NONE', ( #22979 ), #14581, .F. ) ;
#20248 = DIRECTION ( 'NONE',  ( 0.000000000000000000, 0.000000000000000000, 1.000000000000000000 ) ) ;
#20249 = CARTESIAN_POINT ( 'NONE',  ( -8.786685647604890903, -37.00619870957905277, 38.68584556812340480 ) ) ;
#20250 = FACE_OUTER_BOUND ( 'NONE', #22460, .T. ) ;
#20251 = ORIENTED_EDGE ( 'NONE', *, *, #3936, .F. ) ;
#20252 = VECTOR ( 'NONE', #26114, 999.9999999999998863 ) ;
#20253 = VERTEX_POINT ( 'NONE', #5248 ) ;
#20254 = VECTOR ( 'NONE', #27600, 999.9999999999998863 ) ;
#20255 = CARTESIAN_POINT ( 'NONE',  ( 94.22246935314088034, -151.1871800109700246, 12.49999999999999467 ) ) ;
#20256 = CARTESIAN_POINT ( 'NONE',  ( -4.473127245936431073, -41.70021447285034810, 26.34600523034583119 ) ) ;
#20257 = CARTESIAN_POINT ( 'NONE',  ( 25.65782528836481902, -24.04194111108942522, 110.3293115225706202 ) ) ;
#20258 = AXIS2_PLACEMENT_3D ( 'NONE', #23695, #5838, #14308 ) ;
#20259 = DIRECTION ( 'NONE',  ( 5.541455922705463698E-20, -5.223019709708320524E-21, 1.000000000000000000 ) ) ;
#20260 = CARTESIAN_POINT ( 'NONE',  ( 10.93730112725994097, -51.37919228020192008, -142.1801301103790536 ) ) ;
#20261 = CARTESIAN_POINT ( 'NONE',  ( -23.77929240705206126, 25.06639637888459404, 26.20227034809527211 ) ) ;
#20262 = VERTEX_POINT ( 'NONE', #14019 ) ;
#20263 = CARTESIAN_POINT ( 'NONE',  ( 109.1587776205901577, 0.006305329297952418956, 0.003736572840486965252 ) ) ;
#20264 = CARTESIAN_POINT ( 'NONE',  ( -1.619063947482201282, -16.67502769180592992, -43.26576862488428077 ) ) ;
#20265 = AXIS2_PLACEMENT_3D ( 'NONE', #27146, #20391, #4855 ) ;
#20266 = CARTESIAN_POINT ( 'NONE',  ( 1.833750490713744297, -145.1094586213657465, -0.2669522761660584886 ) ) ;
#20267 = EDGE_CURVE ( 'NONE', #8144, #17963, #5853, .T. ) ;
#20268 = CARTESIAN_POINT ( 'NONE',  ( -1.031422197589716205, -36.13727897780147202, -28.14735071801731792 ) ) ;
#20269 = EDGE_CURVE ( 'NONE', #12529, #3847, #10567, .T. ) ;
#20270 = CARTESIAN_POINT ( 'NONE',  ( 109.1592201516379674, 0.0003082430542015802727, 0.007856029051022768092 ) ) ;
#20271 = ORIENTED_EDGE ( 'NONE', *, *, #1774, .F. ) ;
#20272 = CARTESIAN_POINT ( 'NONE',  ( 25.87036335909427009, -12.80197335559886085, -112.3329723497412544 ) ) ;
#20273 = PRODUCT_DEFINITION_SHAPE ( 'NONE', 'NONE',  #28486 ) ;
#20274 = EDGE_LOOP ( 'NONE', ( #1228, #1015, #25639, #26026 ) ) ;
#20276 = EDGE_CURVE ( 'NONE', #27090, #26821, #21288, .T. ) ;
#20275 = DIRECTION ( 'NONE',  ( 0.5946245182733607137, -0.002950380665396057540, 0.8039981203473692828 ) ) ;
#20277 = CARTESIAN_POINT ( 'NONE',  ( 25.64708228042119487, -56.42152786924437180, -97.80372460135731671 ) ) ;
#20278 = ORIENTED_EDGE ( 'NONE', *, *, #16340, .F. ) ;
#20279 = B_SPLINE_CURVE_WITH_KNOTS ( 'NONE', 3,
 ( #8255, #7842, #10420, #19186, #6107, #14862, #16603, #23244 ),
 .UNSPECIFIED., .F., .F.,
 ( 4, 2, 2, 4 ),
 ( 0.000000000000000000, 0.002761524886576655416, 0.005523049773153310832, 0.01104609954630660432 ),
 .UNSPECIFIED. ) ;
#20280 = EDGE_CURVE ( 'NONE', #5960, #17673, #2046, .T. ) ;
#20281 = VERTEX_POINT ( 'NONE', #25830 ) ;
#20282 = VERTEX_POINT ( 'NONE', #10436 ) ;
#20283 = CIRCLE ( 'NONE', #21660, 151.1787379149930359 ) ;
#20284 = AXIS2_PLACEMENT_3D ( 'NONE', #13328, #22127, #21850 ) ;
#20285 = CARTESIAN_POINT ( 'NONE',  ( 25.69398547355839568, 84.42756928260575933, 75.02007992711736506 ) ) ;
#20286 = LINE ( 'NONE', #9073, #21627 ) ;
#20287 =( BOUNDED_SURFACE ( )  B_SPLINE_SURFACE ( 3, 1, ( 
 ( #12515, #1442 ),
 ( #5920, #1165 ),
 ( #23059, #21009 ),
 ( #27636, #20879 ) ),
 .UNSPECIFIED., .F., .F., .F. ) 
 B_SPLINE_SURFACE_WITH_KNOTS ( ( 4, 4 ),
 ( 2, 2 ),
 ( 0.000000000000000000, 1.000000000000000000 ),
 ( 0.000000000000000000, 1.000000000000000000 ),
 .UNSPECIFIED. ) 
 GEOMETRIC_REPRESENTATION_ITEM ( )  RATIONAL_B_SPLINE_SURFACE ( (
 ( 1.000000000000000000, 1.000000000000000000),
 ( 0.6386103224230302855, 0.9954351624131538845),
 ( 0.6386103224230302855, 0.9954351624131538845),
 ( 1.000000000000000000, 1.000000000000000000) ) ) 
 REPRESENTATION_ITEM ( '' )  SURFACE ( )  );
#20288 = FACE_OUTER_BOUND ( 'NONE', #7601, .T. ) ;
#20289 = CARTESIAN_POINT ( 'NONE',  ( 0.000000000000000000, 0.000000000000000000, 0.000000000000000000 ) ) ;
#20290 = ORIENTED_EDGE ( 'NONE', *, *, #20068, .T. ) ;
#20291 = CARTESIAN_POINT ( 'NONE',  ( -21.81686047589426636, 27.83628745321488296, 26.62923599424938459 ) ) ;
#20292 = CARTESIAN_POINT ( 'NONE',  ( 25.64681081121879203, -102.9795863647031666, 46.30456157731292421 ) ) ;
#20293 = CARTESIAN_POINT ( 'NONE',  ( 2.263178113027022764, -142.5035404044876088, 28.85718369185665821 ) ) ;
#20294 = VERTEX_POINT ( 'NONE', #12845 ) ;
#20295 = ORIENTED_EDGE ( 'NONE', *, *, #21324, .T. ) ;
#20296 = CARTESIAN_POINT ( 'NONE',  ( -1.031422197589711764, -45.78027046666444733, -1.530725436377303073 ) ) ;
#20297 = CARTESIAN_POINT ( 'NONE',  ( 1.833206308920058536, 14.42724735286848947, 144.3905119031280719 ) ) ;
#20298 = CARTESIAN_POINT ( 'NONE',  ( -18.41936578851709072, 38.22933728004715448, 18.42310649277586876 ) ) ;
#20299 = DIRECTION ( 'NONE',  ( -0.7637818620346800147, -0.2198041754873968356, -0.6068965246771005351 ) ) ;
#20300 = CARTESIAN_POINT ( 'NONE',  ( -40.00000000000000000, 0.000000000000000000, -80.00000000000000000 ) ) ;
#20301 = CARTESIAN_POINT ( 'NONE',  ( -1.323830074806768176, 44.47857376182273015, -12.01461446423216906 ) ) ;
#20302 = FACE_OUTER_BOUND ( 'NONE', #25116, .T. ) ;
#20303 = EDGE_CURVE ( 'NONE', #21873, #19211, #2020, .T. ) ;
#20304 = EDGE_CURVE ( 'NONE', #17196, #6453, #23691, .T. ) ;
#20305 = CARTESIAN_POINT ( 'NONE',  ( -20.47566262905010248, 16.24827521404687403, 25.06314747784817243 ) ) ;
#20306 = CARTESIAN_POINT ( 'NONE',  ( 109.1587776205901861, -0.006729130500864231000, -0.002904816147411946967 ) ) ;
#20307 = CARTESIAN_POINT ( 'NONE',  ( -1.031422197589716205, 44.01264471863865424, 12.69107518035457005 ) ) ;
#20308 = VECTOR ( 'NONE', #12163, 1000.000000000000000 ) ;
#20309 = ORIENTED_EDGE ( 'NONE', *, *, #28135, .T. ) ;
#20311 = EDGE_CURVE ( 'NONE', #1484, #25606, #3059, .T. ) ;
#20310 = CARTESIAN_POINT ( 'NONE',  ( -8.786685647604890903, -53.04920435127188938, -7.199674155858766689 ) ) ;
#20312 = CARTESIAN_POINT ( 'NONE',  ( 8.186469829614216209, 71.65198613712979636, 131.0413692472655214 ) ) ;
#20313 = ORIENTED_EDGE ( 'NONE', *, *, #4002, .F. ) ;
#20314 = ORIENTED_EDGE ( 'NONE', *, *, #313, .F. ) ;
#20315 = ORIENTED_EDGE ( 'NONE', *, *, #12923, .F. ) ;
#20316 = CARTESIAN_POINT ( 'NONE',  ( -55.24271866751342941, -0.006757859501005985571, -0.006671293903669251422 ) ) ;
#20317 = B_SPLINE_CURVE_WITH_KNOTS ( 'NONE', 3,
 ( #4563, #26306, #17522, #19968 ),
 .UNSPECIFIED., .F., .F.,
 ( 4, 4 ),
 ( 0.000000000000000000, 0.01077107196513799221 ),
 .UNSPECIFIED. ) ;
#20318 = CARTESIAN_POINT ( 'NONE',  ( 109.1586900883932856, 0.004277182003220953051, -0.005715190711488734449 ) ) ;
#20319 = CARTESIAN_POINT ( 'NONE',  ( -55.24271866751342941, 0.006671293903668402275, 0.006757859501010043089 ) ) ;
#20320 = CARTESIAN_POINT ( 'NONE',  ( -1.239374126674604337, 45.98822239537608425, -2.406737988131283146 ) ) ;
#20321 = CARTESIAN_POINT ( 'NONE',  ( 25.70243777736189017, -107.1912711514952576, -35.59945151684184594 ) ) ;
#20322 = VECTOR ( 'NONE', #16367, 1000.000000000000000 ) ;
#20323 = AXIS2_PLACEMENT_3D ( 'NONE', #1294, #25771, #5627 ) ;
#20324 = CARTESIAN_POINT ( 'NONE',  ( 32.73300124599732186, 0.000000000000000000, 0.000000000000000000 ) ) ;
#20325 = CARTESIAN_POINT ( 'NONE',  ( -1.155001620486246550, -16.13799328198394178, 42.97366440495927975 ) ) ;
#20326 = CARTESIAN_POINT ( 'NONE',  ( -1.619063947482197729, 43.26576862488456499, 16.67502769180516964 ) ) ;
#20327 = CARTESIAN_POINT ( 'NONE',  ( 1.833485406944057594, -132.7804117027884274, -58.53321471327013370 ) ) ;
#20328 = CARTESIAN_POINT ( 'NONE',  ( 26.11404676487257603, 33.91085499298377925, 108.0249973236468577 ) ) ;
#20329 =( BOUNDED_SURFACE ( )  B_SPLINE_SURFACE ( 3, 1, ( 
 ( #20673, #966 ),
 ( #9902, #5571 ),
 ( #9751, #18524 ),
 ( #14336, #16361 ) ),
 .UNSPECIFIED., .F., .F., .F. ) 
 B_SPLINE_SURFACE_WITH_KNOTS ( ( 4, 4 ),
 ( 2, 2 ),
 ( 0.000000000000000000, 1.000000000000000000 ),
 ( 0.000000000000000000, 1.000000000000000000 ),
 .UNSPECIFIED. ) 
 GEOMETRIC_REPRESENTATION_ITEM ( )  RATIONAL_B_SPLINE_SURFACE ( (
 ( 1.000000000000000000, 1.000000000000000000),
 ( 0.9934239774497838349, 0.8357310067453913582),
 ( 0.9934239774497838349, 0.8357310067453913582),
 ( 1.000000000000000000, 1.000000000000000000) ) ) 
 REPRESENTATION_ITEM ( '' )  SURFACE ( )  );
#20330 = CARTESIAN_POINT ( 'NONE',  ( -1.619063947482197729, -43.26576862488421682, 16.67502769180607203 ) ) ;
#20331 = CARTESIAN_POINT ( 'NONE',  ( -1.583189561560253589, -2.490696082060195327, -46.33203782964460515 ) ) ;
#20332 = DIRECTION ( 'NONE',  ( 0.000000000000000000, 5.223019709707975211E-21, -1.000000000000000000 ) ) ;
#20333 = ORIENTED_EDGE ( 'NONE', *, *, #13544, .T. ) ;
#20335 = CARTESIAN_POINT ( 'NONE',  ( 109.1624594426973118, -0.001206615835669557933, 0.01591840958353239049 ) ) ;
#20334 = CARTESIAN_POINT ( 'NONE',  ( -4.473127245936434626, 47.80062405537817938, 12.17046501147466842 ) ) ;
#20336 = EDGE_CURVE ( 'NONE', #12735, #21937, #10310, .T. ) ;
#20337 = CARTESIAN_POINT ( 'NONE',  ( -55.24198130335446422, -0.001516807524707838167, 0.009170435128245089246 ) ) ;
#20338 = CARTESIAN_POINT ( 'NONE',  ( 10.93730112726002979, 92.80059208661855052, -119.3442956573263558 ) ) ;
#20339 = CARTESIAN_POINT ( 'NONE',  ( -55.24198130335446422, -0.001516807524707838167, 0.009170435128245089246 ) ) ;
#20340 = CARTESIAN_POINT ( 'NONE',  ( -2.904412668506660911, -11.97478724945543860, -46.12477647685269488 ) ) ;
#20341 = ORIENTED_EDGE ( 'NONE', *, *, #24795, .F. ) ;
#20342 = CARTESIAN_POINT ( 'NONE',  ( -1.031422197589711764, 15.60268798220637798, -43.06660437151313658 ) ) ;
#20343 = ORIENTED_EDGE ( 'NONE', *, *, #7110, .F. ) ;
#20345 = EDGE_CURVE ( 'NONE', #17200, #3161, #8220, .T. ) ;
#20344 = DIRECTION ( 'NONE',  ( 1.000000000000000000, -6.938893903907226837E-18, 1.734723475976806709E-18 ) ) ;
#20346 = B_SPLINE_CURVE_WITH_KNOTS ( 'NONE', 3,
 ( #28183, #26172, #17111, #4428, #117, #15494, #14946 ),
 .UNSPECIFIED., .F., .F.,
 ( 4, 3, 4 ),
 ( 0.000000000000000000, 0.006568092053401789268, 0.02506242213020845946 ),
 .UNSPECIFIED. ) ;
#20347 = CARTESIAN_POINT ( 'NONE',  ( 25.64681081121880624, 12.21581276189807497, 112.2483031020013868 ) ) ;
#20348 = ORIENTED_EDGE ( 'NONE', *, *, #16929, .F. ) ;
#20349 = ADVANCED_FACE ( 'NONE', ( #19334 ), #19069, .F. ) ;
#20350 = CARTESIAN_POINT ( 'NONE',  ( -23.79223135445719350, -30.42557260166821109, -13.25822371132282917 ) ) ;
#20351 = CIRCLE ( 'NONE', #10277, 117.6351876552689504 ) ;
#20352 = ORIENTED_EDGE ( 'NONE', *, *, #17599, .T. ) ;
#20353 = CARTESIAN_POINT ( 'NONE',  ( -8.786685647604890903, -52.67761315067293282, -9.545808661480407409 ) ) ;
#20354 = VECTOR ( 'NONE', #5586, 1000.000000000000114 ) ;
#20355 = EDGE_LOOP ( 'NONE', ( #11465, #9779, #8399, #3593 ) ) ;
#20356 = VERTEX_POINT ( 'NONE', #27841 ) ;
#20357 = CARTESIAN_POINT ( 'NONE',  ( 109.1592201516379674, 0.001127733110588118211, 0.007780772729122761334 ) ) ;
#20358 = CARTESIAN_POINT ( 'NONE',  ( -28.41354790283022069, -22.41474081377996441, 5.969609727608259142 ) ) ;
#20359 = FACE_OUTER_BOUND ( 'NONE', #21645, .T. ) ;
#20360 = CARTESIAN_POINT ( 'NONE',  ( 109.1721716018069515, 0.01392660302850057957, -0.009868622090669602540 ) ) ;
#20361 = CONICAL_SURFACE ( 'NONE', #3835, 117.6351876552689504, 0.9945805576725580410 ) ;
#20362 = CARTESIAN_POINT ( 'NONE',  ( 5.340103579038068204, 135.6222865281528414, 57.86178752084538246 ) ) ;
#20363 = CARTESIAN_POINT ( 'NONE',  ( -1.050230346682680560, 26.92058491724867153, -37.05182464821992028 ) ) ;
#20364 = CARTESIAN_POINT ( 'NONE',  ( 1.834118845439484335, -97.22976650547352051, -107.7186227765464395 ) ) ;
#20366 =( BOUNDED_SURFACE ( )  B_SPLINE_SURFACE ( 3, 1, ( 
 ( #6828, #26386 ),
 ( #22223, #21931 ),
 ( #2190, #24387 ),
 ( #4656, #26659 ) ),
 .UNSPECIFIED., .F., .F., .F. ) 
 B_SPLINE_SURFACE_WITH_KNOTS ( ( 4, 4 ),
 ( 2, 2 ),
 ( 0.000000000000000000, 1.000000000000000000 ),
 ( 0.000000000000000000, 1.000000000000000000 ),
 .UNSPECIFIED. ) 
 GEOMETRIC_REPRESENTATION_ITEM ( )  RATIONAL_B_SPLINE_SURFACE ( (
 ( 1.000000000000000000, 1.000000000000000000),
 ( 0.6386103224230316178, 0.9954351624131538845),
 ( 0.6386103224230316178, 0.9954351624131538845),
 ( 1.000000000000000000, 1.000000000000000000) ) ) 
 REPRESENTATION_ITEM ( '' )  SURFACE ( )  );
#20365 = AXIS2_PLACEMENT_3D ( 'NONE', #22106, #6328, #17311 ) ;
#20367 = ORIENTED_EDGE ( 'NONE', *, *, #14089, .F. ) ;
#20368 = DIRECTION ( 'NONE',  ( -0.5914120900931442160, -0.3962188444547289912, 0.7023121577978114205 ) ) ;
#20370 = CARTESIAN_POINT ( 'NONE',  ( 25.86096068574581963, 45.07009591924560254, 103.6815822123520263 ) ) ;
#20369 = CARTESIAN_POINT ( 'NONE',  ( -20.57838717382308147, 10.78122205917000365, -27.96569011373090063 ) ) ;
#20371 = B_SPLINE_CURVE_WITH_KNOTS ( 'NONE', 3,
 ( #20560, #24325, #22598, #16095, #11354, #3013, #9490, #17685, #8928, #2864 ),
 .UNSPECIFIED., .F., .F.,
 ( 4, 3, 3, 4 ),
 ( 6.938893903907228378E-18, 0.0002669560319015760498, 0.0005492286108966415621, 0.0008315040496093473914 ),
 .UNSPECIFIED. ) ;
#20372 = EDGE_CURVE ( 'NONE', #11759, #8126, #13727, .T. ) ;
#20373 = CARTESIAN_POINT ( 'NONE',  ( 55.79472521941428198, 72.42790650415572884, 6.880567342319954705 ) ) ;
#20374 = CARTESIAN_POINT ( 'NONE',  ( 2.263178607246656870, 86.59154415224598722, 116.7985473178705860 ) ) ;
#20375 = ORIENTED_EDGE ( 'NONE', *, *, #11837, .F. ) ;
#20376 = ORIENTED_EDGE ( 'NONE', *, *, #24283, .T. ) ;
#20377 = CARTESIAN_POINT ( 'NONE',  ( 26.11404676487257603, 98.61392875273440950, -55.62948129436141897 ) ) ;
#20378 = CARTESIAN_POINT ( 'NONE',  ( -18.41936578851705519, -42.05131332928132082, -5.707900577128024011 ) ) ;
#20379 = CARTESIAN_POINT ( 'NONE',  ( 55.49584447822657296, -53.73688382046231737, -48.74506217377937389 ) ) ;
#20380 = EDGE_LOOP ( 'NONE', ( #23072, #26559, #5088, #6753 ) ) ;
#20381 = CARTESIAN_POINT ( 'NONE',  ( 26.11404676487257603, -36.06104232266525145, 107.3263591096429082 ) ) ;
#20382 = ORIENTED_EDGE ( 'NONE', *, *, #7705, .T. ) ;
#20383 = CARTESIAN_POINT ( 'NONE',  ( -1.113427685307007531, -16.03057832159182539, -42.96952363574826705 ) ) ;
#20384 = VECTOR ( 'NONE', #27025, 1000.000000000000114 ) ;
#20385 = CARTESIAN_POINT ( 'NONE',  ( -23.79223135445721837, -33.03345552685147624, -3.207301057648224596 ) ) ;
#20386 = ORIENTED_EDGE ( 'NONE', *, *, #3617, .F. ) ;
#20387 = DIRECTION ( 'NONE',  ( 0.000000000000000000, 0.000000000000000000, 1.000000000000000000 ) ) ;
#20388 = ORIENTED_EDGE ( 'NONE', *, *, #9342, .T. ) ;
#20389 = CARTESIAN_POINT ( 'NONE',  ( 109.1778270068192853, -0.0003511581237512927567, -0.009307953841270274684 ) ) ;
#20390 = EDGE_LOOP ( 'NONE', ( #4066, #9274, #24480, #13716 ) ) ;
#20391 = DIRECTION ( 'NONE',  ( 1.000000000000000000, -6.938893903907226837E-18, 1.734723475976806709E-18 ) ) ;
#20392 = CARTESIAN_POINT ( 'NONE',  ( 25.64681081121879203, -97.57530875170644435, 56.81519825470720519 ) ) ;
#20393 = CARTESIAN_POINT ( 'NONE',  ( -1.031422197589711987, -25.67058493451414591, 37.93675465142499803 ) ) ;
#20394 = CARTESIAN_POINT ( 'NONE',  ( 1.833721034905621661, -125.4904194343090182, 72.86293192427449128 ) ) ;
#20395 = ORIENTED_EDGE ( 'NONE', *, *, #17438, .F. ) ;
#20396 = B_SPLINE_CURVE_WITH_KNOTS ( 'NONE', 3,
 ( #21376, #12178, #14751, #18941 ),
 .UNSPECIFIED., .F., .F.,
 ( 4, 4 ),
 ( 3.332884739788762247E-16, 0.01077107486149806760 ),
 .UNSPECIFIED. ) ;
#20397 = EDGE_CURVE ( 'NONE', #6178, #1609, #27673, .T. ) ;
#20398 = CIRCLE ( 'NONE', #3402, 12.50000000000000000 ) ;
#20399 = CARTESIAN_POINT ( 'NONE',  ( 109.1592201516379674, -0.006174480289200349852, -0.004867031887010190086 ) ) ;
#20400 = CARTESIAN_POINT ( 'NONE',  ( 26.11404676487257603, 47.08215554553518700, 102.9690087468803341 ) ) ;
#20401 = CARTESIAN_POINT ( 'NONE',  ( 16.75465622695666923, -19.47041796022332605, 140.8868039942614985 ) ) ;
#20402 = ORIENTED_EDGE ( 'NONE', *, *, #6154, .F. ) ;
#20403 = EDGE_CURVE ( 'NONE', #24442, #16227, #2049, .T. ) ;
#20404 = ORIENTED_EDGE ( 'NONE', *, *, #24067, .F. ) ;
#20405 = ORIENTED_EDGE ( 'NONE', *, *, #20198, .T. ) ;
#20406 = FACE_OUTER_BOUND ( 'NONE', #26041, .T. ) ;
#20407 = CARTESIAN_POINT ( 'NONE',  ( -20.20612091757422135, -10.22177757278296184, 27.77903622052264865 ) ) ;
#20409 = CARTESIAN_POINT ( 'NONE',  ( -1.031422197589716205, 36.13727897780168519, 28.14735071801704436 ) ) ;
#20408 = CARTESIAN_POINT ( 'NONE',  ( 28.37599760073041821, 10.20682761621932499, 114.2774414139535253 ) ) ;
#20410 = EDGE_CURVE ( 'NONE', #8158, #22719, #9608, .T. ) ;
#20411 = CARTESIAN_POINT ( 'NONE',  ( -6.574463467970541153, -38.37705091668347279, 34.08059230520071026 ) ) ;
#20412 = CARTESIAN_POINT ( 'NONE',  ( -1.056502255334265339, -26.51074901220530222, -37.35734037467625512 ) ) ;
#20413 = CARTESIAN_POINT ( 'NONE',  ( -4.780792508754326597, -48.13366140756551914, 11.68149851467511446 ) ) ;
#20414 = ORIENTED_EDGE ( 'NONE', *, *, #8933, .T. ) ;
#20415 = CARTESIAN_POINT ( 'NONE',  ( 10.93730112726003156, 125.1380233598492140, -84.82621002473311478 ) ) ;
#20416 = CARTESIAN_POINT ( 'NONE',  ( 55.79472521941426777, 14.41365263906553196, 71.31192372336680307 ) ) ;
#20417 = CARTESIAN_POINT ( 'NONE',  ( -28.41354790283022069, -8.345538364877233661, -21.64275480268745255 ) ) ;
#20418 = CARTESIAN_POINT ( 'NONE',  ( 9.884929003653608603, 150.0922431698406285, -11.54837932062876860 ) ) ;
#20419 =( BOUNDED_SURFACE ( )  B_SPLINE_SURFACE ( 3, 1, ( 
 ( #11558, #3075 ),
 ( #11848, #20334 ),
 ( #10258, #25651 ),
 ( #22371, #2634 ) ),
 .UNSPECIFIED., .F., .F., .F. ) 
 B_SPLINE_SURFACE_WITH_KNOTS ( ( 4, 4 ),
 ( 2, 2 ),
 ( 0.000000000000000000, 1.000000000000000000 ),
 ( 0.000000000000000000, 1.000000000000000000 ),
 .UNSPECIFIED. ) 
 GEOMETRIC_REPRESENTATION_ITEM ( )  RATIONAL_B_SPLINE_SURFACE ( (
 ( 1.000000000000000000, 1.000000000000000000),
 ( 0.7789835883360576307, 0.9689951854195403280),
 ( 0.7789835883360576307, 0.9689951854195403280),
 ( 1.000000000000000000, 1.000000000000000000) ) ) 
 REPRESENTATION_ITEM ( '' )  SURFACE ( )  );
#20420 = CARTESIAN_POINT ( 'NONE',  ( 1.833485406944043827, 73.01664920993141550, -125.4007332306537563 ) ) ;
#20421 = CARTESIAN_POINT ( 'NONE',  ( 1.833206310202331935, 142.0914673790820757, 29.44113265020980919 ) ) ;
#20422 = EDGE_LOOP ( 'NONE', ( #964, #4781, #27152, #14242 ) ) ;
#20423 = DIRECTION ( 'NONE',  ( 0.000000000000000000, 0.000000000000000000, 1.000000000000000000 ) ) ;
#20424 = ORIENTED_EDGE ( 'NONE', *, *, #5528, .F. ) ;
#20425 = CARTESIAN_POINT ( 'NONE',  ( 1.833603222531957400, -29.73464781350154595, -142.0304769734131867 ) ) ;
#20427 = CARTESIAN_POINT ( 'NONE',  ( -1.539763995773685723, 11.93465967526358185, 44.72359274866469292 ) ) ;
#20426 = B_SPLINE_CURVE_WITH_KNOTS ( 'NONE', 3,
 ( #13187, #11185, #11461, #17789, #6735, #15480, #15345, #15778, #9027, #22273 ),
 .UNSPECIFIED., .F., .F.,
 ( 4, 3, 3, 4 ),
 ( 3.925231146709437917E-17, 0.0002669559177086255441, 0.0005339118354151083795, 0.001067817517169174875 ),
 .UNSPECIFIED. ) ;
#20428 = ORIENTED_EDGE ( 'NONE', *, *, #24157, .F. ) ;
#20429 =( BOUNDED_SURFACE ( )  B_SPLINE_SURFACE ( 3, 1, ( 
 ( #26174, #26725 ),
 ( #28323, #8621 ),
 ( #6466, #8759 ),
 ( #26586, #24171 ) ),
 .UNSPECIFIED., .F., .F., .F. ) 
 B_SPLINE_SURFACE_WITH_KNOTS ( ( 4, 4 ),
 ( 2, 2 ),
 ( 0.000000000000000000, 1.000000000000000000 ),
 ( 0.000000000000000000, 1.000000000000000000 ),
 .UNSPECIFIED. ) 
 GEOMETRIC_REPRESENTATION_ITEM ( )  RATIONAL_B_SPLINE_SURFACE ( (
 ( 1.000000000000000000, 1.000000000000000000),
 ( 0.6386103224230302855, 0.9954351624131538845),
 ( 0.6386103224230302855, 0.9954351624131538845),
 ( 1.000000000000000000, 1.000000000000000000) ) ) 
 REPRESENTATION_ITEM ( '' )  SURFACE ( )  );
#20430 = ORIENTED_EDGE ( 'NONE', *, *, #13617, .F. ) ;
#20431 = ORIENTED_EDGE ( 'NONE', *, *, #2162, .F. ) ;
#20432 = CARTESIAN_POINT ( 'NONE',  ( -9.156249394959713683, -38.17928057392020236, -38.89149400288393821 ) ) ;
#20433 = CARTESIAN_POINT ( 'NONE',  ( -1.031422197589711987, -44.01264471863856187, -12.69107518035484361 ) ) ;
#20434 = EDGE_CURVE ( 'NONE', #6842, #21998, #8249, .T. ) ;
#20435 = LINE ( 'NONE', #16110, #10301 ) ;
#20436 = DIRECTION ( 'NONE',  ( -1.000000000000000000, -0.000000000000000000, -0.000000000000000000 ) ) ;
#20437 = VERTEX_POINT ( 'NONE', #24100 ) ;
#20438 = CARTESIAN_POINT ( 'NONE',  ( -18.41936578851709783, 18.42310649277627022, -38.22933728004698395 ) ) ;
#20439 = CARTESIAN_POINT ( 'NONE',  ( 2.063896406836609909, -16.52087515463681200, -144.3268707900448931 ) ) ;
#20440 = DIRECTION ( 'NONE',  ( 0.7637818620346801257, 0.6201872550346656521, -0.1788995134688848854 ) ) ;
#20441 = VERTEX_POINT ( 'NONE', #22504 ) ;
#20442 = EDGE_CURVE ( 'NONE', #16465, #5899, #9963, .T. ) ;
#20443 = VERTEX_POINT ( 'NONE', #2326 ) ;
#20444 = CARTESIAN_POINT ( 'NONE',  ( -1.050230346682684113, -43.55729751025872787, -14.15335421912565828 ) ) ;
#20445 = CARTESIAN_POINT ( 'NONE',  ( -23.79248802219722236, 32.40806545715341258, 7.157555990716568672 ) ) ;
#20446 = CARTESIAN_POINT ( 'NONE',  ( 2.063896406836609909, -141.8093313989362798, 31.51663808384510546 ) ) ;
#20447 = CARTESIAN_POINT ( 'NONE',  ( -20.57838717382308147, 27.96569011373101077, 10.78122205916971055 ) ) ;
#20448 = CARTESIAN_POINT ( 'NONE',  ( 1.894214914920950843, 107.2270864706603248, -97.83100278581306952 ) ) ;
#20449 = ORIENTED_EDGE ( 'NONE', *, *, #25638, .T. ) ;
#20450 = CARTESIAN_POINT ( 'NONE',  ( -1.045287976400379737, 44.00138577190644185, -12.68782741917337198 ) ) ;
#20451 = CARTESIAN_POINT ( 'NONE',  ( 32.73300124599732186, 0.000000000000000000, 0.000000000000000000 ) ) ;
#20452 = CARTESIAN_POINT ( 'NONE',  ( -4.780792508754315051, -37.74278713234418348, -32.07473752860764904 ) ) ;
#20453 = CARTESIAN_POINT ( 'NONE',  ( 32.73300124599732186, 0.000000000000000000, 0.000000000000000000 ) ) ;
#20454 = CARTESIAN_POINT ( 'NONE',  ( 6.224689322667647851, 108.2965163446087615, -100.9623537450640924 ) ) ;
#20455 = ORIENTED_EDGE ( 'NONE', *, *, #26089, .F. ) ;
#20456 = CARTESIAN_POINT ( 'NONE',  ( 1.833485406944043827, 145.1085452359073145, 0.5339064996889848480 ) ) ;
#20457 = VERTEX_POINT ( 'NONE', #22361 ) ;
#20458 = B_SPLINE_CURVE_WITH_KNOTS ( 'NONE', 3,
 ( #445, #20305, #24658, #9785, #27321, #7636 ),
 .UNSPECIFIED., .F., .F.,
 ( 4, 2, 4 ),
 ( 0.000000000000000000, 0.0004335151646191536890, 0.0008670303292383073780 ),
 .UNSPECIFIED. ) ;
#20459 = EDGE_LOOP ( 'NONE', ( #27963, #17083, #27420, #11903 ) ) ;
#20460 = ORIENTED_EDGE ( 'NONE', *, *, #25385, .F. ) ;
#20461 =( BOUNDED_SURFACE ( )  B_SPLINE_SURFACE ( 3, 1, ( 
 ( #14716, #12285 ),
 ( #25548, #1065 ),
 ( #9700, #27243 ),
 ( #14444, #20773 ) ),
 .UNSPECIFIED., .F., .F., .F. ) 
 B_SPLINE_SURFACE_WITH_KNOTS ( ( 4, 4 ),
 ( 2, 2 ),
 ( 0.000000000000000000, 1.000000000000000000 ),
 ( 0.000000000000000000, 1.000000000000000000 ),
 .UNSPECIFIED. ) 
 GEOMETRIC_REPRESENTATION_ITEM ( )  RATIONAL_B_SPLINE_SURFACE ( (
 ( 1.000000000000000000, 1.000000000000000000),
 ( 0.6386103224230302855, 0.9954351624131538845),
 ( 0.6386103224230302855, 0.9954351624131538845),
 ( 1.000000000000000000, 1.000000000000000000) ) ) 
 REPRESENTATION_ITEM ( '' )  SURFACE ( )  );
#20462 = CARTESIAN_POINT ( 'NONE',  ( -25.21435515916025594, 1.749597353048488237E-16, -4.373993382621220594E-17 ) ) ;
#20463 = CARTESIAN_POINT ( 'NONE',  ( -28.13707043255157103, 0.7675454997510209321, 22.88591869784690047 ) ) ;
#20464 = CARTESIAN_POINT ( 'NONE',  ( 109.1592201516379674, 0.002134489919768143857, -0.007566779963325576466 ) ) ;
#20465 = CARTESIAN_POINT ( 'NONE',  ( 32.73300124599734318, 105.8473486001051072, 51.32617430724947383 ) ) ;
#20466 = EDGE_CURVE ( 'NONE', #15825, #4812, #1023, .T. ) ;
#20467 = EDGE_CURVE ( 'NONE', #16400, #14717, #3410, .T. ) ;
#20468 = CARTESIAN_POINT ( 'NONE',  ( 2.430230287190592531, 126.7388733285345097, 71.49654683843552050 ) ) ;
#20469 = LINE ( 'NONE', #16586, #8765 ) ;
#20470 = CARTESIAN_POINT ( 'NONE',  ( 10.93730112725932813, 150.7858122213658305, 10.89264110825069132 ) ) ;
#20471 = EDGE_CURVE ( 'NONE', #18577, #6221, #7942, .T. ) ;
#20472 = CARTESIAN_POINT ( 'NONE',  ( 25.65782528836481546, -35.44279022896562026, 107.2118488517899664 ) ) ;
#20473 = B_SPLINE_CURVE_WITH_KNOTS ( 'NONE', 3,
 ( #3027, #11804, #20575, #856, #18406, #27183, #17830, #26615, #4750, #13525 ),
 .UNSPECIFIED., .F., .F.,
 ( 4, 3, 3, 4 ),
 ( 1.040834085586084257E-17, 0.0002669560319015708998, 0.0005492286108966411284, 0.0008315040496093379589 ),
 .UNSPECIFIED. ) ;
#20474 = LINE ( 'NONE', #25383, #14328 ) ;
#20475 = CARTESIAN_POINT ( 'NONE',  ( 30.58324630866341565, 3.944468862007675103, 120.8793175557614745 ) ) ;
#20476 = CARTESIAN_POINT ( 'NONE',  ( 1.833206308920085181, 108.3342547309378006, -96.54250175814011925 ) ) ;
#20477 = EDGE_CURVE ( 'NONE', #27511, #13048, #4766, .T. ) ;
#20478 = CARTESIAN_POINT ( 'NONE',  ( -10.86508079875779842, 36.95527278096579948, 35.35100740321738044 ) ) ;
#20479 = CARTESIAN_POINT ( 'NONE',  ( 32.73300124599732186, 0.000000000000000000, 0.000000000000000000 ) ) ;
#20480 = CARTESIAN_POINT ( 'NONE',  ( -1.050230347699842692, 5.964912479342754695E-15, -45.79907861674080749 ) ) ;
#20481 = CARTESIAN_POINT ( 'NONE',  ( 26.04756280548352265, -83.36043467252073924, 76.55292122840010904 ) ) ;
#20482 = CARTESIAN_POINT ( 'NONE',  ( -1.045287976400362417, -1.530335034933495653, 45.76855895860946788 ) ) ;
#20483 = CARTESIAN_POINT ( 'NONE',  ( 28.37599760073041466, -78.09498850373461210, 84.05168479399063131 ) ) ;
#20484 = CARTESIAN_POINT ( 'NONE',  ( 109.1778270068192853, 0.001591747944959422253, 0.009177562596826683780 ) ) ;
#20485 = CARTESIAN_POINT ( 'NONE',  ( 2.433796855181233454, -107.1581411821792216, 98.43889364293823974 ) ) ;
#20486 = ORIENTED_EDGE ( 'NONE', *, *, #3305, .F. ) ;
#20487 = CARTESIAN_POINT ( 'NONE',  ( 26.28373643307413232, 30.57614217577458149, 123.8418562193897543 ) ) ;
#20488 = ORIENTED_EDGE ( 'NONE', *, *, #11370, .F. ) ;
#20489 = CARTESIAN_POINT ( 'NONE',  ( 1.833485406944057594, -84.86072343962649711, 117.7091014914947209 ) ) ;
#20490 = CARTESIAN_POINT ( 'NONE',  ( 2.433796855181205476, 1.451562450951669803, -145.5024947199069345 ) ) ;
#20491 = EDGE_LOOP ( 'NONE', ( #1207, #9209 ) ) ;
#20492 = ORIENTED_EDGE ( 'NONE', *, *, #4327, .F. ) ;
#20493 = VERTEX_POINT ( 'NONE', #21922 ) ;
#20494 = CARTESIAN_POINT ( 'NONE',  ( 6.224689322667647851, 18.02516478984143333, 146.9579047224770250 ) ) ;
#20495 = EDGE_CURVE ( 'NONE', #19910, #9180, #1348, .T. ) ;
#20496 =( BOUNDED_SURFACE ( )  B_SPLINE_SURFACE ( 3, 1, ( 
 ( #6637, #6498 ),
 ( #19714, #6782 ),
 ( #17273, #4457 ),
 ( #25934, #12816 ) ),
 .UNSPECIFIED., .F., .F., .F. ) 
 B_SPLINE_SURFACE_WITH_KNOTS ( ( 4, 4 ),
 ( 2, 2 ),
 ( 0.000000000000000000, 1.000000000000000000 ),
 ( 0.000000000000000000, 1.000000000000000000 ),
 .UNSPECIFIED. ) 
 GEOMETRIC_REPRESENTATION_ITEM ( )  RATIONAL_B_SPLINE_SURFACE ( (
 ( 1.000000000000000000, 1.000000000000000000),
 ( 0.9956975270656955868, 0.8568959468854907557),
 ( 0.9956975270656955868, 0.8568959468854907557),
 ( 1.000000000000000000, 1.000000000000000000) ) ) 
 REPRESENTATION_ITEM ( '' )  SURFACE ( )  );
#20497 = FACE_OUTER_BOUND ( 'NONE', #115, .T. ) ;
#20498 = CARTESIAN_POINT ( 'NONE',  ( -8.786685647604898008, 48.22796981442765940, -23.24040270374399952 ) ) ;
#20499 = EDGE_CURVE ( 'NONE', #24314, #24512, #20569, .T. ) ;
#20500 = CARTESIAN_POINT ( 'NONE',  ( 9.884929003653626367, 65.04493172071478568, 135.7578851563887952 ) ) ;
#20501 = CARTESIAN_POINT ( 'NONE',  ( 19.66333377628681944, 114.0223162644916215, -77.29039328249528751 ) ) ;
#20502 = DIRECTION ( 'NONE',  ( 0.000000000000000000, 1.000000000000000000, 0.000000000000000000 ) ) ;
#20503 = CARTESIAN_POINT ( 'NONE',  ( 28.43349137099851021, 65.60227321965575698, 105.5221910860617527 ) ) ;
#20504 = FACE_OUTER_BOUND ( 'NONE', #18515, .T. ) ;
#20505 = PRODUCT_DEFINITION_SHAPE ( 'NONE', 'NONE',  #28482 ) ;
#20506 = CARTESIAN_POINT ( 'NONE',  ( 25.81918753295379432, -34.03777907511991430, 107.7789657594973676 ) ) ;
#20507 = CARTESIAN_POINT ( 'NONE',  ( -1.048996300304498419, 0.7649764263858191971, 45.79145529752468491 ) ) ;
#20508 = ORIENTED_EDGE ( 'NONE', *, *, #3454, .T. ) ;
#20509 = EDGE_LOOP ( 'NONE', ( #8706, #10586, #15553, #22820 ) ) ;
#20510 = CARTESIAN_POINT ( 'NONE',  ( 2.430230287190581429, 144.8619874886008461, -13.76600171652495241 ) ) ;
#20511 = CARTESIAN_POINT ( 'NONE',  ( 25.64699802086721547, -91.20712948285704158, 66.55977212001133125 ) ) ;
#20512 = CARTESIAN_POINT ( 'NONE',  ( 109.1589550718174877, 0.005233222325298225036, -0.005477029346537791096 ) ) ;
#20513 = CARTESIAN_POINT ( 'NONE',  ( -1.045287976400383290, -36.12803364096628655, -28.14015102489793918 ) ) ;
#20514 = SURFACE_STYLE_FILL_AREA ( #26979 ) ;
#20515 = CARTESIAN_POINT ( 'NONE',  ( -9.156249394959706578, 24.29252099376491358, -48.78605533024748553 ) ) ;
#20516 = VERTEX_POINT ( 'NONE', #17444 ) ;
#20517 = CARTESIAN_POINT ( 'NONE',  ( 32.73300124599731475, 117.5726003567930036, -3.836798148479248827 ) ) ;
#20518 = CARTESIAN_POINT ( 'NONE',  ( 28.37644542392842695, -46.84227702240702484, -115.1790646972553986 ) ) ;
#20519 = CARTESIAN_POINT ( 'NONE',  ( -7.078251931573400491, 47.71415099571833451, 20.86696228105175166 ) ) ;
#20520 = ORIENTED_EDGE ( 'NONE', *, *, #16287, .T. ) ;
#20521 = CARTESIAN_POINT ( 'NONE',  ( -4.473127245936431073, -45.82513704981557368, -18.25038884639852199 ) ) ;
#20522 = ORIENTED_EDGE ( 'NONE', *, *, #10833, .T. ) ;
#20523 = CARTESIAN_POINT ( 'NONE',  ( 25.65782528836481902, -112.3587790429871518, 11.22838748007579568 ) ) ;
#20524 = B_SPLINE_CURVE_WITH_KNOTS ( 'NONE', 3,
 ( #12263, #1463, #23504, #14840, #1605, #5941 ),
 .UNSPECIFIED., .F., .F.,
 ( 4, 2, 4 ),
 ( 2.168404344971008868E-18, 0.0006311636237756670931, 0.001262327247551332018 ),
 .UNSPECIFIED. ) ;
#20525 = B_SPLINE_CURVE_WITH_KNOTS ( 'NONE', 3,
 ( #16380, #838, #2860, #11638, #20413, #9622, #696, #16091 ),
 .UNSPECIFIED., .F., .F.,
 ( 4, 2, 2, 4 ),
 ( 2.225109362706117716E-16, 0.002761568181852862899, 0.005523136363705503753, 0.01104627272741078893 ),
 .UNSPECIFIED. ) ;
#20526 = B_SPLINE_CURVE_WITH_KNOTS ( 'NONE', 3,
 ( #17746, #8843, #15292, #474 ),
 .UNSPECIFIED., .F., .F.,
 ( 4, 4 ),
 ( 0.000000000000000000, 0.008383560773332729421 ),
 .UNSPECIFIED. ) ;
#20527 = ORIENTED_EDGE ( 'NONE', *, *, #8118, .T. ) ;
#20528 = CARTESIAN_POINT ( 'NONE',  ( 55.79472521941426777, 69.41463258328542452, -21.78881894124631913 ) ) ;
#20529 = ORIENTED_EDGE ( 'NONE', *, *, #13341, .F. ) ;
#20530 = EDGE_CURVE ( 'NONE', #23146, #6702, #21592, .T. ) ;
#20531 = ORIENTED_EDGE ( 'NONE', *, *, #681, .T. ) ;
#20532 = CARTESIAN_POINT ( 'NONE',  ( 825.8814872879997893, 950.5262624572890218, 1447.888130612201621 ) ) ;
#20533 = CARTESIAN_POINT ( 'NONE',  ( -20.20898977204109670, 0.6607022527616891461, -29.59696883073212348 ) ) ;
#20534 =( BOUNDED_SURFACE ( )  B_SPLINE_SURFACE ( 3, 1, ( 
 ( #2422, #275 ),
 ( #17819, #26605 ),
 ( #6913, #24474 ),
 ( #4739, #13513 ) ),
 .UNSPECIFIED., .F., .F., .F. ) 
 B_SPLINE_SURFACE_WITH_KNOTS ( ( 4, 4 ),
 ( 2, 2 ),
 ( 0.000000000000000000, 1.000000000000000000 ),
 ( 0.000000000000000000, 1.000000000000000000 ),
 .UNSPECIFIED. ) 
 GEOMETRIC_REPRESENTATION_ITEM ( )  RATIONAL_B_SPLINE_SURFACE ( (
 ( 1.000000000000000000, 1.000000000000000000),
 ( 0.9960225298536222738, 0.9999952330161893110),
 ( 0.9960225298536222738, 0.9999952330161893110),
 ( 1.000000000000000000, 1.000000000000000000) ) ) 
 REPRESENTATION_ITEM ( '' )  SURFACE ( )  );
#20535 = EDGE_CURVE ( 'NONE', #11485, #24558, #3391, .T. ) ;
#20536 = CARTESIAN_POINT ( 'NONE',  ( 109.1586059443104944, -0.005983234375914175257, 0.003774052605966610619 ) ) ;
#20537 = CARTESIAN_POINT ( 'NONE',  ( 32.73300124599731475, 117.5726003567930178, 3.836798148479249715 ) ) ;
#20538 = CARTESIAN_POINT ( 'NONE',  ( -19.53423201713129842, 1.355459634611817431E-16, -3.388649086529543578E-17 ) ) ;
#20539 = EDGE_CURVE ( 'NONE', #119, #12354, #321, .T. ) ;
#20540 = ORIENTED_EDGE ( 'NONE', *, *, #27775, .F. ) ;
#20541 = CARTESIAN_POINT ( 'NONE',  ( 109.1721716018069657, 0.01673651515803009984, 0.003350975118864233521 ) ) ;
#20542 = CARTESIAN_POINT ( 'NONE',  ( 26.04756280548352620, 33.91579348271660876, -107.9769918539636677 ) ) ;
#20543 = VECTOR ( 'NONE', #8048, 1000.000000000000000 ) ;
#20544 = CARTESIAN_POINT ( 'NONE',  ( 13.84597867724983367, -20.08297016719483352, 145.3211459389822267 ) ) ;
#20545 = VERTEX_POINT ( 'NONE', #13851 ) ;
#20546 = ORIENTED_EDGE ( 'NONE', *, *, #2134, .F. ) ;
#20547 = ORIENTED_EDGE ( 'NONE', *, *, #1745, .T. ) ;
#20548 = CARTESIAN_POINT ( 'NONE',  ( -1.050231094221214079, 37.20185272688497236, 26.71409683968576942 ) ) ;
#20549 = ADVANCED_FACE ( 'NONE', ( #22659 ), #19537, .F. ) ;
#20551 = CARTESIAN_POINT ( 'NONE',  ( 25.64708010899963142, 11.74803558238434853, -112.2984447178532434 ) ) ;
#20550 = CARTESIAN_POINT ( 'NONE',  ( 32.73300124599735739, 39.98094346392311138, 110.6325518752275485 ) ) ;
#20552 = B_SPLINE_CURVE_WITH_KNOTS ( 'NONE', 3,
 ( #10480, #12757, #1680, #17084, #8185, #27888, #10614 ),
 .UNSPECIFIED., .F., .F.,
 ( 4, 3, 4 ),
 ( 0.000000000000000000, 0.006568092053401776258, 0.02506242213020846987 ),
 .UNSPECIFIED. ) ;
#20553 = CARTESIAN_POINT ( 'NONE',  ( 25.64681081121879203, -102.9795863647031666, 46.30456157731292421 ) ) ;
#20554 = FACE_OUTER_BOUND ( 'NONE', #25573, .T. ) ;
#20555 = CARTESIAN_POINT ( 'NONE',  ( 26.11404676487259024, 10.71016160607717538, -112.7148551500679332 ) ) ;
#20556 = CARTESIAN_POINT ( 'NONE',  ( 10.93730112725990011, -151.0983828010092225, 4.928439153519769356 ) ) ;
#20557 = ORIENTED_EDGE ( 'NONE', *, *, #19850, .F. ) ;
#20558 = CARTESIAN_POINT ( 'NONE',  ( 32.73300124599740002, -110.6325518752271080, -39.98094346392423404 ) ) ;
#20559 = CARTESIAN_POINT ( 'NONE',  ( 1.831572820252008738, 43.90210991190623702, 138.3111855986062437 ) ) ;
#20560 = CARTESIAN_POINT ( 'NONE',  ( 25.64681081121880624, 12.21581276189807497, 112.2483031020013868 ) ) ;
#20561 = CARTESIAN_POINT ( 'NONE',  ( 1.831572820252008738, -73.40899645746092972, 125.1738732943807690 ) ) ;
#20562 = CARTESIAN_POINT ( 'NONE',  ( -28.41354790283022069, -5.969609727608182759, -22.41474081377998218 ) ) ;
#20563 = CARTESIAN_POINT ( 'NONE',  ( 10.93730112725939030, 140.0398180619108075, 56.95489579269806057 ) ) ;
#20564 = VERTEX_POINT ( 'NONE', #23088 ) ;
#20565 = CARTESIAN_POINT ( 'NONE',  ( 109.1624594426973260, -0.01405141589343899405, 0.007576898892904823310 ) ) ;
#20566 = CARTESIAN_POINT ( 'NONE',  ( 1.833838848569443014, -30.34409872482129344, -141.9017642089167737 ) ) ;
#20567 = CARTESIAN_POINT ( 'NONE',  ( -8.786685647604885574, 6.096987947571466530E-17, -1.524246986892866633E-17 ) ) ;
#20568 = VERTEX_POINT ( 'NONE', #24815 ) ;
#20569 = B_SPLINE_CURVE_WITH_KNOTS ( 'NONE', 3,
 ( #20179, #24238, #20039, #11130, #11551, #15871, #13701 ),
 .UNSPECIFIED., .F., .F.,
 ( 4, 3, 4 ),
 ( 0.000000000000000000, 0.02398743853561383088, 0.04000277880656213925 ),
 .UNSPECIFIED. ) ;
#20570 = ORIENTED_EDGE ( 'NONE', *, *, #13704, .T. ) ;
#20571 = EDGE_CURVE ( 'NONE', #14717, #20645, #9938, .T. ) ;
#20572 = ORIENTED_EDGE ( 'NONE', *, *, #10774, .F. ) ;
#20573 = EDGE_CURVE ( 'NONE', #18502, #13492, #26073, .T. ) ;
#20574 = CARTESIAN_POINT ( 'NONE',  ( -1.048994561756802169, 45.79144455904140898, 0.7655149579825029083 ) ) ;
#20575 = CARTESIAN_POINT ( 'NONE',  ( 25.64699802086723324, -23.70809581152530043, -110.3941571196683640 ) ) ;
#20576 = CARTESIAN_POINT ( 'NONE',  ( 109.1778270068192853, 0.007736698406806029153, -0.005186985107080967217 ) ) ;
#20577 = CARTESIAN_POINT ( 'NONE',  ( 25.98107933586756246, 112.3948402207508650, 12.91054317625147796 ) ) ;
#20578 = CARTESIAN_POINT ( 'NONE',  ( -4.162674018437153123, 47.46216648493558665, -11.82104147411576989 ) ) ;
#20579 = VERTEX_POINT ( 'NONE', #12136 ) ;
#20580 = CARTESIAN_POINT ( 'NONE',  ( 25.98107933586720719, 67.37827847766638456, -90.88151529733718803 ) ) ;
#20581 = FACE_OUTER_BOUND ( 'NONE', #2023, .T. ) ;
#20582 = CARTESIAN_POINT ( 'NONE',  ( 10.93730112725932635, 0.000000000000000000, 0.000000000000000000 ) ) ;
#20583 = ORIENTED_EDGE ( 'NONE', *, *, #21634, .T. ) ;
#20584 = EDGE_LOOP ( 'NONE', ( #25932, #16370 ) ) ;
#20585 = CARTESIAN_POINT ( 'NONE',  ( 13.36082413113061307, -127.3428651193253813, 84.67697637120370757 ) ) ;
#20586 = CARTESIAN_POINT ( 'NONE',  ( 10.93730112725991432, -71.28103789254845424, -133.3192575531807620 ) ) ;
#20587 = CARTESIAN_POINT ( 'NONE',  ( 109.1586900883932856, 0.007109207791181753125, -0.0006456433529162725928 ) ) ;
#20588 = DIRECTION ( 'NONE',  ( 0.5946245182733608248, -0.6948076064830658316, -0.4045541647807455732 ) ) ;
#20589 = CARTESIAN_POINT ( 'NONE',  ( 2.063896406836605024, 137.7380992975102743, 46.16709813092669634 ) ) ;
#20590 = CARTESIAN_POINT ( 'NONE',  ( 2.433796855181205476, -145.5024947199069629, -1.451562450951161987 ) ) ;
#20591 = ORIENTED_EDGE ( 'NONE', *, *, #721, .T. ) ;
#20592 = CARTESIAN_POINT ( 'NONE',  ( 1.833485406944043827, -132.3460930279895535, 59.50871042846178938 ) ) ;
#20593 = CARTESIAN_POINT ( 'NONE',  ( -20.20700224038492721, -24.51628800869035274, 16.58740185276737122 ) ) ;
#20594 = CARTESIAN_POINT ( 'NONE',  ( 25.86096068574579832, -65.64181925268263740, -92.04529103340848906 ) ) ;
#20595 = LINE ( 'NONE', #27502, #14413 ) ;
#20596 =( BOUNDED_SURFACE ( )  B_SPLINE_SURFACE ( 3, 1, ( 
 ( #22013, #4318 ),
 ( #6916, #15823 ),
 ( #24476, #19996 ),
 ( #24632, #2275 ) ),
 .UNSPECIFIED., .F., .F., .F. ) 
 B_SPLINE_SURFACE_WITH_KNOTS ( ( 4, 4 ),
 ( 2, 2 ),
 ( 0.000000000000000000, 1.000000000000000000 ),
 ( 0.000000000000000000, 1.000000000000000000 ),
 .UNSPECIFIED. ) 
 GEOMETRIC_REPRESENTATION_ITEM ( )  RATIONAL_B_SPLINE_SURFACE ( (
 ( 1.000000000000000000, 1.000000000000000000),
 ( 0.9593753223639863714, 0.9995975284513187731),
 ( 0.9593753223639863714, 0.9995975284513187731),
 ( 1.000000000000000000, 1.000000000000000000) ) ) 
 REPRESENTATION_ITEM ( '' )  SURFACE ( )  );
#20597 = CARTESIAN_POINT ( 'NONE',  ( -55.24198130335446422, -0.008252882783648586573, -0.004276389980780055493 ) ) ;
#20598 = ORIENTED_EDGE ( 'NONE', *, *, #20796, .F. ) ;
#20599 = CARTESIAN_POINT ( 'NONE',  ( 1.832998868059890096, -132.7810136645734360, -58.53348008137779601 ) ) ;
#20600 = ORIENTED_EDGE ( 'NONE', *, *, #19473, .F. ) ;
#20601 = ORIENTED_EDGE ( 'NONE', *, *, #6868, .T. ) ;
#20602 = EDGE_CURVE ( 'NONE', #12090, #9124, #16443, .T. ) ;
#20603 = ORIENTED_EDGE ( 'NONE', *, *, #7756, .T. ) ;
#20604 = FACE_OUTER_BOUND ( 'NONE', #291, .T. ) ;
#20605 = ADVANCED_FACE ( 'NONE', ( #18745 ), #1477, .T. ) ;
#20606 = CARTESIAN_POINT ( 'NONE',  ( 1.831572820252008738, -108.4969585352561410, 96.36280042115893707 ) ) ;
#20607 = CARTESIAN_POINT ( 'NONE',  ( -55.24271866751342941, 0.004365563123939763222, -0.008433070970614044842 ) ) ;
#20608 = CARTESIAN_POINT ( 'NONE',  ( 6.224689322667647851, -108.2965163446081078, 100.9623537450648172 ) ) ;
#20609 = CARTESIAN_POINT ( 'NONE',  ( 2.433796855181219243, -13.76554153471791864, 144.8571464219888583 ) ) ;
#20610 = CARTESIAN_POINT ( 'NONE',  ( -21.81686047589431965, 5.181745222995449929, -38.17230180719251820 ) ) ;
#20611 = CARTESIAN_POINT ( 'NONE',  ( -1.463510566862834761, -16.57250862017389892, 43.13857742234520032 ) ) ;
#20612 = CARTESIAN_POINT ( 'NONE',  ( -1.019300379054419725, 45.76814864815091255, -2.023851374322835017 ) ) ;
#20613 = FACE_OUTER_BOUND ( 'NONE', #12260, .T. ) ;
#20614 = EDGE_CURVE ( 'NONE', #23277, #21774, #16590, .T. ) ;
#20615 = CARTESIAN_POINT ( 'NONE',  ( -20.57838717382308147, -27.96569011373078339, 10.78122205917029675 ) ) ;
#20616 = CARTESIAN_POINT ( 'NONE',  ( -20.21097721712959228, -28.26295595852180043, 8.835581498567762537 ) ) ;
#20617 = CIRCLE ( 'NONE', #22951, 117.6351876552689504 ) ;
#20618 = CARTESIAN_POINT ( 'NONE',  ( 25.86096068574578766, -55.66087367585338797, -98.40249579084571963 ) ) ;
#20619 = CARTESIAN_POINT ( 'NONE',  ( 25.81918753295378366, -83.36706424720497921, 76.32043280377783390 ) ) ;
#20620 = CARTESIAN_POINT ( 'NONE',  ( -1.463510566862821882, -2.430838777909866355, 46.14841196428346848 ) ) ;
#20621 = CARTESIAN_POINT ( 'NONE',  ( 55.49584447822657296, -58.85239198729157550, -42.42793568433017981 ) ) ;
#20622 = CARTESIAN_POINT ( 'NONE',  ( -1.031422197589716205, -1.530725436377772031, -45.78027046666443312 ) ) ;
#20623 = CARTESIAN_POINT ( 'NONE',  ( 10.93730112725990189, -148.8212007290660495, -26.59437931460901439 ) ) ;
#20624 = ORIENTED_EDGE ( 'NONE', *, *, #20198, .F. ) ;
#20625 = LINE ( 'NONE', #6983, #13413 ) ;
#20626 =( BOUNDED_SURFACE ( )  B_SPLINE_SURFACE ( 3, 1, ( 
 ( #22303, #20125 ),
 ( #2565, #8772 ),
 ( #7056, #13355 ),
 ( #410, #9192 ) ),
 .UNSPECIFIED., .F., .F., .F. ) 
 B_SPLINE_SURFACE_WITH_KNOTS ( ( 4, 4 ),
 ( 2, 2 ),
 ( 0.000000000000000000, 1.000000000000000000 ),
 ( 0.000000000000000000, 1.000000000000000000 ),
 .UNSPECIFIED. ) 
 GEOMETRIC_REPRESENTATION_ITEM ( )  RATIONAL_B_SPLINE_SURFACE ( (
 ( 1.000000000000000000, 1.000000000000000000),
 ( 0.9956975270656954757, 0.8568959468854893125),
 ( 0.9956975270656954757, 0.8568959468854893125),
 ( 1.000000000000000000, 1.000000000000000000) ) ) 
 REPRESENTATION_ITEM ( '' )  SURFACE ( )  );
#20627 = EDGE_CURVE ( 'NONE', #7617, #13959, #20474, .T. ) ;
#20628 = ORIENTED_EDGE ( 'NONE', *, *, #14655, .F. ) ;
#20629 = FACE_OUTER_BOUND ( 'NONE', #5398, .T. ) ;
#20630 = CARTESIAN_POINT ( 'NONE',  ( 109.1592201516379674, -0.005027640251764426034, 0.006044422199831456753 ) ) ;
#20631 = ORIENTED_EDGE ( 'NONE', *, *, #12317, .F. ) ;
#20632 = EDGE_CURVE ( 'NONE', #4332, #26927, #18456, .T. ) ;
#20633 = VERTEX_POINT ( 'NONE', #7542 ) ;
#20634 = ORIENTED_EDGE ( 'NONE', *, *, #746, .F. ) ;
#20635 = EDGE_CURVE ( 'NONE', #15678, #4919, #6161, .T. ) ;
#20636 = CARTESIAN_POINT ( 'NONE',  ( 109.1587776205901861, -0.0006832286435017355386, 0.007297420966932444478 ) ) ;
#20637 = EDGE_CURVE ( 'NONE', #7936, #23571, #26940, .T. ) ;
#20638 = DIRECTION ( 'NONE',  ( 0.7563875759206387661, -0.6320336713238486892, 0.1685564395263406956 ) ) ;
#20639 = DIRECTION ( 'NONE',  ( -1.000000000000000000, -0.000000000000000000, -0.000000000000000000 ) ) ;
#20640 = CARTESIAN_POINT ( 'NONE',  ( -5.986830583229461489, 46.64941882410799678, -19.95149887249867859 ) ) ;
#20641 = CARTESIAN_POINT ( 'NONE',  ( 55.49584447822657296, -22.16497542184453451, 69.08290406177572152 ) ) ;
#20642 = DIRECTION ( 'NONE',  ( 0.000000000000000000, 5.223019709708233256E-21, -1.000000000000000000 ) ) ;
#20643 = CARTESIAN_POINT ( 'NONE',  ( 1.833721034905660741, -59.34646046113689977, -132.4192200895888050 ) ) ;
#20644 = CARTESIAN_POINT ( 'NONE',  ( 25.64670758986456889, 83.57526425215496602, 75.92149922855223565 ) ) ;
#20645 = VERTEX_POINT ( 'NONE', #8246 ) ;
#20646 = EDGE_LOOP ( 'NONE', ( #11814, #22794, #12203, #1655 ) ) ;
#20647 = CARTESIAN_POINT ( 'NONE',  ( -8.786685647604890903, -25.35688121747466184, 47.14957014837381166 ) ) ;
#20649 = CARTESIAN_POINT ( 'NONE',  ( 5.340103579038300019, 57.86178752084676091, -135.6222865281523582 ) ) ;
#20648 = CARTESIAN_POINT ( 'NONE',  ( 25.64699802086725811, 66.17503410044022871, -91.48665801621594085 ) ) ;
#20650 = CARTESIAN_POINT ( 'NONE',  ( -18.41936578851711204, -7.566034416291083531, -41.75701384111729197 ) ) ;
#20651 = LINE ( 'NONE', #24722, #25825 ) ;
#20652 = CARTESIAN_POINT ( 'NONE',  ( 2.263178113027022764, -71.48082833564976113, -126.6115605262345980 ) ) ;
#20653 = ORIENTED_EDGE ( 'NONE', *, *, #347, .T. ) ;
#20654 = CARTESIAN_POINT ( 'NONE',  ( 25.64681081121879203, 97.99105938548001404, -56.09509703373240797 ) ) ;
#20655 = CARTESIAN_POINT ( 'NONE',  ( -1.239374126674604337, 2.406737988131765871, 45.98822239537605583 ) ) ;
#20656 = CARTESIAN_POINT ( 'NONE',  ( -1.619063947482197729, -38.92136151114888776, 25.20140673341416360 ) ) ;
#20657 = VERTEX_POINT ( 'NONE', #5808 ) ;
#20658 = CARTESIAN_POINT ( 'NONE',  ( 55.49584447822657296, -36.04376091928588721, 62.96491934285981529 ) ) ;
#20659 = ADVANCED_FACE ( 'NONE', ( #25671 ), #18946, .T. ) ;
#20660 = ORIENTED_EDGE ( 'NONE', *, *, #13875, .F. ) ;
#20661 = CARTESIAN_POINT ( 'NONE',  ( 1.833206310202331935, 116.9567751109830596, -85.89457578512693203 ) ) ;
#20662 = EDGE_CURVE ( 'NONE', #6495, #25074, #8381, .T. ) ;
#20663 = CARTESIAN_POINT ( 'NONE',  ( -1.044557008772710072, 45.76404748504490527, 1.643388457098048372 ) ) ;
#20664 =( BOUNDED_SURFACE ( )  B_SPLINE_SURFACE ( 3, 1, ( 
 ( #9756, #20829 ),
 ( #14340, #10045 ),
 ( #7900, #3414 ),
 ( #25456, #5730 ) ),
 .UNSPECIFIED., .F., .F., .F. ) 
 B_SPLINE_SURFACE_WITH_KNOTS ( ( 4, 4 ),
 ( 2, 2 ),
 ( 0.000000000000000000, 1.000000000000000000 ),
 ( 0.000000000000000000, 1.000000000000000000 ),
 .UNSPECIFIED. ) 
 GEOMETRIC_REPRESENTATION_ITEM ( )  RATIONAL_B_SPLINE_SURFACE ( (
 ( 1.000000000000000000, 1.000000000000000000),
 ( 0.9956975270656954757, 0.8568959468854893125),
 ( 0.9956975270656954757, 0.8568959468854893125),
 ( 1.000000000000000000, 1.000000000000000000) ) ) 
 REPRESENTATION_ITEM ( '' )  SURFACE ( )  );
#20665 = ORIENTED_EDGE ( 'NONE', *, *, #21996, .T. ) ;
#20666 = CARTESIAN_POINT ( 'NONE',  ( -1.031422197589711987, 36.13727897780127307, -28.14735071801756661 ) ) ;
#20667 = ORIENTED_EDGE ( 'NONE', *, *, #22034, .F. ) ;
#20668 = CARTESIAN_POINT ( 'NONE',  ( -23.79248802219731118, 28.61009539422409631, 16.82188324679449565 ) ) ;
#20669 = CARTESIAN_POINT ( 'NONE',  ( -1.619063947482201282, -44.80407745103776307, 11.94059994246206635 ) ) ;
#20670 = B_SPLINE_CURVE_WITH_KNOTS ( 'NONE', 3,
 ( #5319, #575, #15971, #5026, #11662, #22909, #25193 ),
 .UNSPECIFIED., .F., .F.,
 ( 4, 3, 4 ),
 ( 0.000000000000000000, 0.02398743853561357067, 0.04000277880656220864 ),
 .UNSPECIFIED. ) ;
#20671 = VERTEX_POINT ( 'NONE', #19453 ) ;
#20672 = SHAPE_REPRESENTATION_RELATIONSHIP ( 'NONE' , 'NONE' ,  #747, #24076 ) ;
#20673 = CARTESIAN_POINT ( 'NONE',  ( -55.24271866751342941, -0.004256484107792932181, -0.008488649505346277865 ) ) ;
#20674 = CARTESIAN_POINT ( 'NONE',  ( 9.884929003653608603, -91.84919534722023116, 119.2676479132370702 ) ) ;
#20675 = CARTESIAN_POINT ( 'NONE',  ( 1.833809397011890940, 0.1779683723495601722, -145.1096615925544882 ) ) ;
#20676 = CARTESIAN_POINT ( 'NONE',  ( 2.433796855181219243, -142.0211193075558356, 31.67151202412923894 ) ) ;
#20677 = VERTEX_POINT ( 'NONE', #3774 ) ;
#20678 = CARTESIAN_POINT ( 'NONE',  ( -9.156249394959706578, 53.74753343182702991, -9.022661520477960551 ) ) ;
#20680 = CARTESIAN_POINT ( 'NONE',  ( -9.156249394959706578, -48.32878616080991208, 25.18996226954667605 ) ) ;
#20679 = CARTESIAN_POINT ( 'NONE',  ( 99.22246935314079508, -90.00000000000005684, -40.00000000000002842 ) ) ;
#20681 = CARTESIAN_POINT ( 'NONE',  ( -20.38016308990358638, 23.16952666206584155, -18.69911008768343663 ) ) ;
#20682 = ORIENTED_EDGE ( 'NONE', *, *, #26121, .F. ) ;
#20683 = EDGE_LOOP ( 'NONE', ( #17172, #6668, #22608, #4633 ) ) ;
#20684 = ORIENTED_EDGE ( 'NONE', *, *, #20019, .T. ) ;
#20685 = CARTESIAN_POINT ( 'NONE',  ( -1.046935749539997129, 36.28605774377803073, 27.93995161054655085 ) ) ;
#20686 = DIRECTION ( 'NONE',  ( -1.000000000000000000, -0.000000000000000000, -0.000000000000000000 ) ) ;
#20688 = CARTESIAN_POINT ( 'NONE',  ( 8.186469829614452465, 49.43817854882515661, -140.9315935955036423 ) ) ;
#20687 = CARTESIAN_POINT ( 'NONE',  ( 2.430230287190592531, -74.01081053031012402, -125.2872625092170153 ) ) ;
#20689 = CARTESIAN_POINT ( 'NONE',  ( -8.786685647604890903, -48.22796981442753150, 23.24040270374441874 ) ) ;
#20690 = CARTESIAN_POINT ( 'NONE',  ( -12.82751273423876270, 48.43568301531151121, -6.573887447703007147 ) ) ;
#20691 = CARTESIAN_POINT ( 'NONE',  ( 30.59138290137910587, 9.457588828076605836, -115.8270707793591185 ) ) ;
#20692 = CARTESIAN_POINT ( 'NONE',  ( 5.340103556456419653, -88.52145167812672355, 117.9209211572682818 ) ) ;
#20693 = VERTEX_POINT ( 'NONE', #17153 ) ;
#20694 = CARTESIAN_POINT ( 'NONE',  ( -1.045287976400365970, 15.59869763335156101, 43.05558670614217931 ) ) ;
#20695 = CARTESIAN_POINT ( 'NONE',  ( -55.24390624410018802, 0.001451500391951047672, 0.01032895241566990016 ) ) ;
#20696 = DIRECTION ( 'NONE',  ( 0.000000000000000000, 0.000000000000000000, 1.000000000000000000 ) ) ;
#20697 = CARTESIAN_POINT ( 'NONE',  ( 25.87036335909426299, -67.25332031939082356, -90.88222105969130382 ) ) ;
#20698 = CIRCLE ( 'NONE', #5073, 53.53553390275978785 ) ;
#20699 = CARTESIAN_POINT ( 'NONE',  ( 1.834118845439484335, 107.7186227765467237, -97.22976650547319366 ) ) ;
#20700 = CARTESIAN_POINT ( 'NONE',  ( 109.1592201516379674, 0.007051465909552763651, -0.003476928926134732496 ) ) ;
#20701 = EDGE_CURVE ( 'NONE', #28132, #17753, #24456, .T. ) ;
#20702 = CIRCLE ( 'NONE', #17454, 117.6351876552689504 ) ;
#20703 = ORIENTED_EDGE ( 'NONE', *, *, #18040, .T. ) ;
#20704 = CARTESIAN_POINT ( 'NONE',  ( 109.1592201516379674, 0.007620268632968142664, 0.001934867487012853927 ) ) ;
#20705 = AXIS2_PLACEMENT_3D ( 'NONE', #12325, #15321, #13035 ) ;
#20706 = CARTESIAN_POINT ( 'NONE',  ( -15.02187109954784106, 45.60876405941888123, -8.264310930412539946 ) ) ;
#20707 = ADVANCED_FACE ( 'NONE', ( #10685 ), #12875, .F. ) ;
#20708 = B_SPLINE_CURVE_WITH_KNOTS ( 'NONE', 3,
 ( #27444, #5872, #23295, #8045, #20962, #5576, #1118, #22873, #16514, #3133, #11910, #3417, #9762 ),
 .UNSPECIFIED., .F., .F.,
 ( 4, 3, 3, 3, 4 ),
 ( 6.938893903907227607E-18, 0.0007657099931970539480, 0.001531419946797919806, 0.002296279302920154267, 0.003061450627205759834 ),
 .UNSPECIFIED. ) ;
#20709 = CARTESIAN_POINT ( 'NONE',  ( 109.1592201516379674, 0.0005146241775907373474, -0.007845213074660002325 ) ) ;
#20710 = EDGE_CURVE ( 'NONE', #23443, #3658, #18158, .T. ) ;
#20711 = ORIENTED_EDGE ( 'NONE', *, *, #12316, .F. ) ;
#20712 = ORIENTED_EDGE ( 'NONE', *, *, #9342, .F. ) ;
#20713 =( BOUNDED_SURFACE ( )  B_SPLINE_SURFACE ( 3, 1, ( 
 ( #5757, #25182 ),
 ( #16245, #7781 ),
 ( #14212, #9931 ),
 ( #20700, #7928 ) ),
 .UNSPECIFIED., .F., .F., .F. ) 
 B_SPLINE_SURFACE_WITH_KNOTS ( ( 4, 4 ),
 ( 2, 2 ),
 ( 0.000000000000000000, 1.000000000000000000 ),
 ( 0.000000000000000000, 1.000000000000000000 ),
 .UNSPECIFIED. ) 
 GEOMETRIC_REPRESENTATION_ITEM ( )  RATIONAL_B_SPLINE_SURFACE ( (
 ( 1.000000000000000000, 1.000000000000000000),
 ( 0.9956975270656955868, 0.8568959468854907557),
 ( 0.9956975270656955868, 0.8568959468854907557),
 ( 1.000000000000000000, 1.000000000000000000) ) ) 
 REPRESENTATION_ITEM ( '' )  SURFACE ( )  );
#20714 = CARTESIAN_POINT ( 'NONE',  ( -1.056502255334265339, 27.33667001641170557, -36.75727364034741385 ) ) ;
#20715 = CARTESIAN_POINT ( 'NONE',  ( 26.11404676487257603, -102.9690087468804762, 47.08215554553482463 ) ) ;
#20716 = CARTESIAN_POINT ( 'NONE',  ( -20.57838717382308147, -28.96176188950224528, -7.715628353033566533 ) ) ;
#20717 = CARTESIAN_POINT ( 'NONE',  ( 16.75465622695656265, -79.80233222761923173, -117.7275519421685459 ) ) ;
#20718 = CARTESIAN_POINT ( 'NONE',  ( 1.833691583653538126, 125.8462703805709140, -72.24637705290355427 ) ) ;
#20719 = ORIENTED_EDGE ( 'NONE', *, *, #2868, .F. ) ;
#20720 = CARTESIAN_POINT ( 'NONE',  ( 8.186469777910991397, 84.95702201436577639, -122.8338388711454314 ) ) ;
#20721 = CIRCLE ( 'NONE', #11067, 53.53553390275978785 ) ;
#20722 = EDGE_CURVE ( 'NONE', #25788, #12126, #12547, .T. ) ;
#20723 = CARTESIAN_POINT ( 'NONE',  ( 1.833206308920100724, -116.9567745381553436, -85.89457656603988767 ) ) ;
#20724 = VERTEX_POINT ( 'NONE', #28220 ) ;
#20725 = VECTOR ( 'NONE', #24838, 999.9999999999998863 ) ;
#20726 = ORIENTED_EDGE ( 'NONE', *, *, #21964, .T. ) ;
#20727 = CARTESIAN_POINT ( 'NONE',  ( -25.21435515916042647, 25.00736669481023355, -23.92354251275945742 ) ) ;
#20728 = CARTESIAN_POINT ( 'NONE',  ( 10.93730112725972958, -84.82621002473526062, 125.1380233598475229 ) ) ;
#20729 = CARTESIAN_POINT ( 'NONE',  ( 21.16825799904899341, -83.13600836828936735, -106.9139171613934849 ) ) ;
#20730 = CARTESIAN_POINT ( 'NONE',  ( 32.73300124599735739, 20.69176323058628597, 115.8010721414084543 ) ) ;
#20731 = CARTESIAN_POINT ( 'NONE',  ( 2.263178113027046301, -84.32376073259139559, -118.4461880110611958 ) ) ;
#20732 = EDGE_CURVE ( 'NONE', #19518, #11913, #19859, .T. ) ;
#20733 = CARTESIAN_POINT ( 'NONE',  ( -20.20700224038492721, -23.35150625415645820, 18.19058640100249491 ) ) ;
#20734 = ORIENTED_EDGE ( 'NONE', *, *, #8339, .T. ) ;
#20735 = CARTESIAN_POINT ( 'NONE',  ( 8.186469777910986068, 42.84118569629532658, -143.0750864738772918 ) ) ;
#20736 = CARTESIAN_POINT ( 'NONE',  ( 32.73300124599737870, 20.69176323058787759, -115.8010721414081132 ) ) ;
#20737 = LINE ( 'NONE', #1173, #19320 ) ;
#20738 = EDGE_CURVE ( 'NONE', #4343, #17054, #11656, .T. ) ;
#20739 = CARTESIAN_POINT ( 'NONE',  ( 2.430230287190589422, -60.50928654924667427, -132.3371620660956864 ) ) ;
#20740 = CARTESIAN_POINT ( 'NONE',  ( -1.464342487929850778, 38.76467504336618219, 25.15873223207648834 ) ) ;
#20741 = ORIENTED_EDGE ( 'NONE', *, *, #12962, .T. ) ;
#20742 = ORIENTED_EDGE ( 'NONE', *, *, #18604, .F. ) ;
#20743 = CARTESIAN_POINT ( 'NONE',  ( 26.11404676487257603, 22.43340081644767636, 110.9778746459747794 ) ) ;
#20744 = VERTEX_POINT ( 'NONE', #14701 ) ;
#20745 = VECTOR ( 'NONE', #4730, 999.9999999999998863 ) ;
#20746 = ORIENTED_EDGE ( 'NONE', *, *, #7141, .T. ) ;
#20747 = ORIENTED_EDGE ( 'NONE', *, *, #14886, .F. ) ;
#20748 = VECTOR ( 'NONE', #27716, 999.9999999999998863 ) ;
#20749 = FACE_OUTER_BOUND ( 'NONE', #7681, .T. ) ;
#20750 = CARTESIAN_POINT ( 'NONE',  ( -1.056502255334264895, -43.72121397317232550, -13.66916755949833373 ) ) ;
#20751 = FACE_OUTER_BOUND ( 'NONE', #11914, .T. ) ;
#20752 = CARTESIAN_POINT ( 'NONE',  ( 10.93730112725990367, -145.2260730187398678, -42.00474393596407197 ) ) ;
#20753 = CARTESIAN_POINT ( 'NONE',  ( 2.063896406836605024, 142.3682421260911326, -28.88716984836180401 ) ) ;
#20754 = B_SPLINE_CURVE_WITH_KNOTS ( 'NONE', 3,
 ( #24275, #6578, #22403, #22107 ),
 .UNSPECIFIED., .F., .F.,
 ( 4, 4 ),
 ( 3.389420616900455111E-16, 0.01077107486149848047 ),
 .UNSPECIFIED. ) ;
#20755 = CARTESIAN_POINT ( 'NONE',  ( -1.239374126674604337, 45.98822239537608425, -2.406737988131283146 ) ) ;
#20756 = CARTESIAN_POINT ( 'NONE',  ( 2.433796855181233454, -133.5135467655514390, -57.85512797798025275 ) ) ;
#20757 = VECTOR ( 'NONE', #23308, 1000.000000000000114 ) ;
#20758 = B_SPLINE_CURVE_WITH_KNOTS ( 'NONE', 3,
 ( #10031, #23276, #3529, #23557, #7591, #19083, #25435, #5712, #22993, #25141 ),
 .UNSPECIFIED., .F., .F.,
 ( 4, 3, 3, 4 ),
 ( 3.122502256758252770E-17, 0.0002669559177086242431, 0.0005339118354151079458, 0.001067817517169163816 ),
 .UNSPECIFIED. ) ;
#20759 = ADVANCED_FACE ( 'NONE', ( #1743 ), #22497, .F. ) ;
#20760 = CARTESIAN_POINT ( 'NONE',  ( -25.21435515916043357, 16.39063784838743132, -30.48034229288645136 ) ) ;
#20761 = CARTESIAN_POINT ( 'NONE',  ( 109.1586900883932856, -0.002301750759599821821, 0.006757191295060836940 ) ) ;
#20762 = CARTESIAN_POINT ( 'NONE',  ( 25.64681081121879203, -56.09509703373275613, -97.99105938547980088 ) ) ;
#20763 = ADVANCED_FACE ( 'NONE', ( #27814 ), #18483, .T. ) ;
#20764 = CARTESIAN_POINT ( 'NONE',  ( -28.41354790283022069, 18.00456980371900784, -14.62505768302807319 ) ) ;
#20765 = EDGE_CURVE ( 'NONE', #18556, #4919, #4762, .T. ) ;
#20766 = CARTESIAN_POINT ( 'NONE',  ( -1.058197053496165552, -1.754224732379234153, 45.77356582045592859 ) ) ;
#20767 = CARTESIAN_POINT ( 'NONE',  ( 9.884929003653626367, -97.56484214660700616, 114.6392083957114494 ) ) ;
#20768 = CARTESIAN_POINT ( 'NONE',  ( 2.430230287190592531, 109.1043569252014436, 96.28466919684133529 ) ) ;
#20769 = ORIENTED_EDGE ( 'NONE', *, *, #19202, .T. ) ;
#20770 = LINE ( 'NONE', #14283, #2375 ) ;
#20771 = ORIENTED_EDGE ( 'NONE', *, *, #28000, .F. ) ;
#20772 = CARTESIAN_POINT ( 'NONE',  ( -20.20997486282892552, 1.395963739018065216E-16, 29.60348406988233450 ) ) ;
#20773 = CARTESIAN_POINT ( 'NONE',  ( 13.36082413113061307, -67.94366799842909188, 137.0038452127797939 ) ) ;
#20774 = ORIENTED_EDGE ( 'NONE', *, *, #25404, .T. ) ;
#20775 = ORIENTED_EDGE ( 'NONE', *, *, #6845, .T. ) ;
#20776 = ORIENTED_EDGE ( 'NONE', *, *, #19398, .T. ) ;
#20777 = B_SPLINE_CURVE_WITH_KNOTS ( 'NONE', 3,
 ( #13197, #4147, #15074, #4292, #26442, #25904, #26307 ),
 .UNSPECIFIED., .F., .F.,
 ( 4, 3, 4 ),
 ( 5.762311684337388436E-16, 0.02816610861753244405, 0.04000277880656280538 ),
 .UNSPECIFIED. ) ;
#20778 = B_SPLINE_CURVE_WITH_KNOTS ( 'NONE', 3,
 ( #11470, #27000, #26717, #821, #7034, #22427, #9604, #11906, #20242, #5282 ),
 .UNSPECIFIED., .F., .F.,
 ( 4, 3, 3, 4 ),
 ( 6.938893903907228378E-18, 0.0002669560319015712793, 0.0005492286108966321296, 0.0008315040496093543303 ),
 .UNSPECIFIED. ) ;
#20779 = CIRCLE ( 'NONE', #24478, 53.53553390275978785 ) ;
#20780 = EDGE_LOOP ( 'NONE', ( #26748, #24784, #19434, #15326 ) ) ;
#20781 = CARTESIAN_POINT ( 'NONE',  ( 9.884929003653626367, 19.90991253123246452, 149.2134106160916929 ) ) ;
#20782 = AXIS2_PLACEMENT_3D ( 'NONE', #8908, #12926, #11198 ) ;
#20783 = FACE_OUTER_BOUND ( 'NONE', #17115, .T. ) ;
#20784 = CARTESIAN_POINT ( 'NONE',  ( -55.24390624410018802, -0.004572280736702649152, 0.009374879212966917563 ) ) ;
#20785 = CARTESIAN_POINT ( 'NONE',  ( 2.433796855181205476, -28.83182736670433499, -142.6247129145651229 ) ) ;
#20786 = EDGE_CURVE ( 'NONE', #4626, #8623, #17154, .T. ) ;
#20787 = CARTESIAN_POINT ( 'NONE',  ( -55.24198130335446422, -0.006617369590168513567, -0.006527480770976002225 ) ) ;
#20788 = B_SPLINE_CURVE_WITH_KNOTS ( 'NONE', 3,
 ( #8955, #19727, #24080, #11104, #13538, #19875 ),
 .UNSPECIFIED., .F., .F.,
 ( 4, 2, 4 ),
 ( 0.000000000000000000, 0.0004335184443140234316, 0.0008670368886280468632 ),
 .UNSPECIFIED. ) ;
#20789 = CARTESIAN_POINT ( 'NONE',  ( 1.831572820252008738, 14.18623102066768915, 144.4165162501763575 ) ) ;
#20790 = CARTESIAN_POINT ( 'NONE',  ( 1.832998868059858122, -44.33343224355138545, -138.1720401012271680 ) ) ;
#20791 = CARTESIAN_POINT ( 'NONE',  ( 1.833206308920097616, -85.89457656603950397, 116.9567745381556563 ) ) ;
#20793 = LINE ( 'NONE', #27704, #6555 ) ;
#20792 = CARTESIAN_POINT ( 'NONE',  ( -20.20700224038492365, 10.08426345511628597, 27.82980252387807951 ) ) ;
#20794 = SURFACE_STYLE_FILL_AREA ( #22981 ) ;
#20795 =( BOUNDED_SURFACE ( )  B_SPLINE_SURFACE ( 3, 1, ( 
 ( #19289, #6073 ),
 ( #12665, #12800 ),
 ( #28063, #1860 ),
 ( #25649, #12523 ) ),
 .UNSPECIFIED., .F., .F., .F. ) 
 B_SPLINE_SURFACE_WITH_KNOTS ( ( 4, 4 ),
 ( 2, 2 ),
 ( 0.000000000000000000, 1.000000000000000000 ),
 ( 0.000000000000000000, 1.000000000000000000 ),
 .UNSPECIFIED. ) 
 GEOMETRIC_REPRESENTATION_ITEM ( )  RATIONAL_B_SPLINE_SURFACE ( (
 ( 1.000000000000000000, 1.000000000000000000),
 ( 0.9593753223639863714, 0.9995975284513187731),
 ( 0.9593753223639863714, 0.9995975284513187731),
 ( 1.000000000000000000, 1.000000000000000000) ) ) 
 REPRESENTATION_ITEM ( '' )  SURFACE ( )  );
#20796 = EDGE_CURVE ( 'NONE', #24974, #8000, #5115, .T. ) ;
#20797 = EDGE_LOOP ( 'NONE', ( #3795, #18949, #4689, #3022 ) ) ;
#20798 = ORIENTED_EDGE ( 'NONE', *, *, #7972, .F. ) ;
#20799 = VECTOR ( 'NONE', #22382, 999.9999999999998863 ) ;
#20800 = CARTESIAN_POINT ( 'NONE',  ( 25.64681081121879203, -11.38886654529750331, 112.3352186517030447 ) ) ;
#20802 = CARTESIAN_POINT ( 'NONE',  ( 25.65782528836481902, 75.98558751977886061, -83.52701600504799728 ) ) ;
#20801 = FACE_OUTER_BOUND ( 'NONE', #13360, .T. ) ;
#20803 = CARTESIAN_POINT ( 'NONE',  ( 28.37603512858459354, -108.5491486026793808, 37.15644006762180851 ) ) ;
#20804 = FILL_AREA_STYLE_COLOUR ( '', #13388 ) ;
#20805 = CARTESIAN_POINT ( 'NONE',  ( 1.833485406944043827, 144.3694338680884925, 14.63699153649408480 ) ) ;
#20806 = VECTOR ( 'NONE', #25872, 1000.000000000000000 ) ;
#20807 = EDGE_CURVE ( 'NONE', #6648, #3087, #11376, .T. ) ;
#20808 = ORIENTED_EDGE ( 'NONE', *, *, #12080, .F. ) ;
#20809 = CARTESIAN_POINT ( 'NONE',  ( 1.833809397773888517, 44.67209459545068029, 138.0624841332889332 ) ) ;
#20810 = VECTOR ( 'NONE', #3099, 1000.000000000000227 ) ;
#20811 = FACE_OUTER_BOUND ( 'NONE', #22623, .T. ) ;
#20812 = CARTESIAN_POINT ( 'NONE',  ( -55.24300891470648622, -0.0003472257464243277253, 0.009812809446890398413 ) ) ;
#20813 = EDGE_LOOP ( 'NONE', ( #20540, #1699, #5998, #4369 ) ) ;
#20814 = DIRECTION ( 'NONE',  ( -0.000000000000000000, 1.000000000000000000, -0.000000000000000000 ) ) ;
#20815 = CARTESIAN_POINT ( 'NONE',  ( 26.28373643307402574, -126.3595147275198514, 17.46364395087421073 ) ) ;
#20816 = AXIS2_PLACEMENT_3D ( 'NONE', #22977, #25263, #9865 ) ;
#20817 = ORIENTED_EDGE ( 'NONE', *, *, #6203, .T. ) ;
#20818 = CARTESIAN_POINT ( 'NONE',  ( -20.20700224038492721, -27.82980252387826781, -10.08426345511578504 ) ) ;
#20819 = ORIENTED_EDGE ( 'NONE', *, *, #13936, .T. ) ;
#20820 = CARTESIAN_POINT ( 'NONE',  ( -28.41354790283022069, 12.60397206714860729, 19.47297445639535596 ) ) ;
#20821 = CARTESIAN_POINT ( 'NONE',  ( -28.13707043255157103, 7.802116958609002673, -21.52861750560941800 ) ) ;
#20822 = VERTEX_POINT ( 'NONE', #13532 ) ;
#20823 = SHAPE_DEFINITION_REPRESENTATION ( #26227, #22271 ) ;
#20824 = AXIS2_PLACEMENT_3D ( 'NONE', #9466, #26998, #18362 ) ;
#20825 = CARTESIAN_POINT ( 'NONE',  ( 109.1587776205901577, -0.004965871434389489830, 0.005390665547499349022 ) ) ;
#20826 = VECTOR ( 'NONE', #1715, 1000.000000000000114 ) ;
#20827 = EDGE_CURVE ( 'NONE', #7710, #16962, #12044, .T. ) ;
#20828 = CARTESIAN_POINT ( 'NONE',  ( 16.75465622695659462, 142.1502242093125687, 4.637075857201994111 ) ) ;
#20829 = CARTESIAN_POINT ( 'NONE',  ( 2.430230287190589422, 31.67257033707502600, 142.0258656395022570 ) ) ;
#20830 = ADVANCED_FACE ( 'NONE', ( #4466 ), #25444, .F. ) ;
#20831 = ORIENTED_EDGE ( 'NONE', *, *, #11896, .T. ) ;
#20832 = CARTESIAN_POINT ( 'NONE',  ( 109.1592201516379674, 0.004867031887019543715, 0.006174480289199423509 ) ) ;
#20834 = CARTESIAN_POINT ( 'NONE',  ( 32.73300124599731475, 117.5726003567930178, 3.836798148479249715 ) ) ;
#20833 = CARTESIAN_POINT ( 'NONE',  ( -1.019300379054419947, 38.21680004809164899, -25.26451264419658571 ) ) ;
#20835 = CARTESIAN_POINT ( 'NONE',  ( 28.37603512858355970, -1.794342805482070258, -114.7183465482400351 ) ) ;
#20836 = ORIENTED_EDGE ( 'NONE', *, *, #23105, .F. ) ;
#20837 = EDGE_CURVE ( 'NONE', #25686, #16400, #3311, .T. ) ;
#20838 = ORIENTED_EDGE ( 'NONE', *, *, #6198, .T. ) ;
#20839 = VERTEX_POINT ( 'NONE', #438 ) ;
#20840 = CARTESIAN_POINT ( 'NONE',  ( 55.79472521941426777, -0.7279028900798781843, 72.75035398477136539 ) ) ;
#20841 = CARTESIAN_POINT ( 'NONE',  ( -1.019300379054419725, -12.21833869579434761, 44.15350047934410327 ) ) ;
#20843 = CARTESIAN_POINT ( 'NONE',  ( 2.063896406836605024, -141.8093313989358251, -31.51663808384702037 ) ) ;
#20842 = CARTESIAN_POINT ( 'NONE',  ( 109.1592201516379674, -0.0003082430541935533277, 0.007856029051018016685 ) ) ;
#20844 = B_SPLINE_CURVE_WITH_KNOTS ( 'NONE', 3,
 ( #22919, #7512, #18580, #16715, #1019, #25070, #27492 ),
 .UNSPECIFIED., .F., .F.,
 ( 4, 3, 4 ),
 ( 5.297613739687102098E-16, 0.02816610861753238160, 0.04000277880656268742 ),
 .UNSPECIFIED. ) ;
#20845 = CARTESIAN_POINT ( 'NONE',  ( 1.833485406944057594, 132.7804117027888253, 58.53321471326925263 ) ) ;
#20846 = LINE ( 'NONE', #14503, #3332 ) ;
#20847 = ORIENTED_EDGE ( 'NONE', *, *, #7209, .T. ) ;
#20848 = CARTESIAN_POINT ( 'NONE',  ( 1.833838848569441682, 107.9566558236576554, 96.96512505224261247 ) ) ;
#20850 = ADVANCED_FACE ( 'NONE', ( #24074 ), #9225, .F. ) ;
#20849 = CARTESIAN_POINT ( 'NONE',  ( -23.77929240705206482, -31.93650644494352875, -17.17389748746951739 ) ) ;
#20851 = ORIENTED_EDGE ( 'NONE', *, *, #13272, .T. ) ;
#20852 = CARTESIAN_POINT ( 'NONE',  ( 2.108985857320947233, -1.281428372374745273, -145.2876352664462445 ) ) ;
#20853 = CARTESIAN_POINT ( 'NONE',  ( 10.93730112725977932, -104.7670965581018123, 108.9902118373738062 ) ) ;
#20854 = CARTESIAN_POINT ( 'NONE',  ( 32.73300124599738581, 39.98094346392455378, -110.6325518752269517 ) ) ;
#20855 = DIRECTION ( 'NONE',  ( 1.000000000000000000, -6.938893903907226837E-18, 1.734723475976806709E-18 ) ) ;
#20856 = CARTESIAN_POINT ( 'NONE',  ( -24.53237795827033807, 22.94498492516385468, 24.99972053297880947 ) ) ;
#20857 = CARTESIAN_POINT ( 'NONE',  ( 2.263178113027039196, -108.9830942735799511, 96.24282436106580008 ) ) ;
#20858 = CARTESIAN_POINT ( 'NONE',  ( 30.59141879584291246, -105.0379937202710892, -49.72305007553554645 ) ) ;
#20859 = ORIENTED_EDGE ( 'NONE', *, *, #19406, .F. ) ;
#20860 = CARTESIAN_POINT ( 'NONE',  ( 25.64681081121879203, -66.70335573067806934, -91.10197563708015878 ) ) ;
#20861 =( BOUNDED_SURFACE ( )  B_SPLINE_SURFACE ( 3, 1, ( 
 ( #782, #16175 ),
 ( #923, #18322 ),
 ( #9563, #9709 ),
 ( #5091, #7566 ) ),
 .UNSPECIFIED., .F., .F., .F. ) 
 B_SPLINE_SURFACE_WITH_KNOTS ( ( 4, 4 ),
 ( 2, 2 ),
 ( 0.000000000000000000, 1.000000000000000000 ),
 ( 0.000000000000000000, 1.000000000000000000 ),
 .UNSPECIFIED. ) 
 GEOMETRIC_REPRESENTATION_ITEM ( )  RATIONAL_B_SPLINE_SURFACE ( (
 ( 1.000000000000000000, 1.000000000000000000),
 ( 0.6386103224230316178, 0.9954351624131538845),
 ( 0.6386103224230316178, 0.9954351624131538845),
 ( 1.000000000000000000, 1.000000000000000000) ) ) 
 REPRESENTATION_ITEM ( '' )  SURFACE ( )  );
#20862 = VECTOR ( 'NONE', #22058, 999.9999999999998863 ) ;
#20863 = CARTESIAN_POINT ( 'NONE',  ( 32.73300124599738581, -44.31599526637883457, -108.9684813982493097 ) ) ;
#20864 = CARTESIAN_POINT ( 'NONE',  ( 1.831572820252009626, 43.90210991190804179, -138.3111855986056753 ) ) ;
#20865 = EDGE_LOOP ( 'NONE', ( #23841, #13206, #17978, #20271 ) ) ;
#20866 = ORIENTED_EDGE ( 'NONE', *, *, #8343, .T. ) ;
#20867 = CARTESIAN_POINT ( 'NONE',  ( 0.000000000000000000, 0.000000000000000000, 0.000000000000000000 ) ) ;
#20868 = FACE_OUTER_BOUND ( 'NONE', #24226, .T. ) ;
#20869 = CARTESIAN_POINT ( 'NONE',  ( 25.64681081121879203, -46.30456157731261868, -102.9795863647033229 ) ) ;
#20870 = ORIENTED_EDGE ( 'NONE', *, *, #25538, .T. ) ;
#20871 = CARTESIAN_POINT ( 'NONE',  ( 26.11404676487259024, -55.62948129436313849, 98.61392875273344316 ) ) ;
#20872 = EDGE_CURVE ( 'NONE', #9793, #28263, #18843, .T. ) ;
#20873 = CARTESIAN_POINT ( 'NONE',  ( 55.49584447822657296, -69.08290406177565046, -22.16497542184476188 ) ) ;
#20874 = CARTESIAN_POINT ( 'NONE',  ( 2.430230287190589422, -133.5180086894987710, -57.85706160874279647 ) ) ;
#20875 = ORIENTED_EDGE ( 'NONE', *, *, #2874, .F. ) ;
#20876 = EDGE_CURVE ( 'NONE', #13127, #22027, #7174, .T. ) ;
#20877 = ORIENTED_EDGE ( 'NONE', *, *, #24868, .F. ) ;
#20878 = CARTESIAN_POINT ( 'NONE',  ( 109.1624594426973118, -0.005372302061316169830, -0.01503296564241275897 ) ) ;
#20879 = CARTESIAN_POINT ( 'NONE',  ( 13.36082413113061307, -117.7941133658645043, 97.52406103376718249 ) ) ;
#20880 = EDGE_CURVE ( 'NONE', #15661, #19144, #3756, .T. ) ;
#20881 = DIRECTION ( 'NONE',  ( 1.000000000000000000, 0.000000000000000000, 0.000000000000000000 ) ) ;
#20882 = B_SPLINE_CURVE_WITH_KNOTS ( 'NONE', 3,
 ( #22, #25956, #26363, #23677, #12699, #10840, #8818 ),
 .UNSPECIFIED., .F., .F.,
 ( 4, 3, 4 ),
 ( 0.000000000000000000, 0.02398743853561324454, 0.04000277880656220864 ),
 .UNSPECIFIED. ) ;
#20883 = CARTESIAN_POINT ( 'NONE',  ( -8.786685647604894456, 7.199674155859698388, 53.04920435127174017 ) ) ;
#20884 = FACE_OUTER_BOUND ( 'NONE', #28388, .T. ) ;
#20885 = VERTEX_POINT ( 'NONE', #20727 ) ;
#20886 = CARTESIAN_POINT ( 'NONE',  ( -1.031422197589711987, 43.06660437151308685, -15.60268798220652720 ) ) ;
#20887 = CARTESIAN_POINT ( 'NONE',  ( 2.063896406836605024, -137.7380992975099332, -46.16709813092763426 ) ) ;
#20888 = CARTESIAN_POINT ( 'NONE',  ( -28.13707043255157103, -6.342158660427161365, -22.00298671236737391 ) ) ;
#20889 = CARTESIAN_POINT ( 'NONE',  ( -20.57838717382308147, -16.28767523336139078, -25.16001208503099917 ) ) ;
#20890 = ORIENTED_EDGE ( 'NONE', *, *, #21155, .T. ) ;
#20891 = CARTESIAN_POINT ( 'NONE',  ( 109.1586900883932856, 0.005833932871491316619, 0.004113747440992344268 ) ) ;
#20892 = CARTESIAN_POINT ( 'NONE',  ( -15.02187109954783750, -6.234056423739195552, 45.93032478317469725 ) ) ;
#20893 = ORIENTED_EDGE ( 'NONE', *, *, #6352, .F. ) ;
#20894 = VERTEX_POINT ( 'NONE', #27196 ) ;
#20895 = ORIENTED_EDGE ( 'NONE', *, *, #5267, .T. ) ;
#20896 = DIRECTION ( 'NONE',  ( 1.000000000000000000, -6.938893903907226837E-18, 1.734723475976806709E-18 ) ) ;
#20897 = CARTESIAN_POINT ( 'NONE',  ( 10.93730112725990011, -119.3442956573265974, -92.80059208661810999 ) ) ;
#20898 = CARTESIAN_POINT ( 'NONE',  ( 109.1624594426973260, -0.009754804742273366636, 0.01263706729758978797 ) ) ;
#20899 = EDGE_CURVE ( 'NONE', #10702, #22524, #5037, .T. ) ;
#20900 = CARTESIAN_POINT ( 'NONE',  ( -28.13707043255157103, -21.52861750560933984, 7.802116958609231823 ) ) ;
#20901 = CARTESIAN_POINT ( 'NONE',  ( 26.28373643307435614, 127.2291519022767403, 9.189598927292342623 ) ) ;
#20902 = ADVANCED_FACE ( 'NONE', ( #22625 ), #28348, .F. ) ;
#20903 = CARTESIAN_POINT ( 'NONE',  ( 5.340103556456460510, 2.303180381360306228, -147.4316330165021043 ) ) ;
#20904 = CARTESIAN_POINT ( 'NONE',  ( 2.433796855181205476, 86.69855925934130880, -116.8607839509047892 ) ) ;
#20905 = EDGE_CURVE ( 'NONE', #28211, #744, #14033, .T. ) ;
#20906 = CARTESIAN_POINT ( 'NONE',  ( -20.20700224038492721, -10.08426345511609235, -27.82980252387815767 ) ) ;
#20907 = FACE_OUTER_BOUND ( 'NONE', #6494, .T. ) ;
#20908 = CARTESIAN_POINT ( 'NONE',  ( -22.23342874802667879, -2.180636882146296696, 31.55488258420093572 ) ) ;
#20909 = CARTESIAN_POINT ( 'NONE',  ( 30.58324630866341920, -21.27395054437324262, 119.0579156359858359 ) ) ;
#20910 = CARTESIAN_POINT ( 'NONE',  ( 2.108985857320929469, 16.46110181986684395, 144.3577886602084845 ) ) ;
#20911 = B_SPLINE_CURVE_WITH_KNOTS ( 'NONE', 3,
 ( #695, #20691, #25042, #20555 ),
 .UNSPECIFIED., .F., .F.,
 ( 4, 4 ),
 ( 5.539203223666104022E-16, 0.008383748772660015725 ),
 .UNSPECIFIED. ) ;
#20912 = CARTESIAN_POINT ( 'NONE',  ( 28.37599760073042177, -114.2774414139535679, 10.20682761621895018 ) ) ;
#20913 = CARTESIAN_POINT ( 'NONE',  ( 32.73300124599732186, 0.000000000000000000, 0.000000000000000000 ) ) ;
#20914 = CARTESIAN_POINT ( 'NONE',  ( -1.058473599757834283, 35.99997772736212198, -28.32531354681296420 ) ) ;
#20915 = ORIENTED_EDGE ( 'NONE', *, *, #3967, .F. ) ;
#20916 = CARTESIAN_POINT ( 'NONE',  ( -20.57838717382308147, -23.26537097894118133, -18.89542499756491978 ) ) ;
#20917 = VERTEX_POINT ( 'NONE', #18578 ) ;
#20918 = DIRECTION ( 'NONE',  ( 1.000000000000000000, -6.938893903907226837E-18, 1.734723475976806709E-18 ) ) ;
#20919 = ORIENTED_EDGE ( 'NONE', *, *, #290, .F. ) ;
#20920 = ORIENTED_EDGE ( 'NONE', *, *, #19181, .F. ) ;
#20921 = ORIENTED_EDGE ( 'NONE', *, *, #8292, .F. ) ;
#20922 = B_SPLINE_CURVE_WITH_KNOTS ( 'NONE', 3,
 ( #6064, #3889, #23771, #4020 ),
 .UNSPECIFIED., .F., .F.,
 ( 4, 4 ),
 ( 3.469446951953614189E-18, 0.008383560773332731156 ),
 .UNSPECIFIED. ) ;
#20923 = ADVANCED_FACE ( 'NONE', ( #11817 ), #10881, .F. ) ;
#20924 = CARTESIAN_POINT ( 'NONE',  ( -25.21435515916025594, 1.749597353048488237E-16, -4.373993382621220594E-17 ) ) ;
#20925 = ADVANCED_FACE ( 'NONE', ( #2892 ), #2806, .F. ) ;
#20926 = ADVANCED_FACE ( 'NONE', ( #5327 ), #13816, .F. ) ;
#20927 = CARTESIAN_POINT ( 'NONE',  ( -23.79223135445719706, 24.83942264280432610, 22.01133905265658441 ) ) ;
#20928 = CARTESIAN_POINT ( 'NONE',  ( 2.430230287190592531, 60.50928654924753403, 132.3371620660953170 ) ) ;
#20929 = CARTESIAN_POINT ( 'NONE',  ( 1.832998868059890096, 125.9352106559993842, -72.09222286250953005 ) ) ;
#20930 = CARTESIAN_POINT ( 'NONE',  ( 1.832998868059858122, -30.69214149073912523, -141.8272129421612249 ) ) ;
#20931 = CARTESIAN_POINT ( 'NONE',  ( 1.832998868059858122, -145.1092030902949830, -0.5339089137763209925 ) ) ;
#20932 = CARTESIAN_POINT ( 'NONE',  ( 5.340103556456468503, -128.8311297043950674, 71.72120378849564304 ) ) ;
#20933 = VERTEX_POINT ( 'NONE', #7223 ) ;
#20934 = ORIENTED_EDGE ( 'NONE', *, *, #17916, .F. ) ;
#20935 = CARTESIAN_POINT ( 'NONE',  ( 25.64700659047694842, -107.3144208978482794, -35.10784848926773805 ) ) ;
#20937 = CARTESIAN_POINT ( 'NONE',  ( -1.619063947482197729, 25.20140673341430571, 38.92136151114879539 ) ) ;
#20936 = CARTESIAN_POINT ( 'NONE',  ( 25.64692872815575342, 66.62748454953282362, -91.15762468787677619 ) ) ;
#20938 = CARTESIAN_POINT ( 'NONE',  ( -20.20700224038492721, -23.35150625415645820, 18.19058640100249491 ) ) ;
#20939 = B_SPLINE_CURVE_WITH_KNOTS ( 'NONE', 3,
 ( #19403, #24026, #1980, #8751, #3730, #10781 ),
 .UNSPECIFIED., .F., .F.,
 ( 4, 2, 4 ),
 ( 1.392007502815792650E-17, 0.0006311571484586009102, 0.001262314296917188159 ),
 .UNSPECIFIED. ) ;
#20940 = CARTESIAN_POINT ( 'NONE',  ( 5.340103579038232517, -111.1041836885941052, -96.93942141937414192 ) ) ;
#20941 = CARTESIAN_POINT ( 'NONE',  ( -20.57838717382308147, 23.26537097894132344, 18.89542499756474569 ) ) ;
#20942 = VERTEX_POINT ( 'NONE', #15978 ) ;
#20943 = CARTESIAN_POINT ( 'NONE',  ( 25.64699802086722968, 91.20712948285751054, -66.55977212001069176 ) ) ;
#20944 = CARTESIAN_POINT ( 'NONE',  ( -1.056502255334265339, 26.51074901220557933, 37.35734037467605617 ) ) ;
#20945 = VERTEX_POINT ( 'NONE', #24785 ) ;
#20946 = CARTESIAN_POINT ( 'NONE',  ( -55.25297051322618813, 0.002853887643042873987, -0.01466904165775150676 ) ) ;
#20947 = DIRECTION ( 'NONE',  ( 1.000000000000000000, -6.938893903907226837E-18, 1.734723475976806709E-18 ) ) ;
#20948 = ORIENTED_EDGE ( 'NONE', *, *, #1883, .F. ) ;
#20949 = EDGE_CURVE ( 'NONE', #12283, #18596, #12304, .T. ) ;
#20950 = B_SPLINE_CURVE_WITH_KNOTS ( 'NONE', 3,
 ( #15579, #11567, #9423, #13579, #9127, #26672 ),
 .UNSPECIFIED., .F., .F.,
 ( 4, 2, 4 ),
 ( 8.673617379884034509E-19, 0.0004335184443140208837, 0.0008670368886280409000 ),
 .UNSPECIFIED. ) ;
#20951 = CARTESIAN_POINT ( 'NONE',  ( 10.93730112725971360, 26.59437931460756488, 148.8212007290661916 ) ) ;
#20952 = ADVANCED_FACE ( 'NONE', ( #12656 ), #2041, .F. ) ;
#20953 = EDGE_CURVE ( 'NONE', #7229, #6633, #23709, .T. ) ;
#20954 = ORIENTED_EDGE ( 'NONE', *, *, #14009, .T. ) ;
#20955 = CARTESIAN_POINT ( 'NONE',  ( -20.47566338032523348, 7.708089572830403746, -28.85746366088566361 ) ) ;
#20956 = CARTESIAN_POINT ( 'NONE',  ( -20.90916690077964191, 34.84883504600978910, 18.74041620980130674 ) ) ;
#20957 = DIRECTION ( 'NONE',  ( -2.641143597229000939E-15, 0.1349691616810136940, -0.9908497996140102071 ) ) ;
#20958 = LINE ( 'NONE', #5423, #5100 ) ;
#20959 = FACE_OUTER_BOUND ( 'NONE', #9531, .T. ) ;
#20960 = LINE ( 'NONE', #21100, #19820 ) ;
#20961 = VERTEX_POINT ( 'NONE', #14818 ) ;
#20962 = CARTESIAN_POINT ( 'NONE',  ( -1.049819825607573254, -13.66706894614408618, 43.71263398674766876 ) ) ;
#20964 = CARTESIAN_POINT ( 'NONE',  ( -55.24390624410018802, 0.001451500391953283731, -0.01032895241566680888 ) ) ;
#20963 = CARTESIAN_POINT ( 'NONE',  ( 30.58324630866348670, -120.6294372749320445, -8.712468656081851393 ) ) ;
#20965 = CARTESIAN_POINT ( 'NONE',  ( -8.786685647604890903, -37.00619870957905277, 38.68584556812340480 ) ) ;
#20966 = VERTEX_POINT ( 'NONE', #21578 ) ;
#20967 = EDGE_LOOP ( 'NONE', ( #15618, #9923, #26139, #8328 ) ) ;
#20968 = VERTEX_POINT ( 'NONE', #10654 ) ;
#20969 = CARTESIAN_POINT ( 'NONE',  ( 55.49584447822657296, 58.53775398922314821, -42.86099773636481558 ) ) ;
#20970 = CARTESIAN_POINT ( 'NONE',  ( -1.239374126674604337, -11.92219841463799135, 44.48112152129359487 ) ) ;
#20972 = CARTESIAN_POINT ( 'NONE',  ( 25.64703792032468854, 11.65444440562330719, -112.3081285890369827 ) ) ;
#20971 = CARTESIAN_POINT ( 'NONE',  ( 13.36082413113063083, -81.89226687791996540, -129.1512766091129834 ) ) ;
#20973 = CARTESIAN_POINT ( 'NONE',  ( 5.340103579038262716, -2.303180387974230303, -147.4316330314913444 ) ) ;
#20974 = CARTESIAN_POINT ( 'NONE',  ( 1.833603222531970056, -132.3826570575579069, -59.42758433816098318 ) ) ;
#20975 = EDGE_LOOP ( 'NONE', ( #1202, #14005, #24254, #15863 ) ) ;
#20976 = CARTESIAN_POINT ( 'NONE',  ( 94.22246935314088034, 70.00000000000002842, -6.938893903907228378E-15 ) ) ;
#20977 = CARTESIAN_POINT ( 'NONE',  ( -16.86833981943428640, -38.94907963570735632, -20.94590537750593739 ) ) ;
#20978 = ORIENTED_EDGE ( 'NONE', *, *, #18452, .T. ) ;
#20979 = CARTESIAN_POINT ( 'NONE',  ( -20.57838717382308147, -29.92853265176832878, -1.611677988432255848 ) ) ;
#20980 = CARTESIAN_POINT ( 'NONE',  ( -20.20612092514784663, 1.137292630518469849, 29.57813644637188233 ) ) ;
#20981 = CARTESIAN_POINT ( 'NONE',  ( -1.619063947482197729, 44.80407745103800465, 11.94059994246113021 ) ) ;
#20982 = CARTESIAN_POINT ( 'NONE',  ( 8.186469777910764023, -57.56191611950399079, 137.8131828745824237 ) ) ;
#20983 = CARTESIAN_POINT ( 'NONE',  ( 2.063896406836605024, -71.46753739785927451, -126.4736179849655144 ) ) ;
#20984 = CARTESIAN_POINT ( 'NONE',  ( 30.59141879584279522, 75.73279557183299460, 88.14706749784066631 ) ) ;
#20985 = ORIENTED_EDGE ( 'NONE', *, *, #12607, .F. ) ;
#20986 = CARTESIAN_POINT ( 'NONE',  ( -55.25297051322618813, -0.001818774723748856851, 0.01483298743815036902 ) ) ;
#20987 = EDGE_CURVE ( 'NONE', #3154, #14763, #19194, .T. ) ;
#20988 = CARTESIAN_POINT ( 'NONE',  ( 26.11404676487257603, 110.9778746459749641, -22.43340081644658213 ) ) ;
#20989 = DIRECTION ( 'NONE',  ( -1.000000000000000000, 6.938893903907226837E-18, -1.734723475976806709E-18 ) ) ;
#20990 = EDGE_CURVE ( 'NONE', #14585, #26642, #7538, .T. ) ;
#20991 = ORIENTED_EDGE ( 'NONE', *, *, #22028, .T. ) ;
#20992 = LINE ( 'NONE', #5057, #8297 ) ;
#20993 = ADVANCED_FACE ( 'NONE', ( #10385 ), #5777, .F. ) ;
#20995 = B_SPLINE_CURVE_WITH_KNOTS ( 'NONE', 3,
 ( #24413, #20362, #22692, #13457 ),
 .UNSPECIFIED., .F., .F.,
 ( 4, 4 ),
 ( 3.206611828262218431E-16, 0.01077107486149763219 ),
 .UNSPECIFIED. ) ;
#20994 = CARTESIAN_POINT ( 'NONE',  ( -1.050230346682665239, -45.79907861045645490, -0.0006945978174090946524 ) ) ;
#20996 = CARTESIAN_POINT ( 'NONE',  ( 6.224689322667647851, -62.55544044765161260, -134.1951906609245384 ) ) ;
#20997 = EDGE_CURVE ( 'NONE', #10838, #5291, #20922, .T. ) ;
#20998 = B_SPLINE_CURVE_WITH_KNOTS ( 'NONE', 3,
 ( #10392, #12944, #21734, #10103 ),
 .UNSPECIFIED., .F., .F.,
 ( 4, 4 ),
 ( 2.593745175800364344E-16, 0.008383748772659713883 ),
 .UNSPECIFIED. ) ;
#20999 = CARTESIAN_POINT ( 'NONE',  ( -21.41430102051751660, -11.22990201072297012, -28.68859753627389253 ) ) ;
#21000 = CARTESIAN_POINT ( 'NONE',  ( 109.1592201516379674, 0.006649399203953390916, 0.004194960840980714069 ) ) ;
#21001 = CARTESIAN_POINT ( 'NONE',  ( 1.833809397773862537, 138.0624841332893880, -44.67209459544923078 ) ) ;
#21002 = ORIENTED_EDGE ( 'NONE', *, *, #23288, .T. ) ;
#21003 = CARTESIAN_POINT ( 'NONE',  ( 32.73300124599735028, 84.80615050150375112, 81.52272205837232377 ) ) ;
#21004 = CARTESIAN_POINT ( 'NONE',  ( 1.833838850093465700, -125.6687428896154159, -72.55487854850817087 ) ) ;
#21005 = DIRECTION ( 'NONE',  ( -0.7637818620346801257, -0.5092696688508642211, 0.3965875333584858997 ) ) ;
#21006 = ORIENTED_EDGE ( 'NONE', *, *, #4618, .F. ) ;
#21007 = ORIENTED_EDGE ( 'NONE', *, *, #10871, .F. ) ;
#21008 = CARTESIAN_POINT ( 'NONE',  ( 109.1624594426973260, -0.01582142368018300480, -0.002129375066970793252 ) ) ;
#21009 = CARTESIAN_POINT ( 'NONE',  ( 9.884929003653608603, -114.6392083957124441, 97.56484214660585508 ) ) ;
#21010 = CARTESIAN_POINT ( 'NONE',  ( 14.74894986621300319, -1.023413983156987147E-16, 2.558534957892467869E-17 ) ) ;
#21011 = CARTESIAN_POINT ( 'NONE',  ( 25.64681081121879203, -83.63051021305848565, -75.86069728269076506 ) ) ;
#21012 = EDGE_CURVE ( 'NONE', #9366, #945, #10262, .T. ) ;
#21013 = CARTESIAN_POINT ( 'NONE',  ( -6.588769196390765970, 38.42957692275894033, 34.04709086065274448 ) ) ;
#21014 =( BOUNDED_SURFACE ( )  B_SPLINE_SURFACE ( 3, 1, ( 
 ( #2075, #10880 ),
 ( #22094, #19639 ),
 ( #2359, #19937 ),
 ( #218, #17482 ) ),
 .UNSPECIFIED., .F., .F., .F. ) 
 B_SPLINE_SURFACE_WITH_KNOTS ( ( 4, 4 ),
 ( 2, 2 ),
 ( 0.000000000000000000, 1.000000000000000000 ),
 ( 0.000000000000000000, 1.000000000000000000 ),
 .UNSPECIFIED. ) 
 GEOMETRIC_REPRESENTATION_ITEM ( )  RATIONAL_B_SPLINE_SURFACE ( (
 ( 1.000000000000000000, 1.000000000000000000),
 ( 0.6386103224230302855, 0.9954351624131538845),
 ( 0.6386103224230302855, 0.9954351624131538845),
 ( 1.000000000000000000, 1.000000000000000000) ) ) 
 REPRESENTATION_ITEM ( '' )  SURFACE ( )  );
#21015 = CARTESIAN_POINT ( 'NONE',  ( -7.711401346138401891, 52.11446537925913702, -6.030154970217080468 ) ) ;
#21016 = CARTESIAN_POINT ( 'NONE',  ( -1.048172774974307053, -45.78636862970790133, 1.020161070261597303 ) ) ;
#21017 = ORIENTED_EDGE ( 'NONE', *, *, #25969, .F. ) ;
#21018 = CARTESIAN_POINT ( 'NONE',  ( 1.833691583653570101, -144.3515375443195978, 14.81406002961268342 ) ) ;
#21019 = DIRECTION ( 'NONE',  ( -1.000000000000000000, -0.000000000000000000, -0.000000000000000000 ) ) ;
#21020 = CARTESIAN_POINT ( 'NONE',  ( 109.1587776205901577, 0.006388631651928893332, -0.003592288931009626502 ) ) ;
#21021 = B_SPLINE_CURVE_WITH_KNOTS ( 'NONE', 3,
 ( #26650, #6964, #5502, #5065, #27376, #22657 ),
 .UNSPECIFIED., .F., .F.,
 ( 4, 2, 4 ),
 ( 4.982613841084487634E-18, 0.0004335151646191490811, 0.0008670303292382946928 ),
 .UNSPECIFIED. ) ;
#21022 = LINE ( 'NONE', #10106, #15776 ) ;
#21023 = EDGE_LOOP ( 'NONE', ( #27449, #11933, #3961, #17327 ) ) ;
#21024 = CARTESIAN_POINT ( 'NONE',  ( -55.25297051322618813, 0.01354497706059944184, 0.006313402748433108967 ) ) ;
#21025 = CARTESIAN_POINT ( 'NONE',  ( -1.323439229708138987, -28.92147054731866263, -35.86372896917463038 ) ) ;
#21026 = VERTEX_POINT ( 'NONE', #14393 ) ;
#21027 = EDGE_CURVE ( 'NONE', #27866, #1025, #24352, .T. ) ;
#21028 = VERTEX_POINT ( 'NONE', #9128 ) ;
#21029 = ORIENTED_EDGE ( 'NONE', *, *, #13220, .F. ) ;
#21030 = ADVANCED_FACE ( 'NONE', ( #13432 ), #16779, .F. ) ;
#21031 = CARTESIAN_POINT ( 'NONE',  ( -1.583189561560253589, 16.68617981233763814, 43.29471907393723029 ) ) ;
#21032 = DIRECTION ( 'NONE',  ( -1.000000000000000000, -0.000000000000000000, -0.000000000000000000 ) ) ;
#21033 = CARTESIAN_POINT ( 'NONE',  ( 109.1589550718175161, 0.005777059646713184060, 0.004900004919101252042 ) ) ;
#21034 = CARTESIAN_POINT ( 'NONE',  ( 2.433796855181233454, -138.8296532063085351, -43.58222566461785163 ) ) ;
#21035 = CARTESIAN_POINT ( 'NONE',  ( -8.786685647604890903, -52.67761315067293282, -9.545808661480407409 ) ) ;
#21036 = CARTESIAN_POINT ( 'NONE',  ( 2.108393763691208456, -132.2055356348357691, -60.26375949664320331 ) ) ;
#21037 = CARTESIAN_POINT ( 'NONE',  ( 109.1592201516379674, 0.007748443302134881173, 0.001331853079201419324 ) ) ;
#21038 = FACE_OUTER_BOUND ( 'NONE', #4187, .T. ) ;
#21039 = CARTESIAN_POINT ( 'NONE',  ( -20.37983603106074781, 24.94323704205437409, -16.25728007463414571 ) ) ;
#21040 = CARTESIAN_POINT ( 'NONE',  ( 26.11404676487257603, -33.91085499298301897, -108.0249973236470993 ) ) ;
#21041 = FACE_OUTER_BOUND ( 'NONE', #13870, .T. ) ;
#21042 = CARTESIAN_POINT ( 'NONE',  ( -55.25297051322618813, 0.006313402748432478395, 0.01354497706059498707 ) ) ;
#21043 = CARTESIAN_POINT ( 'NONE',  ( -1.539763995773681060, -2.469814354917172494, 46.22267697748607418 ) ) ;
#21044 = CARTESIAN_POINT ( 'NONE',  ( -1.031422197589716205, -45.78027046666446154, -1.530725436377304183 ) ) ;
#21045 = CARTESIAN_POINT ( 'NONE',  ( -20.20700224038492721, 29.58392382092673500, 0.9908225410479544193 ) ) ;
#21046 = CARTESIAN_POINT ( 'NONE',  ( 24.01988960052066702, 125.8850824254504630, -36.40943914739766285 ) ) ;
#21047 = ORIENTED_EDGE ( 'NONE', *, *, #3220, .T. ) ;
#21048 = CARTESIAN_POINT ( 'NONE',  ( 109.1592201516379674, 0.002720803050361310545, -0.007376275279030886783 ) ) ;
#21049 = ORIENTED_EDGE ( 'NONE', *, *, #19131, .T. ) ;
#21050 = CARTESIAN_POINT ( 'NONE',  ( -1.048994561756795729, 43.78680886990941445, -13.42228657661138058 ) ) ;
#21051 = CARTESIAN_POINT ( 'NONE',  ( -25.21435515916043357, 6.169479169075458458, -34.05351380035335751 ) ) ;
#21052 = ORIENTED_EDGE ( 'NONE', *, *, #6348, .T. ) ;
#21053 = EDGE_CURVE ( 'NONE', #20645, #16536, #12667, .T. ) ;
#21054 = ORIENTED_EDGE ( 'NONE', *, *, #11402, .F. ) ;
#21055 = ORIENTED_EDGE ( 'NONE', *, *, #19438, .F. ) ;
#21056 = EDGE_CURVE ( 'NONE', #1292, #10573, #14007, .T. ) ;
#21057 = EDGE_CURVE ( 'NONE', #27330, #21644, #4239, .T. ) ;
#21058 = B_SPLINE_CURVE_WITH_KNOTS ( 'NONE', 3,
 ( #10209, #18541, #25468, #3701, #1255, #23170 ),
 .UNSPECIFIED., .F., .F.,
 ( 4, 2, 4 ),
 ( 1.499206600309199041E-16, 0.003570751334075636992, 0.007141502668151123931 ),
 .UNSPECIFIED. ) ;
#21059 = CARTESIAN_POINT ( 'NONE',  ( -1.583189561560256253, 16.68617981233763459, 43.29471907393723029 ) ) ;
#21060 = CARTESIAN_POINT ( 'NONE',  ( 1.832998868059890096, -58.53348008137562175, -132.7810136645743739 ) ) ;
#21061 = CIRCLE ( 'NONE', #13765, 117.6351876552689504 ) ;
#21062 = AXIS2_PLACEMENT_3D ( 'NONE', #11456, #370, #13751 ) ;
#21063 = CARTESIAN_POINT ( 'NONE',  ( -25.21435515916043713, 25.00736669481056751, 23.92354251275909505 ) ) ;
#21064 = CARTESIAN_POINT ( 'NONE',  ( 109.1778270068192853, 0.007736698406808902723, 0.005186985107090163853 ) ) ;
#21065 = CARTESIAN_POINT ( 'NONE',  ( 26.11404676487257603, -107.3263591096432776, 36.06104232266415721 ) ) ;
#21066 = LINE ( 'NONE', #11873, #20308 ) ;
#21067 = EDGE_CURVE ( 'NONE', #9221, #25218, #2290, .T. ) ;
#21068 = DIRECTION ( 'NONE',  ( 0.000000000000000000, 0.000000000000000000, 1.000000000000000000 ) ) ;
#21069 = CARTESIAN_POINT ( 'NONE',  ( 1.833750490713756731, 132.6726660571951300, -58.77746103890142138 ) ) ;
#21070 = VERTEX_POINT ( 'NONE', #2645 ) ;
#21071 = ORIENTED_EDGE ( 'NONE', *, *, #10485, .T. ) ;
#21072 = CARTESIAN_POINT ( 'NONE',  ( 2.263178113027048521, -28.85718369185609333, -142.5035404044876941 ) ) ;
#21074 = CARTESIAN_POINT ( 'NONE',  ( 2.433796855181233454, 57.85512797798071460, -133.5135467655512400 ) ) ;
#21073 = CARTESIAN_POINT ( 'NONE',  ( 1.833485406944057594, -138.1714136985305572, -44.33323125130066700 ) ) ;
#21075 = B_SPLINE_CURVE_WITH_KNOTS ( 'NONE', 3,
 ( #20792, #1082, #25419, #9871, #3382, #10016 ),
 .UNSPECIFIED., .F., .F.,
 ( 4, 2, 4 ),
 ( 0.000000000000000000, 0.0004335184443140258710, 0.0008670368886280517421 ),
 .UNSPECIFIED. ) ;
#21076 = CARTESIAN_POINT ( 'NONE',  ( 1.833750490713655479, -85.50916867388886544, 117.2391074582370578 ) ) ;
#21077 = LINE ( 'NONE', #27983, #22612 ) ;
#21078 = CARTESIAN_POINT ( 'NONE',  ( -55.24728320129491266, 0.009072670231978626973, -0.01137345571547102377 ) ) ;
#21079 = EDGE_CURVE ( 'NONE', #20029, #2039, #6450, .T. ) ;
#21080 = ORIENTED_EDGE ( 'NONE', *, *, #18060, .F. ) ;
#21081 = DIRECTION ( 'NONE',  ( -0.7637818620346800147, -0.6068965246771030886, 0.2198041754873903408 ) ) ;
#21082 = FACE_OUTER_BOUND ( 'NONE', #9344, .T. ) ;
#21083 = CARTESIAN_POINT ( 'NONE',  ( 2.430230287190581429, 46.34481016237006656, -137.9371479820457864 ) ) ;
#21084 = ORIENTED_EDGE ( 'NONE', *, *, #6045, .F. ) ;
#21085 = CARTESIAN_POINT ( 'NONE',  ( -24.53239521893647890, -6.738460611583005466, -33.25736993155761922 ) ) ;
#21086 = EDGE_CURVE ( 'NONE', #26751, #25984, #16767, .T. ) ;
#21087 = CARTESIAN_POINT ( 'NONE',  ( 109.1587776205901861, 0.003736572840496128929, 0.006305329297950517699 ) ) ;
#21088 = EDGE_CURVE ( 'NONE', #21864, #10457, #28392, .T. ) ;
#21089 = ORIENTED_EDGE ( 'NONE', *, *, #17287, .F. ) ;
#21090 = ORIENTED_EDGE ( 'NONE', *, *, #14451, .T. ) ;
#21091 = B_SPLINE_CURVE_WITH_KNOTS ( 'NONE', 3,
 ( #8367, #3896, #21449, #10102, #4311, #17682, #21874 ),
 .UNSPECIFIED., .F., .F.,
 ( 4, 3, 4 ),
 ( 5.463690523629807176E-17, 0.009512539173626407066, 0.02506242213020838661 ),
 .UNSPECIFIED. ) ;
#21092 = CARTESIAN_POINT ( 'NONE',  ( 1.833485406944043827, 96.69979900902167458, 108.1939177044929323 ) ) ;
#21093 = ORIENTED_EDGE ( 'NONE', *, *, #7791, .T. ) ;
#21094 = CARTESIAN_POINT ( 'NONE',  ( -21.41430102051751305, 25.94791611261640085, 16.60879216503605704 ) ) ;
#21095 = CARTESIAN_POINT ( 'NONE',  ( 25.87036335909425588, 112.5399073133628605, 10.83311869338108302 ) ) ;
#21096 = CARTESIAN_POINT ( 'NONE',  ( 109.1586900883932856, -0.004113747440992365084, 0.005833932871491302741 ) ) ;
#21097 = CARTESIAN_POINT ( 'NONE',  ( -55.24390624410018802, 0.01027195578988056128, 0.001811362924362418811 ) ) ;
#21098 = LINE ( 'NONE', #15037, #14762 ) ;
#21099 = CARTESIAN_POINT ( 'NONE',  ( 32.73300124599732186, 0.000000000000000000, 0.000000000000000000 ) ) ;
#21100 = CARTESIAN_POINT ( 'NONE',  ( -28.13707043255157103, 0.7675454997510209321, 22.88591869784690047 ) ) ;
#21101 = ORIENTED_EDGE ( 'NONE', *, *, #14324, .F. ) ;
#21102 = CARTESIAN_POINT ( 'NONE',  ( 26.11404676487257603, -103.8885755249572469, 45.01677474591374306 ) ) ;
#21104 = FACE_OUTER_BOUND ( 'NONE', #11160, .T. ) ;
#21103 = CARTESIAN_POINT ( 'NONE',  ( -20.21097721650788159, -28.26295598655178765, -8.835581399095051580 ) ) ;
#21105 = DIRECTION ( 'NONE',  ( 0.000000000000000000, 1.110223024625156343E-15, 1.000000000000000000 ) ) ;
#21106 = VERTEX_POINT ( 'NONE', #206 ) ;
#21107 = EDGE_LOOP ( 'NONE', ( #13636, #7844, #1458, #19721 ) ) ;
#21108 = VERTEX_POINT ( 'NONE', #18315 ) ;
#21109 = CARTESIAN_POINT ( 'NONE',  ( -4.178947244162641184, -48.81675275154074001, 3.367451375481625320 ) ) ;
#21110 = CARTESIAN_POINT ( 'NONE',  ( 1.834118845439484335, -138.0627591860427117, -44.67218053242533671 ) ) ;
#21112 = CARTESIAN_POINT ( 'NONE',  ( -22.23342874802667168, -7.677086057585177592, -30.68433055777678931 ) ) ;
#21111 = CARTESIAN_POINT ( 'NONE',  ( 109.1778270068192853, 0.005967275455179332777, -0.007152128381195968672 ) ) ;
#21113 = CARTESIAN_POINT ( 'NONE',  ( -1.031422197589711987, -44.01264471863856187, -12.69107518035484361 ) ) ;
#21114 = B_SPLINE_CURVE_WITH_KNOTS ( 'NONE', 3,
 ( #15333, #10613, #24143, #15187, #19525, #28429, #8459, #2093 ),
 .UNSPECIFIED., .F., .F.,
 ( 4, 2, 2, 4 ),
 ( 6.938893903907228378E-18, 0.0002429588503611247914, 0.0004859177007222426439, 0.0009718354014444878898 ),
 .UNSPECIFIED. ) ;
#21115 = DIRECTION ( 'NONE',  ( 0.000000000000000000, 0.000000000000000000, 1.000000000000000000 ) ) ;
#21116 = ORIENTED_EDGE ( 'NONE', *, *, #12447, .F. ) ;
#21117 = CARTESIAN_POINT ( 'NONE',  ( -1.031422197589711987, -43.06660437151296605, 15.60268798220683273 ) ) ;
#21118 = CARTESIAN_POINT ( 'NONE',  ( -1.619063947482197729, -29.22875152547730337, 35.99532424477411041 ) ) ;
#21119 = EDGE_CURVE ( 'NONE', #14178, #25292, #23658, .T. ) ;
#21120 = EDGE_LOOP ( 'NONE', ( #24364, #7402, #26433, #4118 ) ) ;
#21121 = DIRECTION ( 'NONE',  ( 0.000000000000000000, 0.000000000000000000, 1.000000000000000000 ) ) ;
#21122 = CARTESIAN_POINT ( 'NONE',  ( -20.90916690077965612, 5.322316104228523415, 39.20864005633514893 ) ) ;
#21123 = CARTESIAN_POINT ( 'NONE',  ( 6.224689322667647851, 139.9988794244339090, -48.18553814189883866 ) ) ;
#21124 = CARTESIAN_POINT ( 'NONE',  ( 26.11404676487259024, -67.46175819463304890, -90.92995828888270182 ) ) ;
#21125 = EDGE_CURVE ( 'NONE', #2053, #8211, #27771, .T. ) ;
#21126 = CARTESIAN_POINT ( 'NONE',  ( -55.25719721206881729, -0.0006290797159201363779, 0.01115102788683008592 ) ) ;
#21127 = CARTESIAN_POINT ( 'NONE',  ( 26.11404676487257603, 74.91683232330973397, 84.89295829319517850 ) ) ;
#21128 = CARTESIAN_POINT ( 'NONE',  ( 28.43349137099852797, 115.0977416143054199, 46.80919715692925820 ) ) ;
#21130 = ORIENTED_EDGE ( 'NONE', *, *, #8951, .F. ) ;
#21129 = EDGE_CURVE ( 'NONE', #21239, #2577, #7706, .T. ) ;
#21131 = CARTESIAN_POINT ( 'NONE',  ( -12.94347594948481728, -21.16159467081325474, 43.91326021875537577 ) ) ;
#21132 = CARTESIAN_POINT ( 'NONE',  ( 109.1589550718174877, -0.003591809816105041679, -0.006669585340466632761 ) ) ;
#21133 = CARTESIAN_POINT ( 'NONE',  ( -6.574463467970658392, 50.12924290857549181, 11.01561683919999091 ) ) ;
#21134 = ORIENTED_EDGE ( 'NONE', *, *, #20109, .F. ) ;
#21135 = CARTESIAN_POINT ( 'NONE',  ( 2.433796855181219243, 142.0211193075555798, 31.67151202413018396 ) ) ;
#21136 = AXIS2_PLACEMENT_3D ( 'NONE', #25743, #6035, #3860 ) ;
#21137 = VERTEX_POINT ( 'NONE', #9853 ) ;
#21138 = B_SPLINE_CURVE_WITH_KNOTS ( 'NONE', 3,
 ( #9348, #26882, #18237, #16234, #3006, #15946, #18382 ),
 .UNSPECIFIED., .F., .F.,
 ( 4, 3, 4 ),
 ( 0.000000000000000000, 0.02398743853561317516, 0.04000277880656230578 ),
 .UNSPECIFIED. ) ;
#21139 = B_SPLINE_CURVE_WITH_KNOTS ( 'NONE', 3,
 ( #3648, #12424, #27836, #21213, #1764, #10708 ),
 .UNSPECIFIED., .F., .F.,
 ( 4, 2, 4 ),
 ( 8.673617379884035472E-18, 0.0006311636237756842235, 0.001262327247551359773 ),
 .UNSPECIFIED. ) ;
#21140 = B_SPLINE_CURVE_WITH_KNOTS ( 'NONE', 3,
 ( #18327, #9294, #18192, #24568, #4682, #2807, #11301, #27109, #20072, #20208 ),
 .UNSPECIFIED., .F., .F.,
 ( 4, 3, 3, 4 ),
 ( 5.003707553108401214E-17, 0.0002669559177086182258, 0.0005339118354151107648, 0.001067817517169164900 ),
 .UNSPECIFIED. ) ;
#21141 = CARTESIAN_POINT ( 'NONE',  ( -1.050231094221210970, 45.79908322896420003, -0.2545420581350661404 ) ) ;
#21142 = CARTESIAN_POINT ( 'NONE',  ( -8.786685647604890903, -47.14957014837335691, 25.35688121747554291 ) ) ;
#21143 = CARTESIAN_POINT ( 'NONE',  ( -24.53237795827028123, -14.09663893005605395, -30.86653739599992363 ) ) ;
#21144 = CARTESIAN_POINT ( 'NONE',  ( -20.37983603106073005, 18.69865230096527142, -23.16947629293368038 ) ) ;
#21145 = CARTESIAN_POINT ( 'NONE',  ( 1.832998868059890096, 29.64765804470076205, 142.0492247521723641 ) ) ;
#21146 = CARTESIAN_POINT ( 'NONE',  ( 32.73300124599734318, 116.5274707358856006, 16.10546300444864443 ) ) ;
#21147 = B_SPLINE_CURVE_WITH_KNOTS ( 'NONE', 3,
 ( #28455, #19553, #15802, #22141, #15634, #24309, #11201, #19830 ),
 .UNSPECIFIED., .F., .F.,
 ( 4, 2, 2, 4 ),
 ( 0.000000000000000000, 0.002761524886576657151, 0.005523049773153314301, 0.01104609954630661819 ),
 .UNSPECIFIED. ) ;
#21148 = CARTESIAN_POINT ( 'NONE',  ( 1.833485406944043827, -125.4007332306540405, -73.01664920993097496 ) ) ;
#21149 = CARTESIAN_POINT ( 'NONE',  ( 25.64700659047696973, 112.3162501909140900, -11.57609179463844207 ) ) ;
#21150 = CARTESIAN_POINT ( 'NONE',  ( 1.833206308920077632, -15.90849808441977942, 144.2348261777515290 ) ) ;
#21151 = ORIENTED_EDGE ( 'NONE', *, *, #2684, .T. ) ;
#21152 = EDGE_CURVE ( 'NONE', #9239, #11658, #22253, .T. ) ;
#21153 = EDGE_LOOP ( 'NONE', ( #11613, #27043, #19391, #15786, #16118, #6041, #23674, #25114, #8594, #18781, #9322, #12286, #18285, #11085, #19542, #12221, #16829, #13670, #1697, #24003, #23274, #14834, #19601, #12889, #5722, #4776, #23696, #15163, #21806, #687, #16576, #26610, #25574, #14356, #14063, #1977, #1776, #9810, #69, #8622, #19962, #4205, #5713, #23996, #18225, #13430, #7742, #2188, #26667, #19857, #22933, #16897, #4449, #13527, #8794, #1519, #5428, #15429, #10202, #22989, #27858, #7308, #1582, #10737 ) ) ;
#21154 = CARTESIAN_POINT ( 'NONE',  ( -23.77929240705206482, 35.68044874544704470, 6.464423883190010933 ) ) ;
#21155 = EDGE_CURVE ( 'NONE', #414, #21724, #26304, .T. ) ;
#21156 = CARTESIAN_POINT ( 'NONE',  ( -1.019300379054419725, -45.76814864815089123, 2.023851374323154761 ) ) ;
#21157 = CARTESIAN_POINT ( 'NONE',  ( 2.433796855181205476, -43.58222566461547132, -138.8296532063092457 ) ) ;
#21158 = CONICAL_SURFACE ( 'NONE', #8742, 53.53553390275978785, 0.7853981625000051592 ) ;
#21159 = CARTESIAN_POINT ( 'NONE',  ( -1.045287976400351981, 12.68782741917293855, -44.00138577190654132 ) ) ;
#21160 = CARTESIAN_POINT ( 'NONE',  ( 25.81918753295378011, -91.98563552012987543, -65.67738364544824492 ) ) ;
#21161 = DIRECTION ( 'NONE',  ( 0.5914120900931445490, -0.8010740644654237297, -0.09226095020378197176 ) ) ;
#21162 = VERTEX_POINT ( 'NONE', #16610 ) ;
#21163 = DIRECTION ( 'NONE',  ( -5.541455922705464902E-20, 5.223019709708320524E-21, -1.000000000000000000 ) ) ;
#21164 = CARTESIAN_POINT ( 'NONE',  ( 9.884929003653626367, 146.3148513795970871, -35.39789245780186633 ) ) ;
#21165 = CARTESIAN_POINT ( 'NONE',  ( -1.044557008772712514, -25.56990300677008676, -37.98985164565319650 ) ) ;
#21166 = ADVANCED_FACE ( 'NONE', ( #27685 ), #6850, .F. ) ;
#21167 = CARTESIAN_POINT ( 'NONE',  ( -8.786685647604885574, 6.096987947571466530E-17, -1.524246986892866633E-17 ) ) ;
#21168 = CARTESIAN_POINT ( 'NONE',  ( 25.86096068574582674, 65.64181925268327689, 92.04529103340799168 ) ) ;
#21169 = ADVANCED_FACE ( 'NONE', ( #18476 ), #4712, .T. ) ;
#21170 = EDGE_LOOP ( 'NONE', ( #9001, #4223, #24944, #20295 ) ) ;
#21171 = FACE_OUTER_BOUND ( 'NONE', #11226, .T. ) ;
#21172 = CYLINDRICAL_SURFACE ( 'NONE', #14338, 12.50000000000000178 ) ;
#21173 = ORIENTED_EDGE ( 'NONE', *, *, #24530, .F. ) ;
#21174 = ORIENTED_EDGE ( 'NONE', *, *, #21419, .F. ) ;
#21175 = VERTEX_POINT ( 'NONE', #27830 ) ;
#21176 = VECTOR ( 'NONE', #4050, 1000.000000000000114 ) ;
#21177 = AXIS2_PLACEMENT_3D ( 'NONE', #5362, #899, #9683 ) ;
#21178 = CARTESIAN_POINT ( 'NONE',  ( 25.64681081121879203, -110.5293738517606954, -23.06870491922435207 ) ) ;
#21179 = CARTESIAN_POINT ( 'NONE',  ( 109.1586900883932856, 0.001385221016536852898, 0.007002774699553664800 ) ) ;
#21180 = CIRCLE ( 'NONE', #9222, 53.53553390275978785 ) ;
#21181 =( BOUNDED_SURFACE ( )  B_SPLINE_SURFACE ( 3, 1, ( 
 ( #13083, #2125 ),
 ( #6474, #21869 ),
 ( #26319, #12937 ),
 ( #8766, #19694 ) ),
 .UNSPECIFIED., .F., .F., .F. ) 
 B_SPLINE_SURFACE_WITH_KNOTS ( ( 4, 4 ),
 ( 2, 2 ),
 ( 0.000000000000000000, 1.000000000000000000 ),
 ( 0.000000000000000000, 1.000000000000000000 ),
 .UNSPECIFIED. ) 
 GEOMETRIC_REPRESENTATION_ITEM ( )  RATIONAL_B_SPLINE_SURFACE ( (
 ( 1.000000000000000000, 1.000000000000000000),
 ( 0.6386103224230316178, 0.9954351624131538845),
 ( 0.6386103224230316178, 0.9954351624131538845),
 ( 1.000000000000000000, 1.000000000000000000) ) ) 
 REPRESENTATION_ITEM ( '' )  SURFACE ( )  );
#21182 = B_SPLINE_CURVE_WITH_KNOTS ( 'NONE', 3,
 ( #22550, #22109, #20218, #24721, #16050, #11175 ),
 .UNSPECIFIED., .F., .F.,
 ( 4, 2, 4 ),
 ( 0.000000000000000000, 0.003570751334075635258, 0.007141502668151270515 ),
 .UNSPECIFIED. ) ;
#21183 = CARTESIAN_POINT ( 'NONE',  ( 19.66333377628664181, 116.9853418557814280, 72.72773398758276642 ) ) ;
#21184 = VERTEX_POINT ( 'NONE', #27539 ) ;
#21185 = ADVANCED_FACE ( 'NONE', ( #25110 ), #13897, .T. ) ;
#21186 = CARTESIAN_POINT ( 'NONE',  ( 32.73300124599732186, 0.000000000000000000, 0.000000000000000000 ) ) ;
#21187 = CARTESIAN_POINT ( 'NONE',  ( -1.464342487929856995, 46.14921266389555399, -2.431462367721493045 ) ) ;
#21188 = EDGE_CURVE ( 'NONE', #18334, #24971, #10000, .T. ) ;
#21189 = CARTESIAN_POINT ( 'NONE',  ( -1.045287976400362417, -1.530335034934427574, -45.76855895860943235 ) ) ;
#21190 = CARTESIAN_POINT ( 'NONE',  ( 25.64708010899968116, -75.59303792846567660, -83.87281825978691074 ) ) ;
#21191 = CARTESIAN_POINT ( 'NONE',  ( 1.833809397773832783, -141.9016658667394495, -30.34407330672331682 ) ) ;
#21192 = ADVANCED_FACE ( 'NONE', ( #5963 ), #20461, .F. ) ;
#21193 = VECTOR ( 'NONE', #18553, 1000.000000000000227 ) ;
#21194 = B_SPLINE_CURVE_WITH_KNOTS ( 'NONE', 3,
 ( #1242, #12461, #7746, #23001, #23572, #21247, #5723 ),
 .UNSPECIFIED., .F., .F.,
 ( 4, 3, 4 ),
 ( 7.852014599531142026E-16, 0.02816610861753242323, 0.04000277880656292334 ),
 .UNSPECIFIED. ) ;
#21195 = B_SPLINE_CURVE_WITH_KNOTS ( 'NONE', 3,
 ( #23682, #23535, #12569, #5354, #9536, #22355, #3058, #9401, #9251, #11977, #18288, #18154, #26934 ),
 .UNSPECIFIED., .F., .F.,
 ( 4, 3, 3, 3, 4 ),
 ( 1.040834085586084257E-17, 0.0007657099931970558996, 0.001531419946797916336, 0.002296279302920154267, 0.003061450627205756364 ),
 .UNSPECIFIED. ) ;
#21196 = CARTESIAN_POINT ( 'NONE',  ( 55.79472521941428198, -48.13855120843920332, 54.55111121764066695 ) ) ;
#21197 = CARTESIAN_POINT ( 'NONE',  ( 109.1586900883932856, -0.002995460350188440014, -0.006479576224398238618 ) ) ;
#21198 = B_SPLINE_CURVE_WITH_KNOTS ( 'NONE', 3,
 ( #17605, #26388, #6691, #24247, #4504, #21272, #199, #5886, #16827, #6176 ),
 .UNSPECIFIED., .F., .F.,
 ( 4, 2, 2, 2, 4 ),
 ( 2.799429325053882983E-16, 0.0003346187017559026965, 0.0006692374035115254520, 0.001003856105267148099, 0.001338474807022770963 ),
 .UNSPECIFIED. ) ;
#21199 = CARTESIAN_POINT ( 'NONE',  ( 25.64681081121879203, 112.2483031020013442, 12.21581276189844800 ) ) ;
#21200 = CARTESIAN_POINT ( 'NONE',  ( -55.25297051322618813, -0.01354497706059863693, -0.006313402748433391727 ) ) ;
#21201 = FACE_OUTER_BOUND ( 'NONE', #16526, .T. ) ;
#21202 = CARTESIAN_POINT ( 'NONE',  ( 25.64681081121879203, 102.9795863647028682, 46.30456157731362765 ) ) ;
#21203 = ORIENTED_EDGE ( 'NONE', *, *, #10768, .F. ) ;
#21204 = CIRCLE ( 'NONE', #18909, 151.1787379149930359 ) ;
#21205 = ORIENTED_EDGE ( 'NONE', *, *, #27421, .F. ) ;
#21206 = CARTESIAN_POINT ( 'NONE',  ( 109.1592201516379674, -0.007376275279030860763, -0.002720803050361382969 ) ) ;
#21208 = ORIENTED_EDGE ( 'NONE', *, *, #3720, .F. ) ;
#21207 = CARTESIAN_POINT ( 'NONE',  ( 109.1586900883932856, -0.006231977675082132212, 0.003481399864227350312 ) ) ;
#21209 = ORIENTED_EDGE ( 'NONE', *, *, #6283, .T. ) ;
#21210 = VERTEX_POINT ( 'NONE', #5376 ) ;
#21211 = VERTEX_POINT ( 'NONE', #21051 ) ;
#21212 = CIRCLE ( 'NONE', #8806, 117.6351876552689504 ) ;
#21213 = CARTESIAN_POINT ( 'NONE',  ( 1.893872463202031620, -73.39855082356734783, 125.2243573918632507 ) ) ;
#21214 = B_SPLINE_CURVE_WITH_KNOTS ( 'NONE', 3,
 ( #2604, #4624, #11249, #11827, #20021, #20594, #302, #877 ),
 .UNSPECIFIED., .F., .F.,
 ( 4, 2, 2, 4 ),
 ( 0.000000000000000000, 0.0002429588503611201022, 0.0004859177007222402044, 0.0009718354014444856130 ),
 .UNSPECIFIED. ) ;
#21216 = VECTOR ( 'NONE', #8189, 1000.000000000000000 ) ;
#21215 =( BOUNDED_SURFACE ( )  B_SPLINE_SURFACE ( 3, 1, ( 
 ( #5507, #19041 ),
 ( #27818, #1196 ),
 ( #25387, #16887 ),
 ( #20761, #1054 ) ),
 .UNSPECIFIED., .F., .F., .F. ) 
 B_SPLINE_SURFACE_WITH_KNOTS ( ( 4, 4 ),
 ( 2, 2 ),
 ( 0.000000000000000000, 1.000000000000000000 ),
 ( 0.000000000000000000, 1.000000000000000000 ),
 .UNSPECIFIED. ) 
 GEOMETRIC_REPRESENTATION_ITEM ( )  RATIONAL_B_SPLINE_SURFACE ( (
 ( 1.000000000000000000, 1.000000000000000000),
 ( 0.9960225298536222738, 0.9999952330161893110),
 ( 0.9960225298536222738, 0.9999952330161893110),
 ( 1.000000000000000000, 1.000000000000000000) ) ) 
 REPRESENTATION_ITEM ( '' )  SURFACE ( )  );
#21217 = CARTESIAN_POINT ( 'NONE',  ( 55.79472521941426777, 72.42790650415584253, -6.880567342318959945 ) ) ;
#21218 = CARTESIAN_POINT ( 'NONE',  ( 32.73300124599741423, -84.80615050150312584, -81.52272205837286378 ) ) ;
#21219 = CARTESIAN_POINT ( 'NONE',  ( 1.833485406944057594, 72.09189602597886903, -125.9346397303427665 ) ) ;
#21220 = DIRECTION ( 'NONE',  ( 1.000000000000000000, -0.000000000000000000, -0.000000000000000000 ) ) ;
#21221 = EDGE_CURVE ( 'NONE', #3847, #10427, #1342, .T. ) ;
#21222 = CARTESIAN_POINT ( 'NONE',  ( -55.24390624410018802, 0.009209468562451588944, -0.004896917417127890151 ) ) ;
#21223 = CARTESIAN_POINT ( 'NONE',  ( 25.98552792386798771, -112.6247604222998291, -10.75254026142917674 ) ) ;
#21225 = ORIENTED_EDGE ( 'NONE', *, *, #10736, .T. ) ;
#21224 = EDGE_CURVE ( 'NONE', #19554, #2978, #11585, .T. ) ;
#21226 = ORIENTED_EDGE ( 'NONE', *, *, #2151, .F. ) ;
#21227 = CARTESIAN_POINT ( 'NONE',  ( -1.049817751779875907, -27.33161971822171310, 36.75003908324323021 ) ) ;
#21229 = CARTESIAN_POINT ( 'NONE',  ( 109.1721716018069515, 0.006757465437533756447, 0.01567407524361263613 ) ) ;
#21228 = CARTESIAN_POINT ( 'NONE',  ( 1.893872463202068923, 132.9857054814988260, -58.16604752596591510 ) ) ;
#21230 = EDGE_CURVE ( 'NONE', #25910, #17046, #26368, .T. ) ;
#21231 = DIRECTION ( 'NONE',  ( -0.5946245182733608248, 0.5401723099040878218, 0.5955128528260794640 ) ) ;
#21232 = LINE ( 'NONE', #28120, #12924 ) ;
#21233 = CARTESIAN_POINT ( 'NONE',  ( 1.894214914920956172, 96.41356089048431954, -108.5033568857715096 ) ) ;
#21234 = VERTEX_POINT ( 'NONE', #3930 ) ;
#21235 = CARTESIAN_POINT ( 'NONE',  ( -7.733045908741331687, -25.81515396910893045, -45.70676731105710644 ) ) ;
#21236 = CARTESIAN_POINT ( 'NONE',  ( -4.473127245936431073, -49.22197550883370809, -3.196405119333634470 ) ) ;
#21237 = CARTESIAN_POINT ( 'NONE',  ( 26.11404676487257603, 90.92995828888199128, 67.46175819463394419 ) ) ;
#21238 = VERTEX_POINT ( 'NONE', #19735 ) ;
#21239 = VERTEX_POINT ( 'NONE', #28369 ) ;
#21240 = LINE ( 'NONE', #1100, #27299 ) ;
#21241 = ORIENTED_EDGE ( 'NONE', *, *, #14255, .T. ) ;
#21242 = AXIS2_PLACEMENT_3D ( 'NONE', #25800, #8390, #6098 ) ;
#21243 = ORIENTED_EDGE ( 'NONE', *, *, #6290, .T. ) ;
#21244 = CARTESIAN_POINT ( 'NONE',  ( 26.11404676487257603, 76.59696442953305962, -83.38016054979703995 ) ) ;
#21245 = ORIENTED_EDGE ( 'NONE', *, *, #9804, .T. ) ;
#21246 = CARTESIAN_POINT ( 'NONE',  ( -1.619063947482201282, 35.99532424477380488, -29.22875152547769062 ) ) ;
#21247 = CARTESIAN_POINT ( 'NONE',  ( 30.58324630866334104, -57.02364853894557228, 106.6567942264195352 ) ) ;
#21248 = B_SPLINE_CURVE_WITH_KNOTS ( 'NONE', 3,
 ( #1535, #16510, #3274, #25589, #5574, #23429, #3545 ),
 .UNSPECIFIED., .F., .F.,
 ( 4, 3, 4 ),
 ( 0.000000000000000000, 0.02398743853561422640, 0.04000277880656209761 ),
 .UNSPECIFIED. ) ;
#21249 = CARTESIAN_POINT ( 'NONE',  ( -1.259972190295313599, -44.39825172539703146, -12.06706380853675142 ) ) ;
#21250 = CARTESIAN_POINT ( 'NONE',  ( -55.24728320129491266, 0.01137345571547128398, 0.009072670231978179414 ) ) ;
#21251 = CARTESIAN_POINT ( 'NONE',  ( 25.64704443564077252, 83.82001435192627525, 75.65149037849788272 ) ) ;
#21252 = LINE ( 'NONE', #9904, #23052 ) ;
#21253 = CARTESIAN_POINT ( 'NONE',  ( -20.57838717382308147, 18.89542499756533545, 23.26537097894084383 ) ) ;
#21254 = EDGE_CURVE ( 'NONE', #14469, #14145, #17578, .T. ) ;
#21255 = AXIS2_PLACEMENT_3D ( 'NONE', #24992, #1498, #19068 ) ;
#21256 = CARTESIAN_POINT ( 'NONE',  ( -1.045287976400362417, 25.66401692420069125, 37.92705037016716574 ) ) ;
#21258 = CARTESIAN_POINT ( 'NONE',  ( -1.259972190295316485, -45.95417440459613090, 2.243354636026243742 ) ) ;
#21257 = CARTESIAN_POINT ( 'NONE',  ( 25.64708010899964918, -97.81137751680957138, -56.40825696968362735 ) ) ;
#21259 = CARTESIAN_POINT ( 'NONE',  ( 32.73300124599732186, 0.000000000000000000, 0.000000000000000000 ) ) ;
#21260 = VECTOR ( 'NONE', #15982, 1000.000000000000000 ) ;
#21261 = VERTEX_POINT ( 'NONE', #28097 ) ;
#21262 = EDGE_LOOP ( 'NONE', ( #28294, #24255, #2608, #14656 ) ) ;
#21263 = DIRECTION ( 'NONE',  ( 0.5914120900931444380, -0.7023121577978181929, 0.3962188444547167232 ) ) ;
#21264 = CARTESIAN_POINT ( 'NONE',  ( -8.786685647604890903, -37.00619870957905277, 38.68584556812340480 ) ) ;
#21266 = CARTESIAN_POINT ( 'NONE',  ( 2.108985857320904156, 46.11505917359444595, 137.7807691131289403 ) ) ;
#21265 = CARTESIAN_POINT ( 'NONE',  ( 32.73300124599732186, 0.000000000000000000, 0.000000000000000000 ) ) ;
#21267 = CARTESIAN_POINT ( 'NONE',  ( 94.22246935314088034, 70.00000000000004263, 12.49999999999999467 ) ) ;
#21268 = CARTESIAN_POINT ( 'NONE',  ( -1.619063947482201282, 38.92136151114908671, -25.20140673341387227 ) ) ;
#21269 = ORIENTED_EDGE ( 'NONE', *, *, #815, .F. ) ;
#21270 = CARTESIAN_POINT ( 'NONE',  ( -21.41427618760458174, 19.54551635498129514, -23.81423075802588940 ) ) ;
#21271 =( BOUNDED_SURFACE ( )  B_SPLINE_SURFACE ( 3, 1, ( 
 ( #20607, #20175 ),
 ( #22356, #11401 ),
 ( #22499, #18155 ),
 ( #11697, #15999 ) ),
 .UNSPECIFIED., .F., .F., .F. ) 
 B_SPLINE_SURFACE_WITH_KNOTS ( ( 4, 4 ),
 ( 2, 2 ),
 ( 0.000000000000000000, 1.000000000000000000 ),
 ( 0.000000000000000000, 1.000000000000000000 ),
 .UNSPECIFIED. ) 
 GEOMETRIC_REPRESENTATION_ITEM ( )  RATIONAL_B_SPLINE_SURFACE ( (
 ( 1.000000000000000000, 1.000000000000000000),
 ( 0.9934239774497838349, 0.8357310067453913582),
 ( 0.9934239774497838349, 0.8357310067453913582),
 ( 1.000000000000000000, 1.000000000000000000) ) ) 
 REPRESENTATION_ITEM ( '' )  SURFACE ( )  );
#21272 = CARTESIAN_POINT ( 'NONE',  ( -1.259920593601986383, 38.49623866863347388, -25.19630221849063290 ) ) ;
#21273 = VERTEX_POINT ( 'NONE', #17434 ) ;
#21274 = CARTESIAN_POINT ( 'NONE',  ( -20.37983603106074426, -29.73529213200290400, -1.508851015062473211 ) ) ;
#21275 = CARTESIAN_POINT ( 'NONE',  ( -1.031422197589716205, 12.69107518035563764, 44.01264471863834160 ) ) ;
#21276 = CARTESIAN_POINT ( 'NONE',  ( 2.433796855181233454, -57.85512797797981932, 133.5135467655516095 ) ) ;
#21277 = LINE ( 'NONE', #27466, #39 ) ;
#21278 = CARTESIAN_POINT ( 'NONE',  ( -1.583189561560252701, 11.94859433442964658, 44.83405390829658188 ) ) ;
#21279 = ORIENTED_EDGE ( 'NONE', *, *, #9403, .T. ) ;
#21281 = FACE_OUTER_BOUND ( 'NONE', #3118, .T. ) ;
#21280 = B_SPLINE_CURVE_WITH_KNOTS ( 'NONE', 3,
 ( #18100, #13638, #24751, #27009, #7620, #16230, #17945, #7321 ),
 .UNSPECIFIED., .F., .F.,
 ( 4, 2, 2, 4 ),
 ( 1.993045536433795054E-17, 0.0002429588503611324350, 0.0004859177007222449749, 0.0009718354014444726026 ),
 .UNSPECIFIED. ) ;
#21282 = CARTESIAN_POINT ( 'NONE',  ( 109.1592201516379674, 0.006649399203953463774, -0.004194960840990087647 ) ) ;
#21283 = CIRCLE ( 'NONE', #12990, 151.1787379149930359 ) ;
#21284 = ORIENTED_EDGE ( 'NONE', *, *, #16081, .T. ) ;
#21285 = CARTESIAN_POINT ( 'NONE',  ( -1.045287976400386842, 37.92705037016744285, -25.66401692420027203 ) ) ;
#21286 = AXIS2_PLACEMENT_3D ( 'NONE', #20020, #22189, #2456 ) ;
#21287 = DIRECTION ( 'NONE',  ( 0.7563875759206388771, 0.6104009704506959677, 0.2351350468682803785 ) ) ;
#21288 = B_SPLINE_CURVE_WITH_KNOTS ( 'NONE', 3,
 ( #25963, #17034, #19480, #23823 ),
 .UNSPECIFIED., .F., .F.,
 ( 4, 4 ),
 ( 6.258866915731342927E-16, 0.008383748772660081644 ),
 .UNSPECIFIED. ) ;
#21289 = CARTESIAN_POINT ( 'NONE',  ( -1.049819825607587909, -43.71263398674761191, -13.66706894614421408 ) ) ;
#21290 = EDGE_CURVE ( 'NONE', #19216, #19831, #25867, .T. ) ;
#21291 = PRESENTATION_STYLE_ASSIGNMENT (( #23617 ) ) ;
#21292 = EDGE_CURVE ( 'NONE', #20516, #26383, #15268, .T. ) ;
#21293 = CARTESIAN_POINT ( 'NONE',  ( 109.1624594426973260, 0.004489871836309092604, 0.01531968460305925539 ) ) ;
#21294 = CARTESIAN_POINT ( 'NONE',  ( 25.87036335909425944, 74.91347493818375369, -84.67915015758781294 ) ) ;
#21295 = EDGE_CURVE ( 'NONE', #422, #4630, #25411, .T. ) ;
#21296 = CARTESIAN_POINT ( 'NONE',  ( -1.619063947482201282, 35.99532424477380488, -29.22875152547769062 ) ) ;
#21297 = CARTESIAN_POINT ( 'NONE',  ( -1.113548883309551929, -16.03115934825500588, 42.96943836789122173 ) ) ;
#21298 = CARTESIAN_POINT ( 'NONE',  ( -1.464342487929857439, 29.09292098541713401, 35.90631960086386698 ) ) ;
#21299 = ORIENTED_EDGE ( 'NONE', *, *, #15595, .F. ) ;
#21300 = ORIENTED_EDGE ( 'NONE', *, *, #8750, .T. ) ;
#21301 = CARTESIAN_POINT ( 'NONE',  ( 1.834118845439484335, -14.99112450600151369, -144.3336252355298370 ) ) ;
#21302 = CARTESIAN_POINT ( 'NONE',  ( 99.22246935314075245, -90.00000000000005684, 39.99999999999997158 ) ) ;
#21303 = CARTESIAN_POINT ( 'NONE',  ( 109.1586900883932856, -0.005833932871487542728, 0.004113747441000899924 ) ) ;
#21304 = LINE ( 'NONE', #25205, #15614 ) ;
#21305 = CARTESIAN_POINT ( 'NONE',  ( -1.113548883309558368, 42.96943836789127147, 16.03115934825484956 ) ) ;
#21306 = AXIS2_PLACEMENT_3D ( 'NONE', #21564, #19675, #26300 ) ;
#21307 = CARTESIAN_POINT ( 'NONE',  ( -20.20700224038492010, 24.51628800869071867, 16.58740185276683832 ) ) ;
#21308 = ORIENTED_EDGE ( 'NONE', *, *, #8768, .T. ) ;
#21309 = FACE_OUTER_BOUND ( 'NONE', #13338, .T. ) ;
#21310 = CARTESIAN_POINT ( 'NONE',  ( -20.20700224038492721, -18.19058640100206503, 23.35150625415678860 ) ) ;
#21311 = VECTOR ( 'NONE', #27794, 1000.000000000000000 ) ;
#21312 = CARTESIAN_POINT ( 'NONE',  ( 10.93730112725932635, 0.000000000000000000, 0.000000000000000000 ) ) ;
#21313 = CARTESIAN_POINT ( 'NONE',  ( 109.1586059443104944, -0.0002768082440289232316, -0.007068659269321312354 ) ) ;
#21314 = EDGE_LOOP ( 'NONE', ( #9817, #7139, #25960, #280 ) ) ;
#21315 = CARTESIAN_POINT ( 'NONE',  ( -1.619063947482197729, -38.92136151114925724, -25.20140673341360227 ) ) ;
#21316 = CARTESIAN_POINT ( 'NONE',  ( -1.045287976400365970, 1.530335034933814731, -45.76855895860946788 ) ) ;
#21317 = ORIENTED_EDGE ( 'NONE', *, *, #4641, .F. ) ;
#21318 = ORIENTED_EDGE ( 'NONE', *, *, #7537, .T. ) ;
#21319 = VERTEX_POINT ( 'NONE', #4203 ) ;
#21320 = EDGE_CURVE ( 'NONE', #1896, #12511, #23286, .T. ) ;
#21321 = B_SPLINE_CURVE_WITH_KNOTS ( 'NONE', 3,
 ( #6402, #15155, #23978, #13015, #17883, #4813 ),
 .UNSPECIFIED., .F., .F.,
 ( 4, 2, 4 ),
 ( 1.734723475976807094E-18, 0.0006311636237756867171, 0.001262327247551371916 ),
 .UNSPECIFIED. ) ;
#21322 = AXIS2_PLACEMENT_3D ( 'NONE', #18804, #11767, #23152 ) ;
#21323 = FACE_OUTER_BOUND ( 'NONE', #13834, .T. ) ;
#21324 = EDGE_CURVE ( 'NONE', #10869, #10817, #20882, .T. ) ;
#21325 = CARTESIAN_POINT ( 'NONE',  ( 109.1586059443104944, 0.0004635842312889974066, 0.007058870754606111179 ) ) ;
#21326 = EDGE_CURVE ( 'NONE', #19503, #22199, #6665, .T. ) ;
#21327 = CARTESIAN_POINT ( 'NONE',  ( -55.25297051322618813, 0.01466904165775178431, 0.002853887643042449414 ) ) ;
#21328 = B_SPLINE_CURVE_WITH_KNOTS ( 'NONE', 3,
 ( #9158, #22413, #2234, #13182 ),
 .UNSPECIFIED., .F., .F.,
 ( 4, 4 ),
 ( 3.527177457865194202E-16, 0.01077107486149824801 ),
 .UNSPECIFIED. ) ;
#21329 = CARTESIAN_POINT ( 'NONE',  ( 10.93730112725943293, 128.3908183996590537, 79.81734490845931873 ) ) ;
#21330 = ORIENTED_EDGE ( 'NONE', *, *, #22336, .T. ) ;
#21331 = CARTESIAN_POINT ( 'NONE',  ( -55.24271866751342941, -0.009388511352199774979, 0.001425019990778928110 ) ) ;
#21332 = CARTESIAN_POINT ( 'NONE',  ( 1.833206308920118932, -132.2594750499821430, -59.70089323729867914 ) ) ;
#21333 = CARTESIAN_POINT ( 'NONE',  ( 109.1778270068192853, 0.0006237116683871330673, -0.009293669915260188014 ) ) ;
#21334 = CARTESIAN_POINT ( 'NONE',  ( -23.77929240705205416, 15.74261278740719128, 32.66578242509729790 ) ) ;
#21335 = CIRCLE ( 'NONE', #8939, 34.60786435723138510 ) ;
#21336 = CARTESIAN_POINT ( 'NONE',  ( -28.13707043255157103, 22.00298671236740233, -6.342158660427079653 ) ) ;
#21337 = CARTESIAN_POINT ( 'NONE',  ( 109.1778270068192853, 0.008743876326153509834, 0.003210287141656787899 ) ) ;
#21338 = CARTESIAN_POINT ( 'NONE',  ( 26.11404676487259024, 10.71016160607717538, -112.7148551500679332 ) ) ;
#21339 = CARTESIAN_POINT ( 'NONE',  ( 1.834118845439484335, 85.14950727125857100, 117.5010238212701381 ) ) ;
#21340 = CARTESIAN_POINT ( 'NONE',  ( 1.833485406944057594, -117.0814567582550154, 85.72460230293657446 ) ) ;
#21341 = CARTESIAN_POINT ( 'NONE',  ( 55.79472521941428198, -14.41365263906602401, 71.31192372336670360 ) ) ;
#21342 = CARTESIAN_POINT ( 'NONE',  ( -55.25719721206881729, 0.002847566758683125598, -0.01079965405819887508 ) ) ;
#21343 = ORIENTED_EDGE ( 'NONE', *, *, #9635, .F. ) ;
#21344 = VERTEX_POINT ( 'NONE', #21487 ) ;
#21345 = DIRECTION ( 'NONE',  ( -0.7637818620346801257, 0.1788995134688785849, -0.6201872550346672064 ) ) ;
#21346 =( BOUNDED_SURFACE ( )  B_SPLINE_SURFACE ( 3, 1, ( 
 ( #25966, #23825 ),
 ( #10569, #10437 ),
 ( #19336, #6257 ),
 ( #28112, #17446 ) ),
 .UNSPECIFIED., .F., .F., .F. ) 
 B_SPLINE_SURFACE_WITH_KNOTS ( ( 4, 4 ),
 ( 2, 2 ),
 ( 0.000000000000000000, 1.000000000000000000 ),
 ( 0.000000000000000000, 1.000000000000000000 ),
 .UNSPECIFIED. ) 
 GEOMETRIC_REPRESENTATION_ITEM ( )  RATIONAL_B_SPLINE_SURFACE ( (
 ( 1.000000000000000000, 1.000000000000000000),
 ( 0.9934239774497837239, 0.8357310067453919133),
 ( 0.9934239774497837239, 0.8357310067453919133),
 ( 1.000000000000000000, 1.000000000000000000) ) ) 
 REPRESENTATION_ITEM ( '' )  SURFACE ( )  );
#21348 = ORIENTED_EDGE ( 'NONE', *, *, #15279, .F. ) ;
#21347 = CARTESIAN_POINT ( 'NONE',  ( -24.53239521893646824, -30.86654523348673962, -14.09666242510777145 ) ) ;
#21349 = ORIENTED_EDGE ( 'NONE', *, *, #26251, .T. ) ;
#21350 = ORIENTED_EDGE ( 'NONE', *, *, #26065, .T. ) ;
#21351 = ORIENTED_EDGE ( 'NONE', *, *, #9859, .T. ) ;
#21352 = EDGE_CURVE ( 'NONE', #15570, #10003, #3687, .T. ) ;
#21353 = ADVANCED_FACE ( 'NONE', ( #19889 ), #11979, .F. ) ;
#21354 =( BOUNDED_SURFACE ( )  B_SPLINE_SURFACE ( 3, 1, ( 
 ( #19290, #8368 ),
 ( #23913, #17128 ),
 ( #10804, #17958 ),
 ( #5012, #9355 ) ),
 .UNSPECIFIED., .F., .F., .F. ) 
 B_SPLINE_SURFACE_WITH_KNOTS ( ( 4, 4 ),
 ( 2, 2 ),
 ( 0.000000000000000000, 1.000000000000000000 ),
 ( 0.000000000000000000, 1.000000000000000000 ),
 .UNSPECIFIED. ) 
 GEOMETRIC_REPRESENTATION_ITEM ( )  RATIONAL_B_SPLINE_SURFACE ( (
 ( 1.000000000000000000, 1.000000000000000000),
 ( 0.9956975270656955868, 0.8568959468854907557),
 ( 0.9956975270656955868, 0.8568959468854907557),
 ( 1.000000000000000000, 1.000000000000000000) ) ) 
 REPRESENTATION_ITEM ( '' )  SURFACE ( )  );
#21355 = CARTESIAN_POINT ( 'NONE',  ( 28.37644542392839853, 80.14194118792715926, 95.06674036596241706 ) ) ;
#21356 = ADVANCED_FACE ( 'NONE', ( #176 ), #14902, .F. ) ;
#21357 = CARTESIAN_POINT ( 'NONE',  ( -25.21435515916043713, -23.92354251275954979, -25.00736669481013053 ) ) ;
#21358 = LINE ( 'NONE', #9254, #14262 ) ;
#21359 = EDGE_CURVE ( 'NONE', #25814, #431, #9200, .T. ) ;
#21360 = CARTESIAN_POINT ( 'NONE',  ( 32.73300124599769134, -51.32617430724849328, -105.8473486001054198 ) ) ;
#21361 = CARTESIAN_POINT ( 'NONE',  ( 109.1592201516379674, -0.007845213074660005795, -0.0005146241775907089413 ) ) ;
#21362 = CARTESIAN_POINT ( 'NONE',  ( -28.41354790283022069, -5.969609727607868344, 22.41474081378006744 ) ) ;
#21363 = CARTESIAN_POINT ( 'NONE',  ( 26.11404676487257603, 65.63269960453241936, 92.25884714080432047 ) ) ;
#21364 = LINE ( 'NONE', #1354, #24433 ) ;
#21365 = VERTEX_POINT ( 'NONE', #22196 ) ;
#21366 = EDGE_LOOP ( 'NONE', ( #23014, #10720, #13026, #6028 ) ) ;
#21368 = CARTESIAN_POINT ( 'NONE',  ( -55.24271866751342941, 0.006757859501010503658, -0.006671293903668132526 ) ) ;
#21367 = CARTESIAN_POINT ( 'NONE',  ( 119.2224693531408803, 70.00000000000004263, 39.99999999999999289 ) ) ;
#21369 = CARTESIAN_POINT ( 'NONE',  ( -8.786685647604896232, 9.545808661481343549, 52.67761315067276229 ) ) ;
#21370 = CARTESIAN_POINT ( 'NONE',  ( 26.11404676487259024, 10.71016160607717538, -112.7148551500679332 ) ) ;
#21371 = DIRECTION ( 'NONE',  ( 0.000000000000000000, 5.223019709707975211E-21, -1.000000000000000000 ) ) ;
#21372 = ORIENTED_EDGE ( 'NONE', *, *, #1633, .F. ) ;
#21373 = CARTESIAN_POINT ( 'NONE',  ( -55.25297051322618813, -0.01483298743815008106, -0.001818774723749387676 ) ) ;
#21374 = B_SPLINE_CURVE_WITH_KNOTS ( 'NONE', 3,
 ( #10824, #19584, #16881, #25668, #5948, #19170, #14699 ),
 .UNSPECIFIED., .F., .F.,
 ( 4, 3, 4 ),
 ( 1.734723475976807094E-18, 0.009512539173626401862, 0.02506242213020843518 ),
 .UNSPECIFIED. ) ;
#21375 = DIRECTION ( 'NONE',  ( 0.7637818620346800147, -0.3617919495470791613, -0.5345501402766260624 ) ) ;
#21376 = CARTESIAN_POINT ( 'NONE',  ( 2.433796855181233454, -84.34988187691011774, 118.5671979538053904 ) ) ;
#21377 = ORIENTED_EDGE ( 'NONE', *, *, #17565, .T. ) ;
#21378 = EDGE_LOOP ( 'NONE', ( #23876, #11031, #13154, #20428 ) ) ;
#21379 = CARTESIAN_POINT ( 'NONE',  ( -1.539760825549686407, -38.84664866728793697, -25.17088484262129455 ) ) ;
#21380 = ORIENTED_EDGE ( 'NONE', *, *, #11295, .F. ) ;
#21381 = ORIENTED_EDGE ( 'NONE', *, *, #16075, .F. ) ;
#21382 = EDGE_CURVE ( 'NONE', #17891, #3139, #11956, .T. ) ;
#21383 = CARTESIAN_POINT ( 'NONE',  ( 13.36082413113063083, -22.28175172543457450, -151.2941478187909752 ) ) ;
#21384 =( BOUNDED_SURFACE ( )  B_SPLINE_SURFACE ( 3, 1, ( 
 ( #18234, #22737 ),
 ( #26455, #17946 ),
 ( #6758, #20256 ),
 ( #11206, #7047 ) ),
 .UNSPECIFIED., .F., .F., .F. ) 
 B_SPLINE_SURFACE_WITH_KNOTS ( ( 4, 4 ),
 ( 2, 2 ),
 ( 0.000000000000000000, 1.000000000000000000 ),
 ( 0.000000000000000000, 1.000000000000000000 ),
 .UNSPECIFIED. ) 
 GEOMETRIC_REPRESENTATION_ITEM ( )  RATIONAL_B_SPLINE_SURFACE ( (
 ( 1.000000000000000000, 1.000000000000000000),
 ( 0.7789835883360578528, 0.9689951854195403280),
 ( 0.7789835883360578528, 0.9689951854195403280),
 ( 1.000000000000000000, 1.000000000000000000) ) ) 
 REPRESENTATION_ITEM ( '' )  SURFACE ( )  );
#21385 = VERTEX_POINT ( 'NONE', #4482 ) ;
#21386 = ADVANCED_FACE ( 'NONE', ( #4780 ), #26669, .F. ) ;
#21387 = CARTESIAN_POINT ( 'NONE',  ( 26.11404676487257603, -45.01677474591340911, -103.8885755249573606 ) ) ;
#21388 = CARTESIAN_POINT ( 'NONE',  ( 2.433796855181205476, -118.5671979538062146, 84.34988187690890982 ) ) ;
#21389 = CARTESIAN_POINT ( 'NONE',  ( 5.340103579038186332, -126.5279493327089995, 75.71042924123000262 ) ) ;
#21390 = CARTESIAN_POINT ( 'NONE',  ( 6.224689322667630975, -71.79702446228212409, -129.4863684118294884 ) ) ;
#21391 = CARTESIAN_POINT ( 'NONE',  ( 1.833485406944057594, -15.69895494453287021, -144.2578170162064737 ) ) ;
#21392 = CARTESIAN_POINT ( 'NONE',  ( 2.430230287190589422, -116.8646894862417867, 86.70145658344620188 ) ) ;
#21393 = CARTESIAN_POINT ( 'NONE',  ( 26.11404676487257603, -103.8885755249572469, 45.01677474591374306 ) ) ;
#21394 = CARTESIAN_POINT ( 'NONE',  ( 25.81918753295376945, 103.6306245682015117, 45.11728622333180283 ) ) ;
#21396 = CARTESIAN_POINT ( 'NONE',  ( 26.11404676487257603, -10.71016160607644174, 112.7148551500680185 ) ) ;
#21395 = CARTESIAN_POINT ( 'NONE',  ( 25.64681081121879203, -97.57530875170564855, -56.81519825470856944 ) ) ;
#21397 = CARTESIAN_POINT ( 'NONE',  ( -1.463510566862830986, 29.09194585123833932, -35.90603835816513367 ) ) ;
#21398 = B_SPLINE_CURVE_WITH_KNOTS ( 'NONE', 3,
 ( #25926, #6217, #4033, #28205, #8505, #16725 ),
 .UNSPECIFIED., .F., .F.,
 ( 4, 2, 4 ),
 ( 1.734723475976807094E-18, 0.0004335184443140234316, 0.0008670368886280451284 ),
 .UNSPECIFIED. ) ;
#21399 = ORIENTED_EDGE ( 'NONE', *, *, #1937, .T. ) ;
#21400 = ORIENTED_EDGE ( 'NONE', *, *, #8531, .F. ) ;
#21401 = CARTESIAN_POINT ( 'NONE',  ( -1.031422197589711987, 44.01264471863864713, 12.69107518035455762 ) ) ;
#21402 = CARTESIAN_POINT ( 'NONE',  ( 1.833809397773847882, -72.70895493223461870, 125.5796696653635678 ) ) ;
#21404 = CARTESIAN_POINT ( 'NONE',  ( 25.73574536432414916, -98.23578516674997729, 55.78561308781451089 ) ) ;
#21403 = CARTESIAN_POINT ( 'NONE',  ( 2.430230287190572103, -28.83279105684323440, -142.6294793592101087 ) ) ;
#21405 = CARTESIAN_POINT ( 'NONE',  ( 26.11404676487257603, -76.59696442953135431, -83.38016054979861735 ) ) ;
#21406 = CARTESIAN_POINT ( 'NONE',  ( -18.41936578851711559, 29.33493038358074045, -30.66520733838660462 ) ) ;
#21407 = ORIENTED_EDGE ( 'NONE', *, *, #6406, .T. ) ;
#21408 = CARTESIAN_POINT ( 'NONE',  ( -23.79248802219729697, -22.01156985585185311, -24.83956736572401525 ) ) ;
#21409 = CARTESIAN_POINT ( 'NONE',  ( -1.539763995773690164, -44.72359274866473555, 11.93465967526341842 ) ) ;
#21410 = ORIENTED_EDGE ( 'NONE', *, *, #10237, .T. ) ;
#21411 = CARTESIAN_POINT ( 'NONE',  ( 28.37644542392842695, -21.87158679436108955, -122.4011828058667106 ) ) ;
#21412 = CARTESIAN_POINT ( 'NONE',  ( 32.73300124599732186, 0.000000000000000000, 0.000000000000000000 ) ) ;
#21413 = CARTESIAN_POINT ( 'NONE',  ( 25.64704443564078318, 107.3436266109713273, 35.01840413910168337 ) ) ;
#21414 = CARTESIAN_POINT ( 'NONE',  ( -8.786685647604887350, -25.35688121747534751, -47.14957014837345639 ) ) ;
#21415 = CARTESIAN_POINT ( 'NONE',  ( -1.045287976400365970, -45.76855895860942525, 1.530335034934587002 ) ) ;
#21416 = VERTEX_POINT ( 'NONE', #17386 ) ;
#21417 = CARTESIAN_POINT ( 'NONE',  ( -15.02187109954783040, -20.12219089991063825, 41.75590530176331328 ) ) ;
#21418 = LINE ( 'NONE', #12635, #27244 ) ;
#21419 = EDGE_CURVE ( 'NONE', #11307, #16438, #15217, .T. ) ;
#21420 = VERTEX_POINT ( 'NONE', #118 ) ;
#21421 = CARTESIAN_POINT ( 'NONE',  ( 1.833485406944057594, -29.64752363041639782, 142.0485807715645024 ) ) ;
#21422 = ORIENTED_EDGE ( 'NONE', *, *, #9767, .F. ) ;
#21423 = ADVANCED_FACE ( 'NONE', ( #6465 ), #4067, .F. ) ;
#21424 = CARTESIAN_POINT ( 'NONE',  ( -8.786685647604896232, -7.199674155858612146, 53.04920435127190359 ) ) ;
#21425 = EDGE_CURVE ( 'NONE', #9239, #9063, #19829, .T. ) ;
#21426 = CARTESIAN_POINT ( 'NONE',  ( -21.41427618760457818, -19.54551635498111395, 23.81423075802604217 ) ) ;
#21427 = CARTESIAN_POINT ( 'NONE',  ( -1.050230346682684113, 37.05182464822020449, 26.92058491724826297 ) ) ;
#21428 = CARTESIAN_POINT ( 'NONE',  ( -28.41354790283022069, 19.47297445639550162, -12.60397206714839413 ) ) ;
#21429 = CARTESIAN_POINT ( 'NONE',  ( 28.37603512858461485, 108.5491486026796224, -37.15644006762103402 ) ) ;
#21430 = CARTESIAN_POINT ( 'NONE',  ( 10.93730112726003156, 71.28103789255123957, -133.3192575531793693 ) ) ;
#21431 = CARTESIAN_POINT ( 'NONE',  ( 2.063896406836605024, 145.2631347824382715, 1.344106060020868076 ) ) ;
#21432 = CARTESIAN_POINT ( 'NONE',  ( -1.463510566862824991, -29.09194585123808707, 35.90603835816536815 ) ) ;
#21433 =( BOUNDED_SURFACE ( )  B_SPLINE_SURFACE ( 3, 1, ( 
 ( #1152, #25759 ),
 ( #10375, #22904 ),
 ( #7648, #20996 ),
 ( #25627, #27478 ) ),
 .UNSPECIFIED., .F., .F., .F. ) 
 B_SPLINE_SURFACE_WITH_KNOTS ( ( 4, 4 ),
 ( 2, 2 ),
 ( 0.000000000000000000, 1.000000000000000000 ),
 ( 0.000000000000000000, 1.000000000000000000 ),
 .UNSPECIFIED. ) 
 GEOMETRIC_REPRESENTATION_ITEM ( )  RATIONAL_B_SPLINE_SURFACE ( (
 ( 1.000000000000000000, 1.000000000000000000),
 ( 0.6386103224230316178, 0.9954351624131538845),
 ( 0.6386103224230316178, 0.9954351624131538845),
 ( 1.000000000000000000, 1.000000000000000000) ) ) 
 REPRESENTATION_ITEM ( '' )  SURFACE ( )  );
#21434 = CARTESIAN_POINT ( 'NONE',  ( -20.20700224038492721, -24.51628800869059432, -16.58740185276701951 ) ) ;
#21435 = LINE ( 'NONE', #24037, #1492 ) ;
#21436 = CARTESIAN_POINT ( 'NONE',  ( 25.64681081121879203, 35.28660243342691416, -107.2555980796237804 ) ) ;
#21437 = EDGE_LOOP ( 'NONE', ( #26277, #2276, #22014, #17357 ) ) ;
#21438 = VERTEX_POINT ( 'NONE', #6610 ) ;
#21439 = VERTEX_POINT ( 'NONE', #28322 ) ;
#21440 = CARTESIAN_POINT ( 'NONE',  ( -1.539760825549689516, -43.19716078875427456, 16.63252404870400269 ) ) ;
#21441 = CARTESIAN_POINT ( 'NONE',  ( -20.20612091757423912, 1.137293889216362874, -29.57813639663777039 ) ) ;
#21442 = DIRECTION ( 'NONE',  ( -0.7071067818211357325, 9.150583771627653840E-17, -0.7071067805519594129 ) ) ;
#21443 = CARTESIAN_POINT ( 'NONE',  ( 25.64708010899964208, -83.94602815988619682, -75.51173009720608320 ) ) ;
#21444 = CARTESIAN_POINT ( 'NONE',  ( -1.323439229708146536, 43.04565903621286083, -16.42345129173351381 ) ) ;
#21445 = EDGE_CURVE ( 'NONE', #6599, #6748, #23587, .T. ) ;
#21446 = CARTESIAN_POINT ( 'NONE',  ( 109.1586900883932856, 0.007137750914552287197, 0.0001010081143884401729 ) ) ;
#21447 = CARTESIAN_POINT ( 'NONE',  ( 1.893872463202038947, 97.83022426232111002, -107.2274879309817806 ) ) ;
#21448 = ORIENTED_EDGE ( 'NONE', *, *, #5742, .T. ) ;
#21449 = CARTESIAN_POINT ( 'NONE',  ( -12.94347594948484392, -8.691477019903656398, -47.96504705787742040 ) ) ;
#21450 = CARTESIAN_POINT ( 'NONE',  ( -20.37983603106074426, -18.69865230096510444, 23.16947629293382960 ) ) ;
#21451 = CARTESIAN_POINT ( 'NONE',  ( -1.050230346682690108, -37.05182464822001975, -26.92058491724852942 ) ) ;
#21452 = B_SPLINE_CURVE_WITH_KNOTS ( 'NONE', 3,
 ( #21034, #11839, #5499, #20752 ),
 .UNSPECIFIED., .F., .F.,
 ( 4, 4 ),
 ( 3.364033176744297164E-16, 0.01077107486149825669 ),
 .UNSPECIFIED. ) ;
#21453 = CARTESIAN_POINT ( 'NONE',  ( 25.81918753295379076, 0.9336804662327143900, 113.0221398901142607 ) ) ;
#21454 = CARTESIAN_POINT ( 'NONE',  ( 25.70243777736190438, 65.79472741891264320, 91.80600962488421146 ) ) ;
#21455 = ADVANCED_FACE ( 'NONE', ( #17527 ), #10648, .F. ) ;
#21456 = ORIENTED_EDGE ( 'NONE', *, *, #14319, .F. ) ;
#21457 = CARTESIAN_POINT ( 'NONE',  ( 25.64708010899960300, -45.87517365398556279, 103.1718249732473538 ) ) ;
#21458 = DIRECTION ( 'NONE',  ( -1.000000000000000000, -0.000000000000000000, -0.000000000000000000 ) ) ;
#21459 = ORIENTED_EDGE ( 'NONE', *, *, #15419, .T. ) ;
#21460 = EDGE_CURVE ( 'NONE', #17730, #21851, #21435, .T. ) ;
#21461 = EDGE_CURVE ( 'NONE', #13553, #26751, #24170, .T. ) ;
#21462 = ORIENTED_EDGE ( 'NONE', *, *, #2654, .T. ) ;
#21463 = VERTEX_POINT ( 'NONE', #2118 ) ;
#21464 = CARTESIAN_POINT ( 'NONE',  ( -20.20612092514784663, 10.22177639105900226, 27.77903665678154255 ) ) ;
#21465 = CARTESIAN_POINT ( 'NONE',  ( 1.833809397773857430, 30.34407330672380709, -141.9016658667393074 ) ) ;
#21466 = EDGE_CURVE ( 'NONE', #19804, #24626, #26023, .T. ) ;
#21467 =( BOUNDED_SURFACE ( )  B_SPLINE_SURFACE ( 3, 1, ( 
 ( #5076, #5366 ),
 ( #18304, #7694 ),
 ( #27084, #16453 ),
 ( #7393, #27530 ) ),
 .UNSPECIFIED., .F., .F., .F. ) 
 B_SPLINE_SURFACE_WITH_KNOTS ( ( 4, 4 ),
 ( 2, 2 ),
 ( 0.000000000000000000, 1.000000000000000000 ),
 ( 0.000000000000000000, 1.000000000000000000 ),
 .UNSPECIFIED. ) 
 GEOMETRIC_REPRESENTATION_ITEM ( )  RATIONAL_B_SPLINE_SURFACE ( (
 ( 1.000000000000000000, 1.000000000000000000),
 ( 0.6386103224230316178, 0.9954351624131538845),
 ( 0.6386103224230316178, 0.9954351624131538845),
 ( 1.000000000000000000, 1.000000000000000000) ) ) 
 REPRESENTATION_ITEM ( '' )  SURFACE ( )  );
#21468 = CARTESIAN_POINT ( 'NONE',  ( -1.019300379054419947, 12.21833869579527310, 44.15350047934384747 ) ) ;
#21469 = ORIENTED_EDGE ( 'NONE', *, *, #26542, .F. ) ;
#21470 = CARTESIAN_POINT ( 'NONE',  ( -1.239374126674604337, 35.79060836339814955, -28.97829083655452820 ) ) ;
#21471 = ORIENTED_EDGE ( 'NONE', *, *, #28075, .F. ) ;
#21472 = CARTESIAN_POINT ( 'NONE',  ( 1.833485406944043827, -132.3460930279887293, -59.50871042846357994 ) ) ;
#21473 = CARTESIAN_POINT ( 'NONE',  ( 1.834118845439484335, 132.4921483272728153, 59.18411796427096050 ) ) ;
#21474 = DIRECTION ( 'NONE',  ( -0.5914120900931443270, 0.1754905759872845417, 0.7870418015781053267 ) ) ;
#21475 = CARTESIAN_POINT ( 'NONE',  ( -8.786685647604896232, 23.24040270374459993, 48.22796981442743913 ) ) ;
#21476 = CARTESIAN_POINT ( 'NONE',  ( -1.031422197589711764, 28.14735071801743871, -36.13727897780136544 ) ) ;
#21477 = CARTESIAN_POINT ( 'NONE',  ( 13.36082413113061307, 135.4964217943317237, -70.90215303571982020 ) ) ;
#21478 = CARTESIAN_POINT ( 'NONE',  ( 30.58324630866347960, 100.1119227962719265, 67.85993782330791646 ) ) ;
#21479 = B_SPLINE_CURVE_WITH_KNOTS ( 'NONE', 3,
 ( #17714, #8958, #22486, #2302 ),
 .UNSPECIFIED., .F., .F.,
 ( 4, 4 ),
 ( 1.847623020647441449E-16, 0.001982023823822945483 ),
 .UNSPECIFIED. ) ;
#21480 = CARTESIAN_POINT ( 'NONE',  ( -20.57838717382308502, 27.96569011373086866, -10.78122205917010135 ) ) ;
#21481 = CARTESIAN_POINT ( 'NONE',  ( 2.433796855181205476, 71.49415740225076377, 126.7346379669258312 ) ) ;
#21482 = EDGE_CURVE ( 'NONE', #9399, #19503, #19275, .T. ) ;
#21483 = ORIENTED_EDGE ( 'NONE', *, *, #6401, .F. ) ;
#21484 = EDGE_CURVE ( 'NONE', #7441, #8520, #21993, .T. ) ;
#21485 = ORIENTED_EDGE ( 'NONE', *, *, #18091, .F. ) ;
#21486 = CARTESIAN_POINT ( 'NONE',  ( 2.263178607246684404, -108.9830946142707262, -96.24282447295553311 ) ) ;
#21488 = ORIENTED_EDGE ( 'NONE', *, *, #15521, .T. ) ;
#21487 = CARTESIAN_POINT ( 'NONE',  ( -1.619063947482197729, -35.99532424477401094, -29.22875152547743838 ) ) ;
#21489 = VERTEX_POINT ( 'NONE', #2257 ) ;
#21490 = ORIENTED_EDGE ( 'NONE', *, *, #8113, .F. ) ;
#21491 = ORIENTED_EDGE ( 'NONE', *, *, #24948, .F. ) ;
#21492 = CARTESIAN_POINT ( 'NONE',  ( 32.73300124599734318, 115.8010721414084117, 20.69176323058669809 ) ) ;
#21493 = B_SPLINE_CURVE_WITH_KNOTS ( 'NONE', 3,
 ( #17708, #2157, #12968, #12822, #296, #6653 ),
 .UNSPECIFIED., .F., .F.,
 ( 4, 2, 4 ),
 ( 1.852685484479510670E-17, 0.0006311636237756912708, 0.001262327247551363676 ),
 .UNSPECIFIED. ) ;
#21494 = DIRECTION ( 'NONE',  ( 0.000000000000000000, 5.223019709707975211E-21, -1.000000000000000000 ) ) ;
#21495 = CARTESIAN_POINT ( 'NONE',  ( -1.045287976400365970, 44.00138577190666922, 12.68782741917247670 ) ) ;
#21496 = CARTESIAN_POINT ( 'NONE',  ( 10.93730112725932813, 151.0983828010088246, -4.928439153520510985 ) ) ;
#21497 = CARTESIAN_POINT ( 'NONE',  ( -16.86833981943423311, 31.95666732167563850, -30.57013526701928186 ) ) ;
#21498 = CARTESIAN_POINT ( 'NONE',  ( 109.1778270068192853, 0.004106684808170127376, 0.008360410075196028634 ) ) ;
#21499 = CARTESIAN_POINT ( 'NONE',  ( -1.049817751779873465, 37.35030165458175588, -26.50542916749582645 ) ) ;
#21500 = CARTESIAN_POINT ( 'NONE',  ( 28.43349137099835389, -65.60227321965514591, -105.5221910860624064 ) ) ;
#21501 = EDGE_CURVE ( 'NONE', #6333, #11658, #21861, .T. ) ;
#21502 = ORIENTED_EDGE ( 'NONE', *, *, #21221, .T. ) ;
#21503 = ORIENTED_EDGE ( 'NONE', *, *, #8674, .T. ) ;
#21504 = EDGE_CURVE ( 'NONE', #1292, #6108, #19848, .T. ) ;
#21505 = CARTESIAN_POINT ( 'NONE',  ( 19.66333377628685142, 38.27269871461067652, 132.3257119126255077 ) ) ;
#21506 = CARTESIAN_POINT ( 'NONE',  ( -1.583189561560253589, 29.24830400313217638, 36.01941156322755688 ) ) ;
#21507 = LINE ( 'NONE', #23551, #15691 ) ;
#21508 = CARTESIAN_POINT ( 'NONE',  ( 25.64681081121879203, 112.3352186517032294, -11.38886654529559017 ) ) ;
#21509 = ORIENTED_EDGE ( 'NONE', *, *, #10823, .F. ) ;
#21510 = CARTESIAN_POINT ( 'NONE',  ( -8.786685647604887350, -25.35688121747534751, -47.14957014837345639 ) ) ;
#21511 = EDGE_CURVE ( 'NONE', #24477, #9366, #27396, .T. ) ;
#21512 = CARTESIAN_POINT ( 'NONE',  ( 10.93730112726003156, 125.1380233598492140, -84.82621002473311478 ) ) ;
#21513 = ORIENTED_EDGE ( 'NONE', *, *, #1377, .F. ) ;
#21514 = EDGE_LOOP ( 'NONE', ( #24244, #10818, #22063, #2294, #11740, #6148 ) ) ;
#21515 = B_SPLINE_CURVE_WITH_KNOTS ( 'NONE', 3,
 ( #10546, #28086, #6237, #10691, #17156, #25947, #14988, #21613 ),
 .UNSPECIFIED., .F., .F.,
 ( 4, 2, 2, 4 ),
 ( 0.000000000000000000, 0.002761524886576667125, 0.005523049773153334251, 0.01104609954630666677 ),
 .UNSPECIFIED. ) ;
#21516 = CARTESIAN_POINT ( 'NONE',  ( -25.21435515916043713, -31.17620025257576799, 15.02493970636179377 ) ) ;
#21517 =( BOUNDED_SURFACE ( )  B_SPLINE_SURFACE ( 3, 1, ( 
 ( #8563, #10584 ),
 ( #17329, #2347 ),
 ( #210, #15446 ),
 ( #4516, #26118 ) ),
 .UNSPECIFIED., .F., .F., .F. ) 
 B_SPLINE_SURFACE_WITH_KNOTS ( ( 4, 4 ),
 ( 2, 2 ),
 ( 0.000000000000000000, 1.000000000000000000 ),
 ( 0.000000000000000000, 1.000000000000000000 ),
 .UNSPECIFIED. ) 
 GEOMETRIC_REPRESENTATION_ITEM ( )  RATIONAL_B_SPLINE_SURFACE ( (
 ( 1.000000000000000000, 1.000000000000000000),
 ( 0.9593753223639863714, 0.9995975284513187731),
 ( 0.9593753223639863714, 0.9995975284513187731),
 ( 1.000000000000000000, 1.000000000000000000) ) ) 
 REPRESENTATION_ITEM ( '' )  SURFACE ( )  );
#21518 = EDGE_CURVE ( 'NONE', #6478, #8163, #2661, .T. ) ;
#21519 = ORIENTED_EDGE ( 'NONE', *, *, #6034, .F. ) ;
#21520 = ORIENTED_EDGE ( 'NONE', *, *, #11144, .T. ) ;
#21521 = CARTESIAN_POINT ( 'NONE',  ( 28.37599760073042532, -1.794331790580228736, 114.7183216384031397 ) ) ;
#21522 = ORIENTED_EDGE ( 'NONE', *, *, #22996, .T. ) ;
#21523 = B_SPLINE_CURVE_WITH_KNOTS ( 'NONE', 3,
 ( #25032, #13343, #22140, #2403 ),
 .UNSPECIFIED., .F., .F.,
 ( 4, 4 ),
 ( 1.906343156168367839E-16, 0.0009910334943227156780 ),
 .UNSPECIFIED. ) ;
#21524 = CARTESIAN_POINT ( 'NONE',  ( 1.833206310202324607, -73.19872434058702027, -125.2945016693818587 ) ) ;
#21525 = CARTESIAN_POINT ( 'NONE',  ( 2.433796855181219243, -74.00833731765649759, 125.2830755159751703 ) ) ;
#21526 = CARTESIAN_POINT ( 'NONE',  ( -1.045287976400383290, 12.68782741917383738, 44.00138577190627842 ) ) ;
#21527 = FACE_OUTER_BOUND ( 'NONE', #11136, .T. ) ;
#21528 = CARTESIAN_POINT ( 'NONE',  ( 25.64681081121879203, -112.2483031020012589, -12.21581276189922427 ) ) ;
#21529 = ORIENTED_EDGE ( 'NONE', *, *, #17252, .T. ) ;
#21530 = CARTESIAN_POINT ( 'NONE',  ( 32.73300124599741423, 113.0038235389606314, -32.68291970228113996 ) ) ;
#21531 = EDGE_CURVE ( 'NONE', #10573, #17409, #19489, .T. ) ;
#21532 = CARTESIAN_POINT ( 'NONE',  ( 1.831572820252008738, -31.13525033585589341, 141.7320553118905195 ) ) ;
#21533 = CARTESIAN_POINT ( 'NONE',  ( 25.64670758986458665, -102.9458331681482406, -46.37945960491978070 ) ) ;
#21534 = ORIENTED_EDGE ( 'NONE', *, *, #3912, .F. ) ;
#21535 = CARTESIAN_POINT ( 'NONE',  ( 16.05277956358235159, 137.6634701901226094, 39.81690014528699351 ) ) ;
#21536 = CARTESIAN_POINT ( 'NONE',  ( 109.1586059443104944, 0.0002768082440195323061, -0.007068659269322301146 ) ) ;
#21537 = ADVANCED_FACE ( 'NONE', ( #12786 ), #15712, .T. ) ;
#21539 = CARTESIAN_POINT ( 'NONE',  ( 26.11404676487257603, -98.61392875273402581, 55.62948129436210110 ) ) ;
#21538 = DIRECTION ( 'NONE',  ( -0.5946245182733607137, 0.6521823330502990457, 0.4701913299128794854 ) ) ;
#21540 = CARTESIAN_POINT ( 'NONE',  ( -25.21435515916025594, 1.749597353048488237E-16, -4.373993382621220594E-17 ) ) ;
#21541 = CARTESIAN_POINT ( 'NONE',  ( -20.20700224038492010, -16.58740185276728241, -24.51628800869040958 ) ) ;
#21542 = CARTESIAN_POINT ( 'NONE',  ( -20.57838717382308147, -18.89542499756516847, -23.26537097894098594 ) ) ;
#21543 = CIRCLE ( 'NONE', #393, 117.6351876552689504 ) ;
#21544 = CARTESIAN_POINT ( 'NONE',  ( -1.045287976400383290, -44.00138577190632816, 12.68782741917368106 ) ) ;
#21545 = ORIENTED_EDGE ( 'NONE', *, *, #9554, .T. ) ;
#21546 = CARTESIAN_POINT ( 'NONE',  ( -55.24198130335446422, -0.001391250620101175178, -0.009190321388310287998 ) ) ;
#21547 = VECTOR ( 'NONE', #14606, 1000.000000000000000 ) ;
#21548 = DIRECTION ( 'NONE',  ( 1.000000000000000000, -6.938893903907226837E-18, 1.734723475976806709E-18 ) ) ;
#21549 = ADVANCED_FACE ( 'NONE', ( #5144 ), #15840, .F. ) ;
#21550 = CARTESIAN_POINT ( 'NONE',  ( 2.430230287190589422, 138.8342928068220203, 43.58368230469437776 ) ) ;
#21551 = CARTESIAN_POINT ( 'NONE',  ( 25.64692232868533139, 112.3263170481597371, 11.47740546588672750 ) ) ;
#21552 = B_SPLINE_CURVE_WITH_KNOTS ( 'NONE', 3,
 ( #24156, #28441, #4554, #9321, #11463, #102, #21980, #8895, #19963, #4706 ),
 .UNSPECIFIED., .F., .F.,
 ( 4, 3, 3, 4 ),
 ( 8.944667923005411581E-18, 0.0002669560319015738272, 0.0005492286108966411284, 0.0008315040496093442472 ),
 .UNSPECIFIED. ) ;
#21553 = CARTESIAN_POINT ( 'NONE',  ( 1.893872463202041168, -45.75900850850099033, 137.7483215415846871 ) ) ;
#21554 = ORIENTED_EDGE ( 'NONE', *, *, #12002, .T. ) ;
#21555 = B_SPLINE_CURVE_WITH_KNOTS ( 'NONE', 3,
 ( #26516, #24379, #4646, #28111, #10714, #4075, #12846, #17179 ),
 .UNSPECIFIED., .F., .F.,
 ( 4, 2, 2, 4 ),
 ( 2.194186273941487696E-16, 0.002761568181852869838, 0.005523136363705520233, 0.01104627272741081495 ),
 .UNSPECIFIED. ) ;
#21556 = B_SPLINE_CURVE_WITH_KNOTS ( 'NONE', 3,
 ( #8929, #6483, #19846, #12406 ),
 .UNSPECIFIED., .F., .F.,
 ( 4, 4 ),
 ( 0.000000000000000000, 0.01077107196513890988 ),
 .UNSPECIFIED. ) ;
#21557 = CARTESIAN_POINT ( 'NONE',  ( -18.41936578851709783, -18.42310649277602508, 38.22933728004711185 ) ) ;
#21558 =( BOUNDED_SURFACE ( )  B_SPLINE_SURFACE ( 3, 1, ( 
 ( #16865, #6215 ),
 ( #10663, #4030 ),
 ( #23912, #1450 ),
 ( #10520, #23781 ) ),
 .UNSPECIFIED., .F., .F., .F. ) 
 B_SPLINE_SURFACE_WITH_KNOTS ( ( 4, 4 ),
 ( 2, 2 ),
 ( 0.000000000000000000, 1.000000000000000000 ),
 ( 0.000000000000000000, 1.000000000000000000 ),
 .UNSPECIFIED. ) 
 GEOMETRIC_REPRESENTATION_ITEM ( )  RATIONAL_B_SPLINE_SURFACE ( (
 ( 1.000000000000000000, 1.000000000000000000),
 ( 0.9934239774497837239, 0.8357310067453919133),
 ( 0.9934239774497837239, 0.8357310067453919133),
 ( 1.000000000000000000, 1.000000000000000000) ) ) 
 REPRESENTATION_ITEM ( '' )  SURFACE ( )  );
#21559 = LINE ( 'NONE', #27769, #8869 ) ;
#21560 = ORIENTED_EDGE ( 'NONE', *, *, #18124, .F. ) ;
#21561 = CARTESIAN_POINT ( 'NONE',  ( -7.078251931573400491, -11.16394717458712726, -50.86685171665407523 ) ) ;
#21562 = CARTESIAN_POINT ( 'NONE',  ( 25.98552792386799482, 65.62435323276291399, -92.15963349013291861 ) ) ;
#21563 = ORIENTED_EDGE ( 'NONE', *, *, #20872, .F. ) ;
#21564 = CARTESIAN_POINT ( 'NONE',  ( -19.53423201713129842, 1.355459634611817431E-16, -3.388649086529543578E-17 ) ) ;
#21565 = CARTESIAN_POINT ( 'NONE',  ( 24.22246935314087324, 0.000000000000000000, -20.00000000000000000 ) ) ;
#21566 = CARTESIAN_POINT ( 'NONE',  ( 14.74894986621300319, -1.023413983156987147E-16, 2.558534957892467869E-17 ) ) ;
#21567 = DIRECTION ( 'NONE',  ( -0.5914120900931443270, 0.6045864222316711389, 0.5335794202785242302 ) ) ;
#21568 = CARTESIAN_POINT ( 'NONE',  ( 1.833485406944043827, -137.8414413349082110, -45.34878176254374438 ) ) ;
#21569 = CARTESIAN_POINT ( 'NONE',  ( -40.00000000000000000, 9.797174393178826052E-15, 80.00000000000000000 ) ) ;
#21570 = CARTESIAN_POINT ( 'NONE',  ( -7.078251931573406708, 47.71415099571806451, -20.86696228105241602 ) ) ;
#21571 = CARTESIAN_POINT ( 'NONE',  ( 25.98552792386798771, 110.8838436908327481, 22.46612985365010573 ) ) ;
#21572 = CARTESIAN_POINT ( 'NONE',  ( -55.24728320129491266, 0.01453410071985307417, -0.0006547948648738343260 ) ) ;
#21573 = CARTESIAN_POINT ( 'NONE',  ( 2.433796855181233454, -16.65276281464466024, -144.5536872373193660 ) ) ;
#21574 = CARTESIAN_POINT ( 'NONE',  ( -1.619063947482194177, 29.22875152547808852, 35.99532424477347092 ) ) ;
#21575 = VERTEX_POINT ( 'NONE', #11778 ) ;
#21576 = VERTEX_POINT ( 'NONE', #2995 ) ;
#21577 = ORIENTED_EDGE ( 'NONE', *, *, #23183, .T. ) ;
#21578 = CARTESIAN_POINT ( 'NONE',  ( 26.11404676487257603, -102.9690087468804762, 47.08215554553482463 ) ) ;
#21579 = DIRECTION ( 'NONE',  ( 0.5946245182733607137, -0.6487139525627716452, -0.4749651461092272986 ) ) ;
#21580 = EDGE_CURVE ( 'NONE', #4784, #8439, #18114, .T. ) ;
#21581 = CARTESIAN_POINT ( 'NONE',  ( 2.063896406836605024, 16.52087515463969680, -144.3268707900445520 ) ) ;
#21582 = DIRECTION ( 'NONE',  ( -0.7637818620346800147, 0.2198041754873925890, 0.6068965246771022004 ) ) ;
#21583 = CARTESIAN_POINT ( 'NONE',  ( -1.539760825549693068, 43.19716078875438825, -16.63252404870369006 ) ) ;
#21584 = CARTESIAN_POINT ( 'NONE',  ( 109.1587776205901861, -0.005390665547495615897, 0.004965871434398026404 ) ) ;
#21585 = CARTESIAN_POINT ( 'NONE',  ( 2.263178113027052518, 98.32595894905985290, -107.1074314657334554 ) ) ;
#21586 = ORIENTED_EDGE ( 'NONE', *, *, #28032, .F. ) ;
#21587 = DIRECTION ( 'NONE',  ( -1.000000000000000000, -0.000000000000000000, -0.000000000000000000 ) ) ;
#21588 = FACE_OUTER_BOUND ( 'NONE', #6560, .T. ) ;
#21589 = CARTESIAN_POINT ( 'NONE',  ( -25.21435515916025594, 1.749597353048488237E-16, -4.373993382621220594E-17 ) ) ;
#21590 = EDGE_CURVE ( 'NONE', #106, #27364, #7485, .T. ) ;
#21591 = EDGE_CURVE ( 'NONE', #8288, #27586, #12600, .T. ) ;
#21592 = B_SPLINE_CURVE_WITH_KNOTS ( 'NONE', 3,
 ( #19902, #26233, #41, #6530, #19750, #24376, #22215 ),
 .UNSPECIFIED., .F., .F.,
 ( 4, 3, 4 ),
 ( 0.000000000000000000, 0.006568092053401806615, 0.02506242213020846293 ),
 .UNSPECIFIED. ) ;
#21593 = CARTESIAN_POINT ( 'NONE',  ( -20.47566338032522992, -25.06314818626703200, -16.24827550219816885 ) ) ;
#21594 = VERTEX_POINT ( 'NONE', #27004 ) ;
#21595 = CARTESIAN_POINT ( 'NONE',  ( -1.619063947482197729, -35.99532424477401094, -29.22875152547743838 ) ) ;
#21596 = DIRECTION ( 'NONE',  ( 0.000000000000000000, 0.000000000000000000, 1.000000000000000000 ) ) ;
#21597 = EDGE_LOOP ( 'NONE', ( #17253, #11667, #10814, #10383 ) ) ;
#21598 = ORIENTED_EDGE ( 'NONE', *, *, #4844, .T. ) ;
#21599 = VERTEX_POINT ( 'NONE', #13493 ) ;
#21600 =( BOUNDED_SURFACE ( )  B_SPLINE_SURFACE ( 3, 1, ( 
 ( #2349, #11154 ),
 ( #5761, #1419 ),
 ( #10227, #27768 ),
 ( #8069, #6277 ) ),
 .UNSPECIFIED., .F., .F., .F. ) 
 B_SPLINE_SURFACE_WITH_KNOTS ( ( 4, 4 ),
 ( 2, 2 ),
 ( 0.000000000000000000, 1.000000000000000000 ),
 ( 0.000000000000000000, 1.000000000000000000 ),
 .UNSPECIFIED. ) 
 GEOMETRIC_REPRESENTATION_ITEM ( )  RATIONAL_B_SPLINE_SURFACE ( (
 ( 1.000000000000000000, 1.000000000000000000),
 ( 0.9960225298536222738, 0.9999952330161893110),
 ( 0.9960225298536222738, 0.9999952330161893110),
 ( 1.000000000000000000, 1.000000000000000000) ) ) 
 REPRESENTATION_ITEM ( '' )  SURFACE ( )  );
#21601 = CARTESIAN_POINT ( 'NONE',  ( 109.1586900883932856, 0.004851151255031853869, -0.005236795036868178467 ) ) ;
#21602 = CARTESIAN_POINT ( 'NONE',  ( -1.619063947482197729, 46.30105812165548684, -2.489035965910316506 ) ) ;
#21603 = CARTESIAN_POINT ( 'NONE',  ( 1.833838848569442570, 72.70900949568773797, 125.5797553397071624 ) ) ;
#21604 = VECTOR ( 'NONE', #21813, 1000.000000000000114 ) ;
#21605 = ADVANCED_FACE ( 'NONE', ( #7316 ), #19701, .F. ) ;
#21606 = CARTESIAN_POINT ( 'NONE',  ( 28.43349137099833968, 80.08535015164038384, -94.99961975860179564 ) ) ;
#21607 = EDGE_LOOP ( 'NONE', ( #9247, #3086, #23149, #8664 ) ) ;
#21608 = CARTESIAN_POINT ( 'NONE',  ( 1.833721034905646308, 58.69612512971785634, -132.7087680342062015 ) ) ;
#21609 = EDGE_CURVE ( 'NONE', #16670, #19810, #22629, .T. ) ;
#21610 = LINE ( 'NONE', #15113, #3234 ) ;
#21611 = CARTESIAN_POINT ( 'NONE',  ( -1.048996300304498419, -14.87787369922200043, -43.31387123529974303 ) ) ;
#21612 = CARTESIAN_POINT ( 'NONE',  ( 1.834118845439484335, 144.2964192726481940, 15.34511559672728964 ) ) ;
#21613 = CARTESIAN_POINT ( 'NONE',  ( -1.619063947482197729, 38.92136151114943488, 25.20140673341330739 ) ) ;
#21614 = CARTESIAN_POINT ( 'NONE',  ( 26.11404676487259024, 97.48350837663691948, -57.58742681967348176 ) ) ;
#21615 = CARTESIAN_POINT ( 'NONE',  ( -4.473127245936431073, -3.196405119333463496, 49.22197550883370809 ) ) ;
#21616 = CARTESIAN_POINT ( 'NONE',  ( 2.430230287190589422, 74.01081053031099088, 125.2872625092165180 ) ) ;
#21617 = CARTESIAN_POINT ( 'NONE',  ( 109.1721716018069657, 0.001583175916620053981, -0.01699510305644695227 ) ) ;
#21618 = ORIENTED_EDGE ( 'NONE', *, *, #21067, .F. ) ;
#21619 = VERTEX_POINT ( 'NONE', #20249 ) ;
#21620 = LINE ( 'NONE', #12981, #6952 ) ;
#21621 = AXIS2_PLACEMENT_3D ( 'NONE', #27886, #16945, #27455 ) ;
#21622 = CARTESIAN_POINT ( 'NONE',  ( 16.05277956358202474, 39.81690014528850696, -137.6634701901227231 ) ) ;
#21623 = EDGE_LOOP ( 'NONE', ( #24923, #9669, #26430, #1652 ) ) ;
#21624 = CIRCLE ( 'NONE', #10622, 151.1787379149930359 ) ;
#21625 = VERTEX_POINT ( 'NONE', #18372 ) ;
#21626 = EDGE_LOOP ( 'NONE', ( #20776, #25300 ) ) ;
#21627 = VECTOR ( 'NONE', #3166, 999.9999999999998863 ) ;
#21628 = CARTESIAN_POINT ( 'NONE',  ( 109.1587776205901577, 0.006729130500857901862, -0.002904816147418943541 ) ) ;
#21629 =( BOUNDED_SURFACE ( )  B_SPLINE_SURFACE ( 3, 1, ( 
 ( #10417, #1616 ),
 ( #24054, #14707 ),
 ( #23518, #19182 ),
 ( #26326, #27953 ) ),
 .UNSPECIFIED., .F., .F., .F. ) 
 B_SPLINE_SURFACE_WITH_KNOTS ( ( 4, 4 ),
 ( 2, 2 ),
 ( 0.000000000000000000, 1.000000000000000000 ),
 ( 0.000000000000000000, 1.000000000000000000 ),
 .UNSPECIFIED. ) 
 GEOMETRIC_REPRESENTATION_ITEM ( )  RATIONAL_B_SPLINE_SURFACE ( (
 ( 1.000000000000000000, 1.000000000000000000),
 ( 0.9956975270656955868, 0.8568959468854907557),
 ( 0.9956975270656955868, 0.8568959468854907557),
 ( 1.000000000000000000, 1.000000000000000000) ) ) 
 REPRESENTATION_ITEM ( '' )  SURFACE ( )  );
#21630 = CARTESIAN_POINT ( 'NONE',  ( 25.70243777736191149, -83.44449745408483921, -76.12033502296601739 ) ) ;
#21631 = DIRECTION ( 'NONE',  ( 1.000000000000000000, -6.938893903907226837E-18, 1.734723475976806709E-18 ) ) ;
#21632 = EDGE_CURVE ( 'NONE', #15681, #6278, #21523, .T. ) ;
#21633 = CARTESIAN_POINT ( 'NONE',  ( -8.786685647604894456, 7.199674155859698388, 53.04920435127174017 ) ) ;
#21634 = EDGE_CURVE ( 'NONE', #15497, #18539, #23243, .T. ) ;
#21635 = CARTESIAN_POINT ( 'NONE',  ( -20.20612092514784663, 8.058517256681097862, -28.48192215759668855 ) ) ;
#21636 = VECTOR ( 'NONE', #14133, 1000.000000000000000 ) ;
#21637 = CARTESIAN_POINT ( 'NONE',  ( -20.90916690077959927, 28.59207721780146727, -27.35210456531384082 ) ) ;
#21638 = AXIS2_PLACEMENT_3D ( 'NONE', #19150, #5784, #16982 ) ;
#21639 = CARTESIAN_POINT ( 'NONE',  ( 2.433796855181205476, 109.1007109081238724, -96.28145139437575040 ) ) ;
#21640 = EDGE_CURVE ( 'NONE', #26700, #24455, #11232, .T. ) ;
#21641 = FACE_OUTER_BOUND ( 'NONE', #27331, .T. ) ;
#21642 = CARTESIAN_POINT ( 'NONE',  ( -1.049819825607602342, 36.75053263699390271, -27.33096219556254169 ) ) ;
#21643 = VECTOR ( 'NONE', #15624, 1000.000000000000000 ) ;
#21644 = VERTEX_POINT ( 'NONE', #9909 ) ;
#21645 = EDGE_LOOP ( 'NONE', ( #11999, #15374, #15396, #11005 ) ) ;
#21647 = CARTESIAN_POINT ( 'NONE',  ( 16.75465622695638146, 39.51671382433948310, 136.6258322711653364 ) ) ;
#21646 = CARTESIAN_POINT ( 'NONE',  ( 24.22246935314087324, -90.00000000000005684, 39.99999999999997158 ) ) ;
#21648 = CARTESIAN_POINT ( 'NONE',  ( 25.64681081121879203, -103.3177883989776547, -45.54494737132326776 ) ) ;
#21649 = DIRECTION ( 'NONE',  ( -1.000000000000000000, -0.000000000000000000, -0.000000000000000000 ) ) ;
#21650 = CARTESIAN_POINT ( 'NONE',  ( 0.000000000000000000, 0.000000000000000000, 0.000000000000000000 ) ) ;
#21651 = ORIENTED_EDGE ( 'NONE', *, *, #10859, .F. ) ;
#21652 = DIRECTION ( 'NONE',  ( 0.000000000000000000, 0.000000000000000000, 1.000000000000000000 ) ) ;
#21653 = CARTESIAN_POINT ( 'NONE',  ( -8.786685647604890903, -37.00619870957961410, -38.68584556812286479 ) ) ;
#21654 = CARTESIAN_POINT ( 'NONE',  ( -1.049819825607588575, -27.33096219556267670, -36.75053263699379613 ) ) ;
#21655 = ORIENTED_EDGE ( 'NONE', *, *, #22168, .T. ) ;
#21656 = ORIENTED_EDGE ( 'NONE', *, *, #12967, .T. ) ;
#21657 = FACE_OUTER_BOUND ( 'NONE', #5117, .T. ) ;
#21658 = CARTESIAN_POINT ( 'NONE',  ( -24.53239521893650021, -3.868435622621272163, 33.71193723315178659 ) ) ;
#21659 = ORIENTED_EDGE ( 'NONE', *, *, #22531, .T. ) ;
#21660 = AXIS2_PLACEMENT_3D ( 'NONE', #6772, #15517, #4317 ) ;
#21661 = AXIS2_PLACEMENT_3D ( 'NONE', #1250, #18815, #10050 ) ;
#21662 = CARTESIAN_POINT ( 'NONE',  ( 16.05277956358201052, 113.1291064380275344, -87.96830019103548182 ) ) ;
#21663 = AXIS2_PLACEMENT_3D ( 'NONE', #27499, #21019, #18142 ) ;
#21664 = ADVANCED_FACE ( 'NONE', ( #21104 ), #17684, .F. ) ;
#21665 = VERTEX_POINT ( 'NONE', #10200 ) ;
#21666 = CARTESIAN_POINT ( 'NONE',  ( -1.031422197589711764, 43.06660437151329290, 15.60268798220593034 ) ) ;
#21667 = VECTOR ( 'NONE', #18453, 999.9999999999998863 ) ;
#21668 = DIRECTION ( 'NONE',  ( -0.7563875759206388771, 0.5490129373055280260, 0.3556158456312881189 ) ) ;
#21669 = CARTESIAN_POINT ( 'NONE',  ( -20.20612091757417161, 27.77903622052274102, 10.22177757278288013 ) ) ;
#21670 = ADVANCED_FACE ( 'NONE', ( #1538 ), #18779, .F. ) ;
#21671 = CARTESIAN_POINT ( 'NONE',  ( -1.056502255334264895, -26.51074901220476576, 37.35734037467662461 ) ) ;
#21672 = LINE ( 'NONE', #19227, #26687 ) ;
#21673 = CARTESIAN_POINT ( 'NONE',  ( 109.1778270068192853, 0.005755170886745419705, 0.007323887274081471339 ) ) ;
#21674 = CARTESIAN_POINT ( 'NONE',  ( 32.73300124599740002, -8.473903470905288060, -117.3295799645430151 ) ) ;
#21675 = ORIENTED_EDGE ( 'NONE', *, *, #1767, .T. ) ;
#21676 = B_SPLINE_CURVE_WITH_KNOTS ( 'NONE', 3,
 ( #13592, #2509, #20073, #355 ),
 .UNSPECIFIED., .F., .F.,
 ( 4, 4 ),
 ( 0.000000000000000000, 0.01077107196513851436 ),
 .UNSPECIFIED. ) ;
#21677 = ADVANCED_FACE ( 'NONE', ( #16666 ), #9808, .F. ) ;
#21678 = CARTESIAN_POINT ( 'NONE',  ( 1.833838848569430802, 125.7577269771232551, 72.40075357737693196 ) ) ;
#21680 = CARTESIAN_POINT ( 'NONE',  ( 26.04756280548352265, -10.72497307632870189, 112.6689254848258628 ) ) ;
#21679 = CARTESIAN_POINT ( 'NONE',  ( 109.1589550718174877, 0.007132058561965951352, 0.002553077953671635102 ) ) ;
#21681 = CARTESIAN_POINT ( 'NONE',  ( -55.24300891470648622, -0.003362556190414485880, 0.009225237711097986765 ) ) ;
#21682 = VERTEX_POINT ( 'NONE', #3696 ) ;
#21683 = ORIENTED_EDGE ( 'NONE', *, *, #426, .T. ) ;
#21684 = CARTESIAN_POINT ( 'NONE',  ( 8.186469777910733825, 19.05650978729195444, 148.1306754055309511 ) ) ;
#21685 = CARTESIAN_POINT ( 'NONE',  ( 1.833691583653525470, -72.86287859464681560, 125.4903330494897062 ) ) ;
#21686 = CARTESIAN_POINT ( 'NONE',  ( 1.831572820252009626, 144.2101521542832643, -16.14965423926062016 ) ) ;
#21687 = CARTESIAN_POINT ( 'NONE',  ( -1.050230346682675231, -43.55772679531839486, 14.15203301556477378 ) ) ;
#21688 = CARTESIAN_POINT ( 'NONE',  ( 25.98552792386800192, -90.89136171349133519, 67.36997957637636603 ) ) ;
#21689 = DIRECTION ( 'NONE',  ( -0.7563875759206389882, -0.3556158456312901173, 0.5490129373055266937 ) ) ;
#21690 =( BOUNDED_SURFACE ( )  B_SPLINE_SURFACE ( 3, 1, ( 
 ( #20127, #20268 ),
 ( #9491, #9628 ),
 ( #9195, #15512 ),
 ( #7058, #2866 ) ),
 .UNSPECIFIED., .F., .F., .F. ) 
 B_SPLINE_SURFACE_WITH_KNOTS ( ( 4, 4 ),
 ( 2, 2 ),
 ( 0.000000000000000000, 1.000000000000000000 ),
 ( 0.000000000000000000, 1.000000000000000000 ),
 .UNSPECIFIED. ) 
 GEOMETRIC_REPRESENTATION_ITEM ( )  RATIONAL_B_SPLINE_SURFACE ( (
 ( 1.000000000000000000, 1.000000000000000000),
 ( 0.9593753223639863714, 0.9995975284513187731),
 ( 0.9593753223639863714, 0.9995975284513187731),
 ( 1.000000000000000000, 1.000000000000000000) ) ) 
 REPRESENTATION_ITEM ( '' )  SURFACE ( )  );
#21691 = VERTEX_POINT ( 'NONE', #20834 ) ;
#21692 = CARTESIAN_POINT ( 'NONE',  ( 1.833691583653491941, -45.17974255430909380, 137.8971124741067058 ) ) ;
#21693 = CARTESIAN_POINT ( 'NONE',  ( 109.1587776205901861, 0.0006832286435016865327, -0.007297420966932449682 ) ) ;
#21694 = CARTESIAN_POINT ( 'NONE',  ( -8.786685647604890903, 47.14957014837354876, -25.35688121747519119 ) ) ;
#21695 = CARTESIAN_POINT ( 'NONE',  ( -20.20612091757422490, -1.137293889216157705, 29.57813639663779171 ) ) ;
#21696 = VERTEX_POINT ( 'NONE', #12471 ) ;
#21697 = CARTESIAN_POINT ( 'NONE',  ( 1.834118845439484335, -138.0627591860432801, 44.67218053242348930 ) ) ;
#21698 = CARTESIAN_POINT ( 'NONE',  ( 109.1778270068192853, -0.005755170886745368530, -0.007323887274081511238 ) ) ;
#21699 = B_SPLINE_CURVE_WITH_KNOTS ( 'NONE', 3,
 ( #16623, #388, #5532, #18772, #10153, #4857, #25413 ),
 .UNSPECIFIED., .F., .F.,
 ( 4, 3, 4 ),
 ( 1.868354362588067661E-17, 0.009512539173626417474, 0.02506242213020845253 ),
 .UNSPECIFIED. ) ;
#21700 = ORIENTED_EDGE ( 'NONE', *, *, #12923, .T. ) ;
#21701 = CARTESIAN_POINT ( 'NONE',  ( -28.13707043255157103, 22.00298671236748760, 6.342158660426773231 ) ) ;
#21702 = EDGE_CURVE ( 'NONE', #711, #710, #14996, .T. ) ;
#21703 = VERTEX_POINT ( 'NONE', #14193 ) ;
#21704 = CARTESIAN_POINT ( 'NONE',  ( -1.045287976400383290, -36.12803364096628655, -28.14015102489793918 ) ) ;
#21705 = CARTESIAN_POINT ( 'NONE',  ( 1.831572820252009626, -97.82994539998308881, -107.1759352627516222 ) ) ;
#21706 = ADVANCED_FACE ( 'NONE', ( #27446 ), #21735, .F. ) ;
#21707 = LINE ( 'NONE', #17239, #17147 ) ;
#21708 = CIRCLE ( 'NONE', #21255, 80.00000000000000000 ) ;
#21709 = CARTESIAN_POINT ( 'NONE',  ( -1.048171036023513025, 36.44209502233747600, 27.73816396939524509 ) ) ;
#21710 = CARTESIAN_POINT ( 'NONE',  ( -28.41354790283022069, -21.64275480268742058, 8.345538364877306492 ) ) ;
#21711 = VECTOR ( 'NONE', #8129, 1000.000000000000227 ) ;
#21712 = EDGE_CURVE ( 'NONE', #9601, #19089, #16393, .T. ) ;
#21713 = DIRECTION ( 'NONE',  ( -1.000000000000000000, -0.000000000000000000, -0.000000000000000000 ) ) ;
#21714 = CARTESIAN_POINT ( 'NONE',  ( -20.20612092514784663, 28.48192215759677737, 8.058517256680804763 ) ) ;
#21715 = CARTESIAN_POINT ( 'NONE',  ( -5.986830583229489022, -4.559539818181495896, -50.53158596890440180 ) ) ;
#21716 = CARTESIAN_POINT ( 'NONE',  ( -4.780792508754321268, 3.764354093953580449, -49.38761389561002346 ) ) ;
#21717 = CARTESIAN_POINT ( 'NONE',  ( 94.22246935314088034, 70.00000000000001421, -12.50000000000000888 ) ) ;
#21718 = EDGE_CURVE ( 'NONE', #26175, #18662, #5759, .T. ) ;
#21719 = CARTESIAN_POINT ( 'NONE',  ( 30.58324630866351157, 83.81536267638941240, 87.19147450740381089 ) ) ;
#21720 = CARTESIAN_POINT ( 'NONE',  ( 5.340103556456538669, -71.72120378849517408, -128.8311297043953232 ) ) ;
#21721 = CARTESIAN_POINT ( 'NONE',  ( 32.73300124599732897, 117.3295799645430151, 8.473903470906510194 ) ) ;
#21722 = ORIENTED_EDGE ( 'NONE', *, *, #14128, .F. ) ;
#21723 = ORIENTED_EDGE ( 'NONE', *, *, #14733, .F. ) ;
#21724 = VERTEX_POINT ( 'NONE', #6018 ) ;
#21725 = CARTESIAN_POINT ( 'NONE',  ( -1.050229599974472627, -43.63650726458052986, 13.90955673306172002 ) ) ;
#21726 = CARTESIAN_POINT ( 'NONE',  ( 32.73300124599735739, -105.8473486001054482, 51.32617430724869223 ) ) ;
#21727 = CARTESIAN_POINT ( 'NONE',  ( 10.93730112725971004, 10.89264110825002163, 150.7858122213661147 ) ) ;
#21728 = CARTESIAN_POINT ( 'NONE',  ( 1.833485406944043827, -141.8265699653865113, -30.69200235379080510 ) ) ;
#21729 = CARTESIAN_POINT ( 'NONE',  ( 25.64681081121879203, -91.59071981940525120, -66.03065707439029097 ) ) ;
#21730 = DIRECTION ( 'NONE',  ( -1.000000000000000000, 0.000000000000000000, 0.000000000000000000 ) ) ;
#21731 = CARTESIAN_POINT ( 'NONE',  ( 16.05277956358202829, -53.98852998724671437, 132.7473359121864291 ) ) ;
#21732 = ORIENTED_EDGE ( 'NONE', *, *, #7530, .T. ) ;
#21733 = CARTESIAN_POINT ( 'NONE',  ( 10.93730112725932635, 0.000000000000000000, 0.000000000000000000 ) ) ;
#21734 = CARTESIAN_POINT ( 'NONE',  ( 28.37603512858357035, -114.2774673387025217, -10.20681926544481044 ) ) ;
#21735 =( BOUNDED_SURFACE ( )  B_SPLINE_SURFACE ( 3, 1, ( 
 ( #25303, #12748 ),
 ( #17214, #21532 ),
 ( #8874, #23585 ),
 ( #11029, #1949 ) ),
 .UNSPECIFIED., .F., .F., .F. ) 
 B_SPLINE_SURFACE_WITH_KNOTS ( ( 4, 4 ),
 ( 2, 2 ),
 ( 0.000000000000000000, 1.000000000000000000 ),
 ( 0.000000000000000000, 1.000000000000000000 ),
 .UNSPECIFIED. ) 
 GEOMETRIC_REPRESENTATION_ITEM ( )  RATIONAL_B_SPLINE_SURFACE ( (
 ( 1.000000000000000000, 1.000000000000000000),
 ( 0.9956975270656955868, 0.8568959468854907557),
 ( 0.9956975270656955868, 0.8568959468854907557),
 ( 1.000000000000000000, 1.000000000000000000) ) ) 
 REPRESENTATION_ITEM ( '' )  SURFACE ( )  );
#21736 = FACE_OUTER_BOUND ( 'NONE', #13646, .T. ) ;
#21737 = B_SPLINE_CURVE_WITH_KNOTS ( 'NONE', 3,
 ( #4150, #6329, #19683, #21434 ),
 .UNSPECIFIED., .F., .F.,
 ( 4, 4 ),
 ( 1.956780383866537384E-16, 0.001982023823822938111 ),
 .UNSPECIFIED. ) ;
#21738 = AXIS2_PLACEMENT_3D ( 'NONE', #11683, #7095, #15991 ) ;
#21739 = B_SPLINE_CURVE_WITH_KNOTS ( 'NONE', 3,
 ( #23303, #16374, #14638, #11918 ),
 .UNSPECIFIED., .F., .F.,
 ( 4, 4 ),
 ( 0.0009910334943227156780, 0.001982023823822944616 ),
 .UNSPECIFIED. ) ;
#21740 = CARTESIAN_POINT ( 'NONE',  ( 6.224689322667630975, -76.23997225729357297, 126.9212313063842430 ) ) ;
#21741 = CIRCLE ( 'NONE', #8872, 117.6351876552689504 ) ;
#21742 = CIRCLE ( 'NONE', #27717, 34.60786435723138510 ) ;
#21743 = ORIENTED_EDGE ( 'NONE', *, *, #23530, .T. ) ;
#21744 = CARTESIAN_POINT ( 'NONE',  ( 1.833206308920084293, 44.13245285122266637, 138.2356393957897751 ) ) ;
#21745 = CARTESIAN_POINT ( 'NONE',  ( 25.64700659047697684, -11.57609179463883464, -112.3162501909140474 ) ) ;
#21746 = ORIENTED_EDGE ( 'NONE', *, *, #12887, .F. ) ;
#21747 = ORIENTED_EDGE ( 'NONE', *, *, #10988, .T. ) ;
#21748 = ORIENTED_EDGE ( 'NONE', *, *, #8205, .T. ) ;
#21749 = EDGE_CURVE ( 'NONE', #9286, #16092, #12610, .T. ) ;
#21750 = CARTESIAN_POINT ( 'NONE',  ( -55.25297051322618813, -0.01483298743814594547, 0.001818774723749421287 ) ) ;
#21751 = CARTESIAN_POINT ( 'NONE',  ( -20.57838717382308147, -27.96569011373093971, -10.78122205916989529 ) ) ;
#21752 = EDGE_CURVE ( 'NONE', #23016, #11485, #5369, .T. ) ;
#21753 = CARTESIAN_POINT ( 'NONE',  ( -55.24271866751342941, 0.004256484107793641683, 0.008488649505346114801 ) ) ;
#21754 = B_SPLINE_CURVE_WITH_KNOTS ( 'NONE', 3,
 ( #27162, #7471, #5295, #7764, #3141, #9916, #1256, #14352, #11919, #10056 ),
 .UNSPECIFIED., .F., .F.,
 ( 4, 3, 3, 4 ),
 ( 1.962615573354718958E-17, 0.0002669559177086156237, 0.0005339118354150979712, 0.001067817517169166418 ),
 .UNSPECIFIED. ) ;
#21755 = CIRCLE ( 'NONE', #18558, 53.53553390275978785 ) ;
#21756 = VECTOR ( 'NONE', #6621, 1000.000000000000114 ) ;
#21757 = CARTESIAN_POINT ( 'NONE',  ( 21.16825799904901473, 87.29264348877980240, -103.5479404090027629 ) ) ;
#21758 = ORIENTED_EDGE ( 'NONE', *, *, #13997, .T. ) ;
#21759 = ORIENTED_EDGE ( 'NONE', *, *, #10839, .T. ) ;
#21760 = CARTESIAN_POINT ( 'NONE',  ( -24.53237795827031320, 33.25734978085278470, 6.738475012719742807 ) ) ;
#21761 = CARTESIAN_POINT ( 'NONE',  ( 1.833809397773872307, -44.67209459544969974, -138.0624841332892174 ) ) ;
#21762 = DIRECTION ( 'NONE',  ( -0.5914120900931443270, -0.6942916636548165377, 0.4101107478122046346 ) ) ;
#21763 = CARTESIAN_POINT ( 'NONE',  ( -8.786685647604890903, 25.35688121747502066, -47.14957014837363403 ) ) ;
#21764 = CARTESIAN_POINT ( 'NONE',  ( -1.056502255334264895, 37.35734037467673119, 26.51074901220462721 ) ) ;
#21765 = FACE_OUTER_BOUND ( 'NONE', #4062, .T. ) ;
#21766 = CARTESIAN_POINT ( 'NONE',  ( -1.619063947482197729, 11.94059994246222622, 44.80407745103770623 ) ) ;
#21767 = CARTESIAN_POINT ( 'NONE',  ( -1.044557008772714068, -44.03203053429562885, 12.57891310333395118 ) ) ;
#21768 = DIRECTION ( 'NONE',  ( -1.000000000000000000, -0.000000000000000000, -0.000000000000000000 ) ) ;
#21769 = ORIENTED_EDGE ( 'NONE', *, *, #23496, .T. ) ;
#21770 = VECTOR ( 'NONE', #3469, 1000.000000000000000 ) ;
#21771 = VERTEX_POINT ( 'NONE', #25730 ) ;
#21772 = CARTESIAN_POINT ( 'NONE',  ( 109.1586900883932856, 0.006561743627143329545, -0.002810909342011622906 ) ) ;
#21773 = CARTESIAN_POINT ( 'NONE',  ( 32.73300124599738581, 32.68291970228383292, -113.0038235389598782 ) ) ;
#21774 = VERTEX_POINT ( 'NONE', #23731 ) ;
#21776 =( BOUNDED_SURFACE ( )  B_SPLINE_SURFACE ( 3, 1, ( 
 ( #14263, #23086 ),
 ( #9253, #18009 ),
 ( #26797, #20320 ),
 ( #15867, #24676 ) ),
 .UNSPECIFIED., .F., .F., .F. ) 
 B_SPLINE_SURFACE_WITH_KNOTS ( ( 4, 4 ),
 ( 2, 2 ),
 ( 0.000000000000000000, 1.000000000000000000 ),
 ( 0.000000000000000000, 1.000000000000000000 ),
 .UNSPECIFIED. ) 
 GEOMETRIC_REPRESENTATION_ITEM ( )  RATIONAL_B_SPLINE_SURFACE ( (
 ( 1.000000000000000000, 1.000000000000000000),
 ( 0.9934239774497838349, 0.8357310067453913582),
 ( 0.9934239774497838349, 0.8357310067453913582),
 ( 1.000000000000000000, 1.000000000000000000) ) ) 
 REPRESENTATION_ITEM ( '' )  SURFACE ( )  );
#21775 = PRODUCT_DEFINITION_FORMATION_WITH_SPECIFIED_SOURCE ( 'ANY', '', #32, .NOT_KNOWN. ) ;
#21777 = VERTEX_POINT ( 'NONE', #8448 ) ;
#21778 = ORIENTED_EDGE ( 'NONE', *, *, #9103, .T. ) ;
#21779 = CARTESIAN_POINT ( 'NONE',  ( 1.832998868059890096, -84.86110816369526333, -117.7096351258396254 ) ) ;
#21780 = EDGE_CURVE ( 'NONE', #14585, #771, #12092, .T. ) ;
#21781 = CARTESIAN_POINT ( 'NONE',  ( 109.1589550718174877, 0.005477029346537774616, 0.005233222325298243251 ) ) ;
#21782 = EDGE_CURVE ( 'NONE', #21644, #24473, #2612, .T. ) ;
#21783 = CARTESIAN_POINT ( 'NONE',  ( 1.833485406944043827, -144.2578170162064168, 15.69895494453337648 ) ) ;
#21784 = CARTESIAN_POINT ( 'NONE',  ( 109.1586900883932856, -0.003481399864218472865, 0.006231977675084978893 ) ) ;
#21785 = EDGE_CURVE ( 'NONE', #17023, #26786, #22198, .T. ) ;
#21786 = B_SPLINE_CURVE_WITH_KNOTS ( 'NONE', 3,
 ( #2199, #15302, #26398, #10732, #19496, #8430, #17195, #24116, #28125, #4379, #23979, #1925, #17464 ),
 .UNSPECIFIED., .F., .F.,
 ( 4, 3, 3, 3, 4 ),
 ( 1.250926888277100303E-17, 0.0007657099931970583933, 0.001531419946797919589, 0.002296279302920155134, 0.003061450627205745088 ),
 .UNSPECIFIED. ) ;
#21787 = CONICAL_SURFACE ( 'NONE', #12592, 117.6351876552689504, 0.9945805576725580410 ) ;
#21788 = CARTESIAN_POINT ( 'NONE',  ( -20.90916690077965612, 5.322316104228523415, 39.20864005633514893 ) ) ;
#21789 = CARTESIAN_POINT ( 'NONE',  ( -28.41354790283022069, -21.64275480268754137, -8.345538364876993853 ) ) ;
#21790 = DIRECTION ( 'NONE',  ( 0.000000000000000000, 0.000000000000000000, 1.000000000000000000 ) ) ;
#21791 = FACE_OUTER_BOUND ( 'NONE', #26581, .T. ) ;
#21792 = CARTESIAN_POINT ( 'NONE',  ( 109.1778270068192853, -0.003210287141653740423, -0.008743876326162627541 ) ) ;
#21793 = CARTESIAN_POINT ( 'NONE',  ( 25.64660436782563835, 112.9095526718339784, -0.5800540083555767445 ) ) ;
#21794 = ORIENTED_EDGE ( 'NONE', *, *, #1624, .F. ) ;
#21795 = ORIENTED_EDGE ( 'NONE', *, *, #6864, .F. ) ;
#21797 = CARTESIAN_POINT ( 'NONE',  ( 13.84597867724968623, 40.76072889493758566, 140.9259526407711292 ) ) ;
#21796 = CARTESIAN_POINT ( 'NONE',  ( 28.37599760073042887, 114.2774414139536390, -10.20682761621814727 ) ) ;
#21798 = CARTESIAN_POINT ( 'NONE',  ( -1.031422197589716205, -37.93675465142454328, 25.67058493451484225 ) ) ;
#21799 = CARTESIAN_POINT ( 'NONE',  ( -1.155001620486252101, -42.97366440495923001, -16.13799328198405902 ) ) ;
#21800 = DIRECTION ( 'NONE',  ( -1.000000000000000000, -0.000000000000000000, -0.000000000000000000 ) ) ;
#21801 = VERTEX_POINT ( 'NONE', #8582 ) ;
#21802 = DIRECTION ( 'NONE',  ( -1.000000000000000000, -0.000000000000000000, -0.000000000000000000 ) ) ;
#21803 = CARTESIAN_POINT ( 'NONE',  ( 32.73300124599739291, 81.52272205837319063, -84.80615050150287004 ) ) ;
#21804 = CARTESIAN_POINT ( 'NONE',  ( -1.045287976400351981, 12.68782741917293855, -44.00138577190654132 ) ) ;
#21805 = ORIENTED_EDGE ( 'NONE', *, *, #15572, .F. ) ;
#21806 = ORIENTED_EDGE ( 'NONE', *, *, #24449, .T. ) ;
#21807 = CARTESIAN_POINT ( 'NONE',  ( -6.588769196390764193, -11.07780292579730208, -50.13301368233293687 ) ) ;
#21808 = EDGE_CURVE ( 'NONE', #384, #4332, #24964, .T. ) ;
#21809 = ORIENTED_EDGE ( 'NONE', *, *, #5325, .T. ) ;
#21810 = CARTESIAN_POINT ( 'NONE',  ( 25.65782528836480836, 107.2118488517900943, 35.44279022896523657 ) ) ;
#21811 = EDGE_LOOP ( 'NONE', ( #16628, #451 ) ) ;
#21812 = EDGE_CURVE ( 'NONE', #14642, #9224, #6571, .T. ) ;
#21813 = DIRECTION ( 'NONE',  ( 0.7637818620346800147, 0.6451161201712181104, 0.02150485345384620800 ) ) ;
#21814 = EDGE_LOOP ( 'NONE', ( #24509, #4850, #18211, #22275, #23714, #5206 ) ) ;
#21815 = CARTESIAN_POINT ( 'NONE',  ( -1.583189561560255143, 43.29471907393764951, 16.68617981233656877 ) ) ;
#21816 = FACE_OUTER_BOUND ( 'NONE', #8861, .T. ) ;
#21817 = DIRECTION ( 'NONE',  ( 0.000000000000000000, 5.223019709708190374E-21, -1.000000000000000000 ) ) ;
#21818 = CARTESIAN_POINT ( 'NONE',  ( 32.73300124599732186, 0.000000000000000000, 0.000000000000000000 ) ) ;
#21819 = LINE ( 'NONE', #2077, #7890 ) ;
#21820 = CARTESIAN_POINT ( 'NONE',  ( 10.93730112725932813, 151.0983828010088246, -4.928439153520510985 ) ) ;
#21821 = CARTESIAN_POINT ( 'NONE',  ( 25.70243777736188306, -112.2504268534933374, -12.53519966262598473 ) ) ;
#21822 = DIRECTION ( 'NONE',  ( 0.000000000000000000, 0.000000000000000000, 1.000000000000000000 ) ) ;
#21824 = CARTESIAN_POINT ( 'NONE',  ( 25.64660436782541808, -11.22538561721967376, 112.3516544824821182 ) ) ;
#21823 = CARTESIAN_POINT ( 'NONE',  ( 2.063896406836605024, -13.84738934186092862, -144.6078654718903067 ) ) ;
#21825 = CARTESIAN_POINT ( 'NONE',  ( 25.64704443564078318, -56.57116289738674908, 97.71717520928662282 ) ) ;
#21826 = VERTEX_POINT ( 'NONE', #13039 ) ;
#21827 = ORIENTED_EDGE ( 'NONE', *, *, #6565, .T. ) ;
#21828 = CARTESIAN_POINT ( 'NONE',  ( -25.21435515916025594, 1.749597353048488237E-16, -4.373993382621220594E-17 ) ) ;
#21829 = CARTESIAN_POINT ( 'NONE',  ( 1.894214914920958392, -31.11059045489028563, -141.7768822502890202 ) ) ;
#21830 = CARTESIAN_POINT ( 'NONE',  ( 1.833485406944057594, 44.33323125130110043, -138.1714136985304151 ) ) ;
#21831 = CARTESIAN_POINT ( 'NONE',  ( 109.1624594426973260, 0.01102230012606003617, -0.01154818537150963803 ) ) ;
#21832 = CARTESIAN_POINT ( 'NONE',  ( -4.473127245936431073, 45.82513704981569447, 18.25038884639822712 ) ) ;
#21833 = ORIENTED_EDGE ( 'NONE', *, *, #27521, .T. ) ;
#21834 = CARTESIAN_POINT ( 'NONE',  ( 25.64708228042119131, -34.85404436489419311, -107.3971738194635321 ) ) ;
#21835 = CARTESIAN_POINT ( 'NONE',  ( -8.786685647604896232, 25.35688121747570278, 47.14957014837326454 ) ) ;
#21836 = ADVANCED_FACE ( 'NONE', ( #10888 ), #24695, .F. ) ;
#21837 = CARTESIAN_POINT ( 'NONE',  ( -1.619063947482197729, -35.99532424477357750, 29.22875152547795707 ) ) ;
#21838 = CARTESIAN_POINT ( 'NONE',  ( -23.79248802219723302, -33.03370827286728684, 3.207402715357496881 ) ) ;
#21839 = CARTESIAN_POINT ( 'NONE',  ( 1.833750490713712322, 117.2391074582372568, 85.50916867388838227 ) ) ;
#21840 = ORIENTED_EDGE ( 'NONE', *, *, #2831, .T. ) ;
#21841 = CARTESIAN_POINT ( 'NONE',  ( 109.1587776205901861, -0.003736572840496174032, -0.006305329297950490811 ) ) ;
#21842 = ADVANCED_FACE ( 'NONE', ( #2811 ), #2395, .T. ) ;
#21843 = EDGE_CURVE ( 'NONE', #1309, #20568, #15646, .T. ) ;
#21844 = FACE_OUTER_BOUND ( 'NONE', #19026, .T. ) ;
#21845 = CARTESIAN_POINT ( 'NONE',  ( 1.833485406944057594, -59.50871042846138437, -132.3460930279897241 ) ) ;
#21846 = EDGE_LOOP ( 'NONE', ( #25199, #7820, #25183, #20734 ) ) ;
#21847 = CARTESIAN_POINT ( 'NONE',  ( 109.1592201516379674, -0.007302213399787572945, -0.002913740842103159506 ) ) ;
#21848 = B_SPLINE_CURVE_WITH_KNOTS ( 'NONE', 3,
 ( #21648, #17455, #8149, #19488, #14887, #16916, #23550, #17318, #3813, #6134 ),
 .UNSPECIFIED., .F., .F.,
 ( 4, 3, 3, 4 ),
 ( 1.387778780781445676E-17, 0.0002669560319015670509, 0.0005492286108966479589, 0.0008315040496093511861 ),
 .UNSPECIFIED. ) ;
#21849 = CARTESIAN_POINT ( 'NONE',  ( -1.058197053496161999, -36.00048521498973031, -28.32422455455065347 ) ) ;
#21850 = DIRECTION ( 'NONE',  ( 0.000000000000000000, 0.000000000000000000, 1.000000000000000000 ) ) ;
#21851 = VERTEX_POINT ( 'NONE', #17633 ) ;
#21852 = CARTESIAN_POINT ( 'NONE',  ( -1.044556982611271279, -12.57890920527746381, 44.03203163107538387 ) ) ;
#21853 = CARTESIAN_POINT ( 'NONE',  ( 5.340103579038220971, -143.7310399932979408, 32.90561047415553020 ) ) ;
#21854 = CARTESIAN_POINT ( 'NONE',  ( -1.113427685307001314, -45.82016658690749722, 1.967672929087657785 ) ) ;
#21855 = B_SPLINE_CURVE_WITH_KNOTS ( 'NONE', 3,
 ( #16260, #22613, #13662, #22464 ),
 .UNSPECIFIED., .F., .F.,
 ( 4, 4 ),
 ( 1.892757412642747770E-16, 0.001982023823822945049 ),
 .UNSPECIFIED. ) ;
#21856 = CARTESIAN_POINT ( 'NONE',  ( 1.833838848569429247, -138.0625820091621563, -44.67212175381978057 ) ) ;
#21857 = CARTESIAN_POINT ( 'NONE',  ( -6.574463467970651287, -5.014313797967385966, -51.07975593197902953 ) ) ;
#21858 = CARTESIAN_POINT ( 'NONE',  ( -1.048171036023500147, -1.020520027228813298, 45.78635789057867100 ) ) ;
#21859 = CARTESIAN_POINT ( 'NONE',  ( 2.430230287190592531, -98.44218333480698391, -107.1617224697474313 ) ) ;
#21860 = CARTESIAN_POINT ( 'NONE',  ( 21.16825799904930605, 93.85612807858977646, 97.63815233965053153 ) ) ;
#21861 = LINE ( 'NONE', #4015, #16669 ) ;
#21862 = CARTESIAN_POINT ( 'NONE',  ( 28.37603512858359522, 114.2774673387025359, 10.20681926544401996 ) ) ;
#21863 = ORIENTED_EDGE ( 'NONE', *, *, #3223, .T. ) ;
#21864 = VERTEX_POINT ( 'NONE', #13884 ) ;
#21865 = CARTESIAN_POINT ( 'NONE',  ( 25.64681081121879203, 102.9795863647028682, 46.30456157731362765 ) ) ;
#21866 = APPLICATION_CONTEXT ( 'automotive_design' ) ;
#21867 = CARTESIAN_POINT ( 'NONE',  ( -20.47566262905010603, 28.85746289809577547, -7.708089517695290382 ) ) ;
#21868 = CARTESIAN_POINT ( 'NONE',  ( -1.619063947482197729, -29.22875152547730337, 35.99532424477411041 ) ) ;
#21869 = CARTESIAN_POINT ( 'NONE',  ( 9.884929003653626367, -144.4113244745768725, -42.50195158091179337 ) ) ;
#21870 = CARTESIAN_POINT ( 'NONE',  ( 1.833485406944043827, 73.01664920993141550, -125.4007332306537563 ) ) ;
#21871 = CARTESIAN_POINT ( 'NONE',  ( -55.25719721206881729, 0.01041086141212550775, -0.004044147484878501606 ) ) ;
#21872 = CARTESIAN_POINT ( 'NONE',  ( -22.23342874802669655, -24.24669006619387090, -20.31166691703116811 ) ) ;
#21873 = VERTEX_POINT ( 'NONE', #19944 ) ;
#21874 = CARTESIAN_POINT ( 'NONE',  ( -25.21435515916043713, -6.169479169075696490, -34.05351380035330777 ) ) ;
#21875 = CARTESIAN_POINT ( 'NONE',  ( 9.884929003653608603, 57.36421526887158961, 139.1775604444705721 ) ) ;
#21876 = CARTESIAN_POINT ( 'NONE',  ( 6.224689322667630975, -43.30635742325279125, -141.5842213414017863 ) ) ;
#21877 = EDGE_CURVE ( 'NONE', #4332, #7007, #19442, .T. ) ;
#21878 = CARTESIAN_POINT ( 'NONE',  ( -1.056502255334265339, -37.35734037467615565, 26.51074901220544433 ) ) ;
#21879 = EDGE_CURVE ( 'NONE', #13376, #6084, #3994, .T. ) ;
#21880 = CARTESIAN_POINT ( 'NONE',  ( -6.574463467970683261, 44.27173031830773908, 25.96726214983142000 ) ) ;
#21882 = EDGE_CURVE ( 'NONE', #11326, #16414, #6389, .T. ) ;
#21881 = CARTESIAN_POINT ( 'NONE',  ( 1.833750490713699888, -108.0159692407137015, 96.89879583303815025 ) ) ;
#21883 = FACE_OUTER_BOUND ( 'NONE', #13552, .T. ) ;
#21884 = EDGE_LOOP ( 'NONE', ( #21205, #5738, #14256, #21284 ) ) ;
#21885 = B_SPLINE_CURVE_WITH_KNOTS ( 'NONE', 3,
 ( #27275, #18501, #11451, #13744, #14168, #2819, #5116, #2668 ),
 .UNSPECIFIED., .F., .F.,
 ( 4, 2, 2, 4 ),
 ( 0.000000000000000000, 0.002761524886576637201, 0.005523049773153274403, 0.01104609954630654707 ),
 .UNSPECIFIED. ) ;
#21886 = EDGE_CURVE ( 'NONE', #22931, #24940, #27703, .T. ) ;
#21887 = ORIENTED_EDGE ( 'NONE', *, *, #24357, .F. ) ;
#21888 = ORIENTED_EDGE ( 'NONE', *, *, #17788, .F. ) ;
#21889 = CARTESIAN_POINT ( 'NONE',  ( -20.20612091757422846, -18.30568244821359869, 23.26073043121652262 ) ) ;
#21890 = CARTESIAN_POINT ( 'NONE',  ( -8.786685647604890903, 23.24040270374391426, -48.22796981442777309 ) ) ;
#21891 = ORIENTED_EDGE ( 'NONE', *, *, #26089, .T. ) ;
#21892 = CARTESIAN_POINT ( 'NONE',  ( 55.49584447822657296, -66.16986612640796750, 29.75369869230931386 ) ) ;
#21893 = CARTESIAN_POINT ( 'NONE',  ( 8.186469829614267724, -113.2805153378644576, 97.33125097511842228 ) ) ;
#21894 = EDGE_LOOP ( 'NONE', ( #27413, #23916, #27457, #28442 ) ) ;
#21895 = CARTESIAN_POINT ( 'NONE',  ( -1.058473599757816963, -25.48501014712370960, 38.06357893967457784 ) ) ;
#21896 = ORIENTED_EDGE ( 'NONE', *, *, #20701, .F. ) ;
#21897 = CARTESIAN_POINT ( 'NONE',  ( -1.050231094221214301, -43.63617436699747287, -13.91061116148175536 ) ) ;
#21898 = CARTESIAN_POINT ( 'NONE',  ( 1.833603222531973387, -44.41798579679444003, -138.1443021179085804 ) ) ;
#21899 = CARTESIAN_POINT ( 'NONE',  ( -1.031422197589716205, -44.01264471863839134, 12.69107518035547955 ) ) ;
#21900 = CARTESIAN_POINT ( 'NONE',  ( -6.574463467970649511, 25.96726214983191383, -44.27173031830743355 ) ) ;
#21901 = CARTESIAN_POINT ( 'NONE',  ( 1.833721034905633429, 96.83259691102649924, -108.0754384393924852 ) ) ;
#21902 = CARTESIAN_POINT ( 'NONE',  ( 5.340103556456499589, -57.86178752079229071, -135.6222865117687775 ) ) ;
#21903 = CARTESIAN_POINT ( 'NONE',  ( -55.24390624410018802, -0.01032895241566962087, 0.001451500391950532459 ) ) ;
#21904 = EDGE_CURVE ( 'NONE', #2974, #3159, #16017, .T. ) ;
#21905 = DIRECTION ( 'NONE',  ( 0.000000000000000000, 5.223019709707975211E-21, -1.000000000000000000 ) ) ;
#21906 = CARTESIAN_POINT ( 'NONE',  ( -8.786685647604885574, 6.096987947571466530E-17, -1.524246986892866633E-17 ) ) ;
#21907 = LINE ( 'NONE', #6241, #19447 ) ;
#21908 = VERTEX_POINT ( 'NONE', #9146 ) ;
#21909 = ORIENTED_EDGE ( 'NONE', *, *, #3196, .T. ) ;
#21911 = EDGE_CURVE ( 'NONE', #24805, #17826, #13260, .T. ) ;
#21910 = CARTESIAN_POINT ( 'NONE',  ( 2.433796855181233454, -109.1007109081219539, -96.28145139437795308 ) ) ;
#21912 = CARTESIAN_POINT ( 'NONE',  ( 26.28373643307406837, 35.44121223575024970, -122.5382646256986305 ) ) ;
#21913 = ORIENTED_EDGE ( 'NONE', *, *, #28078, .T. ) ;
#21914 = B_SPLINE_CURVE_WITH_KNOTS ( 'NONE', 3,
 ( #7925, #14078, #12217, #14209 ),
 .UNSPECIFIED., .F., .F.,
 ( 4, 4 ),
 ( 6.938893903907228378E-18, 0.008383560773332719013 ),
 .UNSPECIFIED. ) ;
#21915 = ORIENTED_EDGE ( 'NONE', *, *, #9464, .F. ) ;
#21916 = EDGE_LOOP ( 'NONE', ( #17211, #5374, #16882, #24766 ) ) ;
#21917 = CARTESIAN_POINT ( 'NONE',  ( 32.73300124599735028, 84.80615050150375112, 81.52272205837232377 ) ) ;
#21918 = CARTESIAN_POINT ( 'NONE',  ( 25.98107933586725338, 10.73978443746734079, 112.6229961579375782 ) ) ;
#21919 = CARTESIAN_POINT ( 'NONE',  ( -1.044557008772710072, -45.76404748504492659, -1.643388457097728184 ) ) ;
#21920 = CARTESIAN_POINT ( 'NONE',  ( -1.239374126674604337, 38.61989855450975995, 25.08410696974200604 ) ) ;
#21921 = DIRECTION ( 'NONE',  ( -1.000000000000000000, -0.000000000000000000, -0.000000000000000000 ) ) ;
#21922 = CARTESIAN_POINT ( 'NONE',  ( 32.73300124599735739, -20.69176323058707823, 115.8010721414082980 ) ) ;
#21923 = CARTESIAN_POINT ( 'NONE',  ( -6.588769196390765970, 38.42957692275894033, 34.04709086065274448 ) ) ;
#21924 = B_SPLINE_CURVE_WITH_KNOTS ( 'NONE', 3,
 ( #127, #17810, #407, #2710, #9188, #17951, #15811, #26595 ),
 .UNSPECIFIED., .F., .F.,
 ( 4, 2, 2, 4 ),
 ( 6.938893903907228378E-18, 0.0002429588503611219996, 0.0004859177007222370602, 0.0009718354014444671816 ),
 .UNSPECIFIED. ) ;
#21925 = CARTESIAN_POINT ( 'NONE',  ( -8.786685647604890903, -48.22796981442753150, 23.24040270374441874 ) ) ;
#21926 = CARTESIAN_POINT ( 'NONE',  ( -1.049819825607599455, 27.33096219556293249, 36.75053263699358297 ) ) ;
#21927 = CARTESIAN_POINT ( 'NONE',  ( 55.49584447822657296, -7.317474139115140552, -72.18163437663947946 ) ) ;
#21928 = ORIENTED_EDGE ( 'NONE', *, *, #11402, .T. ) ;
#21929 = ORIENTED_EDGE ( 'NONE', *, *, #2387, .T. ) ;
#21931 = CARTESIAN_POINT ( 'NONE',  ( 9.884929003653626367, -150.0922431698404012, -11.54837932063185413 ) ) ;
#21930 = CARTESIAN_POINT ( 'NONE',  ( -8.786685647604885574, 6.096987947571466530E-17, -1.524246986892866633E-17 ) ) ;
#21932 = EDGE_CURVE ( 'NONE', #11599, #24182, #5251, .T. ) ;
#21933 = CARTESIAN_POINT ( 'NONE',  ( -1.031422197589716205, 43.06660437151310816, -15.60268798220652187 ) ) ;
#21934 = FACE_OUTER_BOUND ( 'NONE', #12728, .T. ) ;
#21935 = CARTESIAN_POINT ( 'NONE',  ( -1.155031165708882979, 35.88345263711048716, -28.62780465193323920 ) ) ;
#21936 =( BOUNDED_SURFACE ( )  B_SPLINE_SURFACE ( 3, 1, ( 
 ( #22483, #26490 ),
 ( #26772, #17987 ),
 ( #13244, #2745 ),
 ( #24354, #5042 ) ),
 .UNSPECIFIED., .F., .F., .F. ) 
 B_SPLINE_SURFACE_WITH_KNOTS ( ( 4, 4 ),
 ( 2, 2 ),
 ( 0.000000000000000000, 1.000000000000000000 ),
 ( 0.000000000000000000, 1.000000000000000000 ),
 .UNSPECIFIED. ) 
 GEOMETRIC_REPRESENTATION_ITEM ( )  RATIONAL_B_SPLINE_SURFACE ( (
 ( 1.000000000000000000, 1.000000000000000000),
 ( 0.7789835883360578528, 0.9689951854195403280),
 ( 0.7789835883360578528, 0.9689951854195403280),
 ( 1.000000000000000000, 1.000000000000000000) ) ) 
 REPRESENTATION_ITEM ( '' )  SURFACE ( )  );
#21937 = VERTEX_POINT ( 'NONE', #25126 ) ;
#21938 = CARTESIAN_POINT ( 'NONE',  ( -1.619063947482197729, -2.489035965909835557, 46.30105812165550816 ) ) ;
#21940 = EDGE_CURVE ( 'NONE', #1343, #15699, #20793, .T. ) ;
#21939 = CARTESIAN_POINT ( 'NONE',  ( 13.84597867724965248, 101.6650905919627803, -105.7628030201710487 ) ) ;
#21941 = CARTESIAN_POINT ( 'NONE',  ( -1.050230346682680782, -26.91946103437133431, -37.05264119692680680 ) ) ;
#21942 = ORIENTED_EDGE ( 'NONE', *, *, #27552, .T. ) ;
#21943 = VERTEX_POINT ( 'NONE', #5539 ) ;
#21944 = ADVANCED_FACE ( 'NONE', ( #7577 ), #12715, .F. ) ;
#21945 = PLANE ( 'NONE',  #9860 ) ;
#21946 = EDGE_LOOP ( 'NONE', ( #12869, #18967, #25067, #9320 ) ) ;
#21947 = CARTESIAN_POINT ( 'NONE',  ( 26.11404676487257603, 107.3263591096430218, 36.06104232266487486 ) ) ;
#21948 = ORIENTED_EDGE ( 'NONE', *, *, #17732, .F. ) ;
#21949 = CARTESIAN_POINT ( 'NONE',  ( 26.11404676487257603, 1.130420376097130086, 113.2169081140374090 ) ) ;
#21950 = ORIENTED_EDGE ( 'NONE', *, *, #12234, .F. ) ;
#21951 = EDGE_CURVE ( 'NONE', #5719, #3608, #14278, .T. ) ;
#21952 = CARTESIAN_POINT ( 'NONE',  ( -20.57838717382308147, -27.96569011373078339, 10.78122205917029675 ) ) ;
#21953 = CARTESIAN_POINT ( 'NONE',  ( -20.47566262905010603, 27.87687924095562408, 10.72601569609867944 ) ) ;
#21954 = CARTESIAN_POINT ( 'NONE',  ( 25.64681081121880624, 103.3177883989785499, -45.54494737132120008 ) ) ;
#21955 = CARTESIAN_POINT ( 'NONE',  ( 109.1592201516379674, 0.007845213074654433863, -0.0005146241775983094154 ) ) ;
#21956 = CARTESIAN_POINT ( 'NONE',  ( 16.75465622695656265, -4.637075857202498597, 142.1502242093126256 ) ) ;
#21957 = ADVANCED_FACE ( 'NONE', ( #12165 ), #15653, .F. ) ;
#21958 = CARTESIAN_POINT ( 'NONE',  ( -55.24340739397742084, -0.008612749836246226184, 0.005344433640972935315 ) ) ;
#21959 = CARTESIAN_POINT ( 'NONE',  ( -1.539760825549689072, 46.22267384399381740, -2.469813586483248447 ) ) ;
#21960 = DIRECTION ( 'NONE',  ( 0.000000000000000000, 0.000000000000000000, 1.000000000000000000 ) ) ;
#21961 = ORIENTED_EDGE ( 'NONE', *, *, #5176, .F. ) ;
#21962 = CARTESIAN_POINT ( 'NONE',  ( 28.37603512858462196, -68.88140609180129559, -91.75440368549998027 ) ) ;
#21963 = CARTESIAN_POINT ( 'NONE',  ( -1.031422197589716205, 45.78027046666444733, 1.530725436377623927 ) ) ;
#21964 = EDGE_CURVE ( 'NONE', #1898, #10231, #12062, .T. ) ;
#21965 = CARTESIAN_POINT ( 'NONE',  ( 25.64660436782531505, -75.98230157781813432, -83.52001792470981911 ) ) ;
#21966 = CARTESIAN_POINT ( 'NONE',  ( 16.75465622695667278, 140.0080030360329602, -25.01894884133717056 ) ) ;
#21967 = CARTESIAN_POINT ( 'NONE',  ( -55.25719721206881729, 0.002847566758684554142, 0.01079965405819473083 ) ) ;
#21968 = EDGE_CURVE ( 'NONE', #3668, #546, #28344, .T. ) ;
#21969 = EDGE_LOOP ( 'NONE', ( #27388, #24251, #20405, #13521 ) ) ;
#21970 = CARTESIAN_POINT ( 'NONE',  ( 1.833485406944057594, -44.33323125130021225, 138.1714136985306993 ) ) ;
#21971 =( BOUNDED_SURFACE ( )  B_SPLINE_SURFACE ( 3, 1, ( 
 ( #12629, #28299 ),
 ( #10903, #6040 ),
 ( #14928, #17362 ),
 ( #10489, #21278 ) ),
 .UNSPECIFIED., .F., .F., .F. ) 
 B_SPLINE_SURFACE_WITH_KNOTS ( ( 4, 4 ),
 ( 2, 2 ),
 ( 0.000000000000000000, 1.000000000000000000 ),
 ( 0.000000000000000000, 1.000000000000000000 ),
 .UNSPECIFIED. ) 
 GEOMETRIC_REPRESENTATION_ITEM ( )  RATIONAL_B_SPLINE_SURFACE ( (
 ( 1.000000000000000000, 1.000000000000000000),
 ( 0.7789835883360578528, 0.9689951854195403280),
 ( 0.7789835883360578528, 0.9689951854195403280),
 ( 1.000000000000000000, 1.000000000000000000) ) ) 
 REPRESENTATION_ITEM ( '' )  SURFACE ( )  );
#21972 = CARTESIAN_POINT ( 'NONE',  ( 109.1586900883932856, -0.006231977675085013588, -0.003481399864218412150 ) ) ;
#21973 = CARTESIAN_POINT ( 'NONE',  ( -55.24390624410018802, 0.007245494385991918876, 0.007503127514281743120 ) ) ;
#21974 = B_SPLINE_CURVE_WITH_KNOTS ( 'NONE', 3,
 ( #7557, #23249, #22818, #25252, #16609, #3083 ),
 .UNSPECIFIED., .F., .F.,
 ( 4, 2, 4 ),
 ( 1.041737195591640451E-17, 0.0006311571484586031870, 0.001262314296917195749 ),
 .UNSPECIFIED. ) ;
#21975 = CARTESIAN_POINT ( 'NONE',  ( 25.64700659047696618, 75.72132282458984776, -83.75695331063654692 ) ) ;
#21976 = VERTEX_POINT ( 'NONE', #10687 ) ;
#21977 = CARTESIAN_POINT ( 'NONE',  ( -7.078251931573400491, 26.33626633876288636, 44.92740138729136135 ) ) ;
#21978 = CARTESIAN_POINT ( 'NONE',  ( 13.36082413113061307, -97.52406103376675617, -117.7941133658648596 ) ) ;
#21979 = VERTEX_POINT ( 'NONE', #17286 ) ;
#21980 = CARTESIAN_POINT ( 'NONE',  ( 25.64704443564076897, -112.9111375659905718, -0.1334765861215692628 ) ) ;
#21981 = DIRECTION ( 'NONE',  ( -0.7563875759206388771, -0.03500244528123461207, -0.6531865459554673237 ) ) ;
#21982 = ORIENTED_EDGE ( 'NONE', *, *, #7535, .T. ) ;
#21983 = CARTESIAN_POINT ( 'NONE',  ( 25.64704443564079028, 103.2037466592380781, -45.80316013050731527 ) ) ;
#21984 = LINE ( 'NONE', #21428, #17024 ) ;
#21985 = DIRECTION ( 'NONE',  ( 1.000000000000000000, -6.938893903907226837E-18, 1.734723475976806709E-18 ) ) ;
#21986 = DIRECTION ( 'NONE',  ( 0.5946245182733607137, 0.5401723099040918186, -0.5955128528260758003 ) ) ;
#21987 = CARTESIAN_POINT ( 'NONE',  ( 10.93730112725990367, -108.9902118373734652, -104.7670965581022671 ) ) ;
#21988 = CARTESIAN_POINT ( 'NONE',  ( -1.050230347699842692, 1.897926697972695375E-16, 45.79907861674080749 ) ) ;
#21989 = CARTESIAN_POINT ( 'NONE',  ( 109.1778270068192853, -0.009293669915253103403, 0.0006237116683805770051 ) ) ;
#21990 = VECTOR ( 'NONE', #14434, 1000.000000000000000 ) ;
#21991 = ADVANCED_FACE ( 'NONE', ( #24499 ), #27258, .F. ) ;
#21992 = CARTESIAN_POINT ( 'NONE',  ( 26.11404676487257603, 67.46175819463486789, -90.92995828888132337 ) ) ;
#21993 = LINE ( 'NONE', #24307, #27225 ) ;
#21994 = DIRECTION ( 'NONE',  ( 0.5946245182733606027, -0.08110646981859072346, -0.7999021332774026716 ) ) ;
#21995 = ORIENTED_EDGE ( 'NONE', *, *, #20987, .F. ) ;
#21996 = EDGE_CURVE ( 'NONE', #27786, #709, #22183, .T. ) ;
#21997 = ORIENTED_EDGE ( 'NONE', *, *, #9044, .F. ) ;
#21998 = VERTEX_POINT ( 'NONE', #17845 ) ;
#21999 = CARTESIAN_POINT ( 'NONE',  ( -1.049819825607588575, -27.33096219556267670, -36.75053263699379613 ) ) ;
#22000 = CARTESIAN_POINT ( 'NONE',  ( -20.20700224038492721, -28.44216453106531617, 8.199606986804630182 ) ) ;
#22001 = CARTESIAN_POINT ( 'NONE',  ( -5.986830583229481917, 38.20088153919500229, -33.39046620690925238 ) ) ;
#22002 = CARTESIAN_POINT ( 'NONE',  ( 1.833206310202333045, -97.64934828277021950, -107.3376456496891223 ) ) ;
#22003 = CARTESIAN_POINT ( 'NONE',  ( 1.833838850855475489, 72.63194208529650098, -125.6242502389378899 ) ) ;
#22004 = CARTESIAN_POINT ( 'NONE',  ( 2.433796855181205476, -43.58222566461547132, -138.8296532063092457 ) ) ;
#22005 = ORIENTED_EDGE ( 'NONE', *, *, #23139, .T. ) ;
#22006 = DIRECTION ( 'NONE',  ( 0.000000000000000000, 0.000000000000000000, 1.000000000000000000 ) ) ;
#22007 = CARTESIAN_POINT ( 'NONE',  ( 32.73300124599734318, 92.86301839380026024, 72.21147546950587071 ) ) ;
#22008 = CARTESIAN_POINT ( 'NONE',  ( 9.884929003653608603, -42.50195158090934200, -144.4113244745776115 ) ) ;
#22009 = CARTESIAN_POINT ( 'NONE',  ( 109.1592201516379674, -0.001331853079201447297, 0.007748443302134876837 ) ) ;
#22010 = CARTESIAN_POINT ( 'NONE',  ( 16.75465622695655199, 136.6258322711655637, -39.51671382433799096 ) ) ;
#22011 = CARTESIAN_POINT ( 'NONE',  ( 6.224689322667647851, 145.3353551538641000, 28.26953958630669916 ) ) ;
#22012 = CARTESIAN_POINT ( 'NONE',  ( 1.833838848569445013, -107.7184832843401949, 97.22964245509723469 ) ) ;
#22013 = CARTESIAN_POINT ( 'NONE',  ( -55.24271866751342941, 0.006757859501006707216, 0.006671293903669109175 ) ) ;
#22014 = ORIENTED_EDGE ( 'NONE', *, *, #513, .T. ) ;
#22015 = CONICAL_SURFACE ( 'NONE', #22567, 117.6351876552689504, 0.9945805576725580410 ) ;
#22016 = B_SPLINE_CURVE_WITH_KNOTS ( 'NONE', 3,
 ( #11167, #17632, #7277, #24270, #503, #11586 ),
 .UNSPECIFIED., .F., .F.,
 ( 4, 2, 4 ),
 ( 7.757919228897728493E-18, 0.0004335184443140311294, 0.0008670368886280545610 ),
 .UNSPECIFIED. ) ;
#22017 = ORIENTED_EDGE ( 'NONE', *, *, #23794, .F. ) ;
#22018 = B_SPLINE_CURVE_WITH_KNOTS ( 'NONE', 3,
 ( #13788, #3012, #27891, #19387 ),
 .UNSPECIFIED., .F., .F.,
 ( 4, 4 ),
 ( 9.813077866773594792E-18, 0.008383560773332722482 ),
 .UNSPECIFIED. ) ;
#22019 = ORIENTED_EDGE ( 'NONE', *, *, #23139, .F. ) ;
#22020 = CARTESIAN_POINT ( 'NONE',  ( 21.16825799904908223, -37.62905626541790127, 130.1008673867301866 ) ) ;
#22021 = CARTESIAN_POINT ( 'NONE',  ( 109.1592201516379674, -0.007856029051018016685, -0.0003082430541935813001 ) ) ;
#22022 = CARTESIAN_POINT ( 'NONE',  ( 109.1592201516379674, -0.007620268632971095163, 0.001934867487021801630 ) ) ;
#22023 = EDGE_CURVE ( 'NONE', #18831, #14195, #26752, .T. ) ;
#22024 = VERTEX_POINT ( 'NONE', #13243 ) ;
#22025 = CARTESIAN_POINT ( 'NONE',  ( -7.733045908741324581, 35.49239760110675945, -38.67583825854160295 ) ) ;
#22026 = CARTESIAN_POINT ( 'NONE',  ( -1.058197053496160667, -12.47644286888545828, -44.07533330186785037 ) ) ;
#22027 = VERTEX_POINT ( 'NONE', #8802 ) ;
#22028 = EDGE_CURVE ( 'NONE', #21575, #546, #19872, .T. ) ;
#22029 = CARTESIAN_POINT ( 'NONE',  ( 55.79472521941428198, 8.328398066091761365, 72.27573336313956531 ) ) ;
#22030 = ORIENTED_EDGE ( 'NONE', *, *, #3193, .T. ) ;
#22031 = CARTESIAN_POINT ( 'NONE',  ( 32.73300124599732186, 0.000000000000000000, 0.000000000000000000 ) ) ;
#22032 = CARTESIAN_POINT ( 'NONE',  ( -1.464342487929843006, -11.94843286121887438, 44.64187261869788870 ) ) ;
#22033 = CARTESIAN_POINT ( 'NONE',  ( 1.832998868059858122, -45.34898734665954123, -137.8420662456174739 ) ) ;
#22034 = EDGE_CURVE ( 'NONE', #18167, #9317, #4348, .T. ) ;
#22035 = DIRECTION ( 'NONE',  ( -1.000000000000000000, 6.938893903907226837E-18, -1.734723475976806709E-18 ) ) ;
#22036 = CARTESIAN_POINT ( 'NONE',  ( -55.25719721206881729, -0.002847566758682281655, 0.01079965405819869988 ) ) ;
#22037 = CARTESIAN_POINT ( 'NONE',  ( 30.59138290137918759, 113.0806461017758267, -26.79783179610908661 ) ) ;
#22038 = CARTESIAN_POINT ( 'NONE',  ( 24.22246935314087324, 0.000000000000000000, 0.000000000000000000 ) ) ;
#22039 = DIRECTION ( 'NONE',  ( -0.7637818620346800147, -0.2198041754873968356, -0.6068965246771005351 ) ) ;
#22040 = CARTESIAN_POINT ( 'NONE',  ( 2.263178607246671969, 141.9207363487298323, -31.59906277834084065 ) ) ;
#22041 = EDGE_LOOP ( 'NONE', ( #3660, #25490, #23651, #4349 ) ) ;
#22042 = ORIENTED_EDGE ( 'NONE', *, *, #19599, .T. ) ;
#22043 = CARTESIAN_POINT ( 'NONE',  ( 26.11404676487259024, -55.62948129436313849, 98.61392875273344316 ) ) ;
#22044 = B_SPLINE_CURVE_WITH_KNOTS ( 'NONE', 3,
 ( #24163, #10637, #23759, #8611, #4560, #6743, #23892, #28177 ),
 .UNSPECIFIED., .F., .F.,
 ( 4, 2, 2, 4 ),
 ( 6.938893903907228378E-18, 0.0002429592666046868975, 0.0004859185332093668560, 0.0009718370664186821040 ),
 .UNSPECIFIED. ) ;
#22045 = VERTEX_POINT ( 'NONE', #15114 ) ;
#22046 = ORIENTED_EDGE ( 'NONE', *, *, #1113, .T. ) ;
#22047 = ORIENTED_EDGE ( 'NONE', *, *, #8425, .T. ) ;
#22048 = ADVANCED_FACE ( 'NONE', ( #19726 ), #9626, .F. ) ;
#22049 = B_SPLINE_CURVE_WITH_KNOTS ( 'NONE', 3,
 ( #23221, #24701, #4948, #20892, #20197, #9973, #11571 ),
 .UNSPECIFIED., .F., .F.,
 ( 4, 3, 4 ),
 ( 1.114146325429624918E-17, 0.009512539173626377575, 0.02506242213020845946 ),
 .UNSPECIFIED. ) ;
#22050 = EDGE_CURVE ( 'NONE', #12735, #2493, #18049, .T. ) ;
#22051 = CARTESIAN_POINT ( 'NONE',  ( 28.37603512858455801, -100.2461737936626633, -55.80522682147376656 ) ) ;
#22052 = CARTESIAN_POINT ( 'NONE',  ( 25.65782528836480836, -107.2118488517898669, -35.44279022896596842 ) ) ;
#22053 = CARTESIAN_POINT ( 'NONE',  ( -55.24300891470648622, -0.009225237711097735230, -0.003362556190414862749 ) ) ;
#22054 = VECTOR ( 'NONE', #4186, 1000.000000000000114 ) ;
#22055 = EDGE_CURVE ( 'NONE', #25403, #6415, #22937, .T. ) ;
#22056 = CARTESIAN_POINT ( 'NONE',  ( -55.25719721206881729, 0.009391134844729439810, -0.006045473558784624467 ) ) ;
#22057 = CARTESIAN_POINT ( 'NONE',  ( -1.050230347699842692, 1.897926697972695375E-16, 45.79907861674080749 ) ) ;
#22058 = DIRECTION ( 'NONE',  ( 0.5914120900931444380, 0.6045864222316746917, -0.5335794202785202334 ) ) ;
#22059 = CARTESIAN_POINT ( 'NONE',  ( -1.045287976400351981, 12.68782741917293855, -44.00138577190654132 ) ) ;
#22060 = CARTESIAN_POINT ( 'NONE',  ( 109.1624594426973118, 0.01154818537151455250, -0.01102230012606814254 ) ) ;
#22061 = CARTESIAN_POINT ( 'NONE',  ( -12.94347594948494340, 6.555928820869281637, -48.30328466416744249 ) ) ;
#22062 = CARTESIAN_POINT ( 'NONE',  ( 2.433796855181233454, -107.1581411821792216, 98.43889364293823974 ) ) ;
#22063 = ORIENTED_EDGE ( 'NONE', *, *, #20434, .F. ) ;
#22064 = AXIS2_PLACEMENT_3D ( 'NONE', #26494, #13390, #24505 ) ;
#22065 = EDGE_LOOP ( 'NONE', ( #18986, #25465, #24888, #24258, #13924, #27680 ) ) ;
#22067 = CARTESIAN_POINT ( 'NONE',  ( -55.24390624410018802, -0.001451500391952595045, 0.01032895241566660592 ) ) ;
#22066 = CARTESIAN_POINT ( 'NONE',  ( 109.1589550718175161, -0.002874971999837467197, 0.007008495014555471414 ) ) ;
#22068 = VECTOR ( 'NONE', #8446, 999.9999999999998863 ) ;
#22069 = CARTESIAN_POINT ( 'NONE',  ( 1.833485406944057594, -144.3694338680884073, -14.63699153649508311 ) ) ;
#22070 = FACE_OUTER_BOUND ( 'NONE', #937, .T. ) ;
#22071 = CARTESIAN_POINT ( 'NONE',  ( 6.224689322667630975, 33.28770499679534112, -144.2687111683192143 ) ) ;
#22072 = CARTESIAN_POINT ( 'NONE',  ( 16.05277956358202829, -134.7758735858406851, 48.70400867629053465 ) ) ;
#22073 = ORIENTED_EDGE ( 'NONE', *, *, #28034, .T. ) ;
#22074 = FACE_OUTER_BOUND ( 'NONE', #13818, .T. ) ;
#22075 = ORIENTED_EDGE ( 'NONE', *, *, #27825, .T. ) ;
#22076 = CARTESIAN_POINT ( 'NONE',  ( 2.108985857320914370, -84.36123201973892094, 118.2933707022555865 ) ) ;
#22077 = CARTESIAN_POINT ( 'NONE',  ( 21.16825799904897920, -93.85612807858952067, -97.63815233965159734 ) ) ;
#22078 = ORIENTED_EDGE ( 'NONE', *, *, #2237, .T. ) ;
#22079 = VERTEX_POINT ( 'NONE', #11102 ) ;
#22080 = B_SPLINE_CURVE_WITH_KNOTS ( 'NONE', 3,
 ( #3284, #10055, #9771, #12205, #25168, #23438, #5741 ),
 .UNSPECIFIED., .F., .F.,
 ( 4, 3, 4 ),
 ( 0.000000000000000000, 0.02398743853561303638, 0.04000277880656216700 ),
 .UNSPECIFIED. ) ;
#22081 = CARTESIAN_POINT ( 'NONE',  ( 1.834118845439484335, -0.1779704863080166510, 145.1099497418795750 ) ) ;
#22082 = ORIENTED_EDGE ( 'NONE', *, *, #18893, .F. ) ;
#22083 = FACE_OUTER_BOUND ( 'NONE', #17020, .T. ) ;
#22084 = ORIENTED_EDGE ( 'NONE', *, *, #24067, .T. ) ;
#22085 = CARTESIAN_POINT ( 'NONE',  ( -55.24340739397742084, -0.009386184976286139278, -0.003826481709803953961 ) ) ;
#22086 = CARTESIAN_POINT ( 'NONE',  ( -20.57838717382308147, -27.96569011373078339, 10.78122205917029675 ) ) ;
#22087 = EDGE_LOOP ( 'NONE', ( #20395, #24191, #15141, #11652 ) ) ;
#22088 = CIRCLE ( 'NONE', #15166, 117.6351876552689504 ) ;
#22089 = CARTESIAN_POINT ( 'NONE',  ( 109.1721716018069515, -0.01157047143378747006, 0.01254847260354031470 ) ) ;
#22090 = EDGE_CURVE ( 'NONE', #9341, #1180, #8953, .T. ) ;
#22091 = AXIS2_PLACEMENT_3D ( 'NONE', #14015, #11868, #13730 ) ;
#22092 = CARTESIAN_POINT ( 'NONE',  ( 28.37603512858450472, 78.09501335733588689, 84.05169593519752880 ) ) ;
#22093 = CARTESIAN_POINT ( 'NONE',  ( -55.24300891470650754, 0.009225237711101738972, -0.003362556190412665288 ) ) ;
#22094 = CARTESIAN_POINT ( 'NONE',  ( 109.1624594426973118, -0.01318243916935001731, -0.009004164758064509000 ) ) ;
#22095 = EDGE_CURVE ( 'NONE', #14412, #22982, #18423, .T. ) ;
#22096 = DIRECTION ( 'NONE',  ( 1.000000000000000000, 0.000000000000000000, 0.000000000000000000 ) ) ;
#22097 = CARTESIAN_POINT ( 'NONE',  ( 10.93730112725945602, 84.82621002473440797, 125.1380233598478640 ) ) ;
#22098 = EDGE_CURVE ( 'NONE', #4882, #15045, #8496, .T. ) ;
#22099 = B_SPLINE_CURVE_WITH_KNOTS ( 'NONE', 3,
 ( #12028, #7285, #7727, #13889, #7429, #16483, #25274, #18498, #23130, #11880 ),
 .UNSPECIFIED., .F., .F.,
 ( 4, 3, 3, 4 ),
 ( 3.925231146709437917E-17, 0.0002669559177086244599, 0.0005339118354150962364, 0.001067817517169172706 ),
 .UNSPECIFIED. ) ;
#22100 =( BOUNDED_SURFACE ( )  B_SPLINE_SURFACE ( 3, 1, ( 
 ( #19283, #126 ),
 ( #19560, #13211 ),
 ( #28330, #17678 ),
 ( #26457, #4160 ) ),
 .UNSPECIFIED., .F., .F., .F. ) 
 B_SPLINE_SURFACE_WITH_KNOTS ( ( 4, 4 ),
 ( 2, 2 ),
 ( 0.000000000000000000, 1.000000000000000000 ),
 ( 0.000000000000000000, 1.000000000000000000 ),
 .UNSPECIFIED. ) 
 GEOMETRIC_REPRESENTATION_ITEM ( )  RATIONAL_B_SPLINE_SURFACE ( (
 ( 1.000000000000000000, 1.000000000000000000),
 ( 0.9956975270656954757, 0.8568959468854893125),
 ( 0.9956975270656954757, 0.8568959468854893125),
 ( 1.000000000000000000, 1.000000000000000000) ) ) 
 REPRESENTATION_ITEM ( '' )  SURFACE ( )  );
#22101 = DIRECTION ( 'NONE',  ( 0.000000000000000000, 0.000000000000000000, 1.000000000000000000 ) ) ;
#22102 = CARTESIAN_POINT ( 'NONE',  ( 9.884929003653626367, -27.17402761732445526, 148.0628878137279685 ) ) ;
#22103 = DIRECTION ( 'NONE',  ( 0.000000000000000000, 0.000000000000000000, 1.000000000000000000 ) ) ;
#22104 = EDGE_LOOP ( 'NONE', ( #12314, #4301, #9265, #13106 ) ) ;
#22105 = CARTESIAN_POINT ( 'NONE',  ( 25.64660436782543940, 83.52001792470993280, -75.98230157781777905 ) ) ;
#22106 = CARTESIAN_POINT ( 'NONE',  ( 14.74894986621300141, -1.023413983156987271E-16, 2.558534957892468177E-17 ) ) ;
#22107 = CARTESIAN_POINT ( 'NONE',  ( 10.93730112726006176, 146.7718404940648611, -36.23586118136403655 ) ) ;
#22108 = B_SPLINE_CURVE_WITH_KNOTS ( 'NONE', 3,
 ( #6128, #5540, #20932, #3946 ),
 .UNSPECIFIED., .F., .F.,
 ( 4, 4 ),
 ( 0.000000000000000000, 0.01077107196513860457 ),
 .UNSPECIFIED. ) ;
#22109 = CARTESIAN_POINT ( 'NONE',  ( -21.41430102051744555, 1.815007301162403497, 30.75470819672109002 ) ) ;
#22110 = CARTESIAN_POINT ( 'NONE',  ( 1.833485406944043827, 84.86072343962567288, 117.7091014914953320 ) ) ;
#22111 = CARTESIAN_POINT ( 'NONE',  ( 55.49584447822657296, 22.67407039687241621, 68.91748907713598271 ) ) ;
#22112 = VERTEX_POINT ( 'NONE', #15647 ) ;
#22113 = CARTESIAN_POINT ( 'NONE',  ( -12.82751273423884442, 6.573887447703498310, 48.43568301531131937 ) ) ;
#22114 = CIRCLE ( 'NONE', #23957, 53.53553390275978785 ) ;
#22115 = B_SPLINE_CURVE_WITH_KNOTS ( 'NONE', 3,
 ( #25652, #28065, #10666, #5931 ),
 .UNSPECIFIED., .F., .F.,
 ( 4, 4 ),
 ( 3.469446951953614189E-18, 0.008383560773332696461 ),
 .UNSPECIFIED. ) ;
#22116 = CARTESIAN_POINT ( 'NONE',  ( 26.11404676487259024, 113.2169081140373947, -1.130420376097525326 ) ) ;
#22117 = DIRECTION ( 'NONE',  ( 0.000000000000000000, 0.000000000000000000, 1.000000000000000000 ) ) ;
#22118 = CIRCLE ( 'NONE', #8789, 151.1787379149930359 ) ;
#22119 = ORIENTED_EDGE ( 'NONE', *, *, #14695, .F. ) ;
#22120 = CARTESIAN_POINT ( 'NONE',  ( -55.24728320129491266, -0.01214321324517104832, 0.008013189884951824049 ) ) ;
#22121 = CIRCLE ( 'NONE', #25813, 37.50000000000001421 ) ;
#22122 = DIRECTION ( 'NONE',  ( 0.000000000000000000, -1.000000000000000000, -3.122502256758243698E-15 ) ) ;
#22123 = DIRECTION ( 'NONE',  ( -1.000000000000000000, 6.938893903907226837E-18, -1.734723475976806709E-18 ) ) ;
#22124 = VERTEX_POINT ( 'NONE', #11787 ) ;
#22125 = CARTESIAN_POINT ( 'NONE',  ( -1.583189561560253589, -11.94859433442870866, 44.83405390829683057 ) ) ;
#22126 = CARTESIAN_POINT ( 'NONE',  ( -20.57838717382308147, -25.16001208503117326, -16.28767523336112433 ) ) ;
#22127 = DIRECTION ( 'NONE',  ( -1.000000000000000000, -0.000000000000000000, -0.000000000000000000 ) ) ;
#22128 = EDGE_CURVE ( 'NONE', #6453, #15531, #3798, .T. ) ;
#22129 = ORIENTED_EDGE ( 'NONE', *, *, #1971, .T. ) ;
#22130 = CARTESIAN_POINT ( 'NONE',  ( -1.583189561560252701, 46.33203782964461936, 2.490696082060036343 ) ) ;
#22131 = EDGE_CURVE ( 'NONE', #10550, #9180, #9349, .T. ) ;
#22132 = CARTESIAN_POINT ( 'NONE',  ( -1.155031165708893415, -45.85732438018708024, 2.068616213631418344 ) ) ;
#22133 = CARTESIAN_POINT ( 'NONE',  ( 109.1721716018069515, 0.008708654716135744156, -0.01467989464938425186 ) ) ;
#22134 = CARTESIAN_POINT ( 'NONE',  ( 13.84597867724970577, -105.7628030201713045, -101.6650905919622829 ) ) ;
#22135 = CARTESIAN_POINT ( 'NONE',  ( 25.64703792032470631, 110.4746717456749252, 23.32999623362163177 ) ) ;
#22136 = VECTOR ( 'NONE', #12913, 1000.000000000000114 ) ;
#22137 = ORIENTED_EDGE ( 'NONE', *, *, #1565, .F. ) ;
#22138 = DIRECTION ( 'NONE',  ( 0.5946245182733607137, -0.7992853357633872280, -0.08697490616139179342 ) ) ;
#22139 = CARTESIAN_POINT ( 'NONE',  ( 109.1721716018069515, 0.003746085893651815869, -0.01665253177025272785 ) ) ;
#22140 = CARTESIAN_POINT ( 'NONE',  ( -20.20997486282891131, 0.3303743256174362375, -29.60348406988234871 ) ) ;
#22141 = CARTESIAN_POINT ( 'NONE',  ( -6.574463467970653063, 20.55340846381200848, 47.03022655117382556 ) ) ;
#22142 = EDGE_LOOP ( 'NONE', ( #2525, #22964, #19976, #4035 ) ) ;
#22144 = AXIS2_PLACEMENT_3D ( 'NONE', #21828, #4539, #2224 ) ;
#22143 =( BOUNDED_SURFACE ( )  B_SPLINE_SURFACE ( 3, 1, ( 
 ( #3563, #12758 ),
 ( #16950, #6030 ),
 ( #14786, #17085 ),
 ( #14922, #23741 ) ),
 .UNSPECIFIED., .F., .F., .F. ) 
 B_SPLINE_SURFACE_WITH_KNOTS ( ( 4, 4 ),
 ( 2, 2 ),
 ( 0.000000000000000000, 1.000000000000000000 ),
 ( 0.000000000000000000, 1.000000000000000000 ),
 .UNSPECIFIED. ) 
 GEOMETRIC_REPRESENTATION_ITEM ( )  RATIONAL_B_SPLINE_SURFACE ( (
 ( 1.000000000000000000, 1.000000000000000000),
 ( 0.9960225298536222738, 0.9999952330161893110),
 ( 0.9960225298536222738, 0.9999952330161893110),
 ( 1.000000000000000000, 1.000000000000000000) ) ) 
 REPRESENTATION_ITEM ( '' )  SURFACE ( )  );
#22145 = ORIENTED_EDGE ( 'NONE', *, *, #11313, .T. ) ;
#22146 = ORIENTED_EDGE ( 'NONE', *, *, #21027, .F. ) ;
#22147 = CARTESIAN_POINT ( 'NONE',  ( 2.108393763691155609, -43.67806918959044538, -138.5721856399489695 ) ) ;
#22148 = CARTESIAN_POINT ( 'NONE',  ( -25.21435515916043002, -4.655591116594591128, -34.29329011225954105 ) ) ;
#22149 = DIRECTION ( 'NONE',  ( -0.5946245182733608248, 0.3297108033645218539, 0.7332888028688936410 ) ) ;
#22150 = FACE_OUTER_BOUND ( 'NONE', #21170, .T. ) ;
#22151 = CARTESIAN_POINT ( 'NONE',  ( 25.64703792032471341, -91.43447020678384263, -66.24710921678151010 ) ) ;
#22152 = ORIENTED_EDGE ( 'NONE', *, *, #6808, .F. ) ;
#22153 = CARTESIAN_POINT ( 'NONE',  ( 25.98107933586708995, -33.92073193606511694, -107.9289867379275307 ) ) ;
#22154 = FACE_OUTER_BOUND ( 'NONE', #3729, .T. ) ;
#22155 = LINE ( 'NONE', #7331, #16597 ) ;
#22156 = CARTESIAN_POINT ( 'NONE',  ( -21.41430102051752016, 11.22990201072317262, 28.68859753627381792 ) ) ;
#22157 = CARTESIAN_POINT ( 'NONE',  ( 2.433796855181233454, 142.6247129145648387, 28.83182736670586266 ) ) ;
#22158 = EDGE_LOOP ( 'NONE', ( #4303, #3132, #21002, #23066 ) ) ;
#22159 = CARTESIAN_POINT ( 'NONE',  ( 26.11404676487257603, 83.38016054979783576, 76.59696442953219275 ) ) ;
#22160 = B_SPLINE_CURVE_WITH_KNOTS ( 'NONE', 3,
 ( #7325, #16088, #8183, #5440 ),
 .UNSPECIFIED., .F., .F.,
 ( 4, 4 ),
 ( 2.226941760980096400E-16, 0.008383748772659700005 ),
 .UNSPECIFIED. ) ;
#22161 = CARTESIAN_POINT ( 'NONE',  ( 1.833838848569417923, -117.5008734796305845, -85.14939661881690824 ) ) ;
#22162 = ORIENTED_EDGE ( 'NONE', *, *, #24034, .T. ) ;
#22163 = VERTEX_POINT ( 'NONE', #22591 ) ;
#22164 = ADVANCED_FACE ( 'NONE', ( #20554 ), #4478, .F. ) ;
#22165 = ORIENTED_EDGE ( 'NONE', *, *, #15965, .T. ) ;
#22166 = CIRCLE ( 'NONE', #20782, 53.53553390275978785 ) ;
#22167 = EDGE_CURVE ( 'NONE', #15365, #8101, #9511, .T. ) ;
#22168 = EDGE_CURVE ( 'NONE', #26221, #14104, #15947, .T. ) ;
#22169 = CARTESIAN_POINT ( 'NONE',  ( 55.79472521941428198, -8.328398066091271090, -72.27573336313960795 ) ) ;
#22170 = CARTESIAN_POINT ( 'NONE',  ( -7.078251931573400491, -5.101176922830306104, 51.82710018979479116 ) ) ;
#22171 = CARTESIAN_POINT ( 'NONE',  ( -55.24271866751342941, -0.008488649505345847654, 0.004256484107793125603 ) ) ;
#22172 = B_SPLINE_CURVE_WITH_KNOTS ( 'NONE', 3,
 ( #3262, #11894, #22563, #18212, #13753, #5129, #7301, #955, #7447, #11608 ),
 .UNSPECIFIED., .F., .F.,
 ( 4, 2, 2, 2, 4 ),
 ( 3.104682540412587095E-18, 0.0003346267210630946812, 0.0006692534421261863266, 0.001003880163189277809, 0.001338506884252369401 ),
 .UNSPECIFIED. ) ;
#22173 = VERTEX_POINT ( 'NONE', #17950 ) ;
#22174 = CARTESIAN_POINT ( 'NONE',  ( -8.786685647604890903, -47.14957014837335691, 25.35688121747554291 ) ) ;
#22175 = CARTESIAN_POINT ( 'NONE',  ( -55.24728320129491266, -0.01137345571547045305, -0.009072670231978460439 ) ) ;
#22176 = ORIENTED_EDGE ( 'NONE', *, *, #5063, .T. ) ;
#22177 = CARTESIAN_POINT ( 'NONE',  ( -1.044556982611280382, -25.56989963842174873, 37.98985389331836870 ) ) ;
#22178 = ORIENTED_EDGE ( 'NONE', *, *, #16544, .F. ) ;
#22179 = CARTESIAN_POINT ( 'NONE',  ( -28.13707043255157103, 18.96624908365864925, 12.83104814250432923 ) ) ;
#22180 = CARTESIAN_POINT ( 'NONE',  ( 10.93730112725971715, 4.928439153520177030, 151.0983828010091372 ) ) ;
#22181 = CARTESIAN_POINT ( 'NONE',  ( 1.833485406944057594, -29.64752363041639782, 142.0485807715645024 ) ) ;
#22182 = CARTESIAN_POINT ( 'NONE',  ( -25.21435515916043357, -15.02493970636125198, 31.17620025257602379 ) ) ;
#22183 = LINE ( 'NONE', #24212, #22188 ) ;
#22184 = CARTESIAN_POINT ( 'NONE',  ( -25.21435515916025594, 34.29329011225976132, 4.655591116594488099 ) ) ;
#22185 = VECTOR ( 'NONE', #2925, 1000.000000000000000 ) ;
#22186 = CARTESIAN_POINT ( 'NONE',  ( -1.619063947482197729, -35.99532424477357750, 29.22875152547795707 ) ) ;
#22187 = DIRECTION ( 'NONE',  ( 0.000000000000000000, 0.000000000000000000, 1.000000000000000000 ) ) ;
#22188 = VECTOR ( 'NONE', #2158, 1000.000000000000114 ) ;
#22189 = DIRECTION ( 'NONE',  ( 1.000000000000000000, -0.000000000000000000, -0.000000000000000000 ) ) ;
#22190 = CARTESIAN_POINT ( 'NONE',  ( 1.894214914920973269, -43.94587946447497728, 138.3376769255506815 ) ) ;
#22191 =( BOUNDED_SURFACE ( )  B_SPLINE_SURFACE ( 3, 1, ( 
 ( #21037, #23235 ),
 ( #16884, #14853 ),
 ( #3624, #25384 ),
 ( #21333, #7983 ) ),
 .UNSPECIFIED., .F., .F., .F. ) 
 B_SPLINE_SURFACE_WITH_KNOTS ( ( 4, 4 ),
 ( 2, 2 ),
 ( 0.000000000000000000, 1.000000000000000000 ),
 ( 0.000000000000000000, 1.000000000000000000 ),
 .UNSPECIFIED. ) 
 GEOMETRIC_REPRESENTATION_ITEM ( )  RATIONAL_B_SPLINE_SURFACE ( (
 ( 1.000000000000000000, 1.000000000000000000),
 ( 0.6386103224230302855, 0.9954351624131538845),
 ( 0.6386103224230302855, 0.9954351624131538845),
 ( 1.000000000000000000, 1.000000000000000000) ) ) 
 REPRESENTATION_ITEM ( '' )  SURFACE ( )  );
#22192 = VERTEX_POINT ( 'NONE', #26736 ) ;
#22193 = ADVANCED_FACE ( 'NONE', ( #24755 ), #11459, .F. ) ;
#22194 = ORIENTED_EDGE ( 'NONE', *, *, #21027, .T. ) ;
#22195 = CARTESIAN_POINT ( 'NONE',  ( -1.045287976400351981, 43.05558670614237116, -15.59869763335110449 ) ) ;
#22196 = CARTESIAN_POINT ( 'NONE',  ( 26.11404676487259024, -92.25884714080363835, -65.63269960453335727 ) ) ;
#22197 = ORIENTED_EDGE ( 'NONE', *, *, #3578, .F. ) ;
#22198 = B_SPLINE_CURVE_WITH_KNOTS ( 'NONE', 3,
 ( #4256, #21959, #28283, #23864, #19789, #12885, #8307, #17074, #10755, #25865 ),
 .UNSPECIFIED., .F., .F.,
 ( 4, 2, 2, 2, 4 ),
 ( 1.371419323662773916E-18, 0.0003346267210630953859, 0.0006692534421261894708, 0.001003880163189283447, 0.001338506884252376773 ),
 .UNSPECIFIED. ) ;
#22199 = VERTEX_POINT ( 'NONE', #7768 ) ;
#22200 = EDGE_CURVE ( 'NONE', #6724, #23613, #11897, .T. ) ;
#22201 = VERTEX_POINT ( 'NONE', #3430 ) ;
#22202 = CARTESIAN_POINT ( 'NONE',  ( 26.11404676487259024, 83.38016054979885894, -76.59696442953111273 ) ) ;
#22203 = CARTESIAN_POINT ( 'NONE',  ( -20.47566338032518019, 29.82700953060488303, -1.586617869343990739 ) ) ;
#22204 = EDGE_CURVE ( 'NONE', #437, #21420, #9795, .T. ) ;
#22205 = CIRCLE ( 'NONE', #8893, 151.1787379149930359 ) ;
#22206 = B_SPLINE_CURVE_WITH_KNOTS ( 'NONE', 3,
 ( #22405, #2667, #20803, #16787 ),
 .UNSPECIFIED., .F., .F.,
 ( 4, 4 ),
 ( 2.400696848537691317E-16, 0.008383748772659717352 ),
 .UNSPECIFIED. ) ;
#22207 = VECTOR ( 'NONE', #15443, 1000.000000000000114 ) ;
#22208 = EDGE_LOOP ( 'NONE', ( #20225, #19440, #7166, #13177 ) ) ;
#22209 = CARTESIAN_POINT ( 'NONE',  ( 2.433796855181219243, -13.76554153471791864, 144.8571464219888583 ) ) ;
#22210 = CARTESIAN_POINT ( 'NONE',  ( -20.21097721650786738, 29.61001326827675939, -0.3305964462498667822 ) ) ;
#22211 = CARTESIAN_POINT ( 'NONE',  ( 32.73300124599735739, 28.19767303745605602, 114.2056417606549132 ) ) ;
#22212 = CARTESIAN_POINT ( 'NONE',  ( -12.82751273423881777, 43.04932478553568842, 23.15139349681263070 ) ) ;
#22213 = B_SPLINE_CURVE_WITH_KNOTS ( 'NONE', 3,
 ( #14541, #7805, #23346, #12659 ),
 .UNSPECIFIED., .F., .F.,
 ( 4, 4 ),
 ( 0.000000000000000000, 0.008383560773332698196 ),
 .UNSPECIFIED. ) ;
#22214 = B_SPLINE_CURVE_WITH_KNOTS ( 'NONE', 3,
 ( #25525, #3339, #27810, #23653, #25794, #18599, #12537, #3476 ),
 .UNSPECIFIED., .F., .F.,
 ( 4, 2, 2, 4 ),
 ( 0.000000000000000000, 0.0002429588503611251709, 0.0004859177007222503417, 0.0009718354014444904919 ),
 .UNSPECIFIED. ) ;
#22215 = CARTESIAN_POINT ( 'NONE',  ( -8.786685647604894456, 37.00619870957989832, 38.68584556812258768 ) ) ;
#22216 = CARTESIAN_POINT ( 'NONE',  ( 25.70243777736189728, 24.19989514742873737, -110.3252221127464026 ) ) ;
#22217 = B_SPLINE_CURVE_WITH_KNOTS ( 'NONE', 3,
 ( #3707, #2338, #11140, #19913 ),
 .UNSPECIFIED., .F., .F.,
 ( 4, 4 ),
 ( 0.0009910334943227156780, 0.001982023823822944616 ),
 .UNSPECIFIED. ) ;
#22218 = CARTESIAN_POINT ( 'NONE',  ( 2.433796855181205476, -133.5135467655521779, 57.85512797797844087 ) ) ;
#22219 = CARTESIAN_POINT ( 'NONE',  ( 109.1721716018069657, 0.006757465437538790615, -0.01567407524362082055 ) ) ;
#22220 = CARTESIAN_POINT ( 'NONE',  ( -55.24390624410018802, -0.01032895241566633357, -0.001451500391952961289 ) ) ;
#22221 = ORIENTED_EDGE ( 'NONE', *, *, #1905, .F. ) ;
#22223 = CARTESIAN_POINT ( 'NONE',  ( 109.1721716018069515, -0.003746085893651930360, 0.01665253177025270356 ) ) ;
#22222 = CARTESIAN_POINT ( 'NONE',  ( 25.64699802086724389, 91.48665801621663718, 66.17503410043930501 ) ) ;
#22224 = CARTESIAN_POINT ( 'NONE',  ( -1.155001620486273861, 35.88346938217592452, 28.62773628245626867 ) ) ;
#22225 = CARTESIAN_POINT ( 'NONE',  ( 25.64692232868534560, 46.22343382108737586, 103.0161468101948827 ) ) ;
#22226 = CARTESIAN_POINT ( 'NONE',  ( 2.433796855181205476, 57.85512797797890272, 133.5135467655520074 ) ) ;
#22227 = CARTESIAN_POINT ( 'NONE',  ( 2.433796855181205476, 144.8571464219891141, -13.76554153471544417 ) ) ;
#22228 = ORIENTED_EDGE ( 'NONE', *, *, #27147, .F. ) ;
#22229 = CARTESIAN_POINT ( 'NONE',  ( 25.64703792032469920, 97.70949518026583291, -56.58441811305505098 ) ) ;
#22230 = VECTOR ( 'NONE', #19562, 1000.000000000000114 ) ;
#22231 = EDGE_CURVE ( 'NONE', #17054, #20235, #22885, .T. ) ;
#22232 = ORIENTED_EDGE ( 'NONE', *, *, #20571, .T. ) ;
#22233 = CARTESIAN_POINT ( 'NONE',  ( 1.832998868059858122, 84.86110816369603072, 117.7096351258390854 ) ) ;
#22234 = B_SPLINE_CURVE_WITH_KNOTS ( 'NONE', 3,
 ( #5311, #5457, #18701, #9791, #16252, #14216, #1277, #24771, #20427, #18119 ),
 .UNSPECIFIED., .F., .F.,
 ( 4, 2, 2, 2, 4 ),
 ( 2.847672227753435151E-16, 0.0003346187017559034554, 0.0006692374035115221994, 0.001003856105267140727, 0.001338474807022759470 ),
 .UNSPECIFIED. ) ;
#22235 = CARTESIAN_POINT ( 'NONE',  ( 1.833485406944043827, 0.5339064996905048543, -145.1085452359073145 ) ) ;
#22236 = VERTEX_POINT ( 'NONE', #14202 ) ;
#22237 = VERTEX_POINT ( 'NONE', #10059 ) ;
#22238 = ADVANCED_FACE ( 'NONE', ( #6027 ), #1934, .T. ) ;
#22239 = CARTESIAN_POINT ( 'NONE',  ( -28.13707043255157103, 18.06394523322473944, 14.07296284901312688 ) ) ;
#22240 = VERTEX_POINT ( 'NONE', #25605 ) ;
#22241 = CARTESIAN_POINT ( 'NONE',  ( 1.831572820252008738, -96.36280042115856759, -108.4969585352564678 ) ) ;
#22242 = ORIENTED_EDGE ( 'NONE', *, *, #6775, .F. ) ;
#22243 = EDGE_CURVE ( 'NONE', #26223, #27903, #20846, .T. ) ;
#22244 = FACE_OUTER_BOUND ( 'NONE', #27096, .T. ) ;
#22245 = EDGE_CURVE ( 'NONE', #13623, #3154, #23442, .T. ) ;
#22246 = CIRCLE ( 'NONE', #9842, 151.1787379149930359 ) ;
#22247 = CARTESIAN_POINT ( 'NONE',  ( -1.049819825607596568, 37.34982882986881236, 26.50610175068227292 ) ) ;
#22248 = CARTESIAN_POINT ( 'NONE',  ( -55.24390624410018802, 0.01032895241567037548, -0.001451500391950801341 ) ) ;
#22249 = FACE_OUTER_BOUND ( 'NONE', #22697, .T. ) ;
#22250 = CARTESIAN_POINT ( 'NONE',  ( 1.834118845439484335, 137.9527673765111899, -45.01070051384449044 ) ) ;
#22251 = CARTESIAN_POINT ( 'NONE',  ( -23.77929240705206482, -31.93650644494352875, -17.17389748746951739 ) ) ;
#22252 = CARTESIAN_POINT ( 'NONE',  ( 109.1586059443104944, -0.004935564877224718136, -0.005067816690886739472 ) ) ;
#22253 = B_SPLINE_CURVE_WITH_KNOTS ( 'NONE', 3,
 ( #916, #18623, #11859, #19055, #14287, #23108, #18764, #1486, #3367, #5826, #12416, #23388, #27393 ),
 .UNSPECIFIED., .F., .F.,
 ( 4, 3, 3, 3, 4 ),
 ( 1.551583845779545699E-17, 0.0007657099931970509123, 0.001531419946797920456, 0.002296279302920149930, 0.003061450627205759834 ),
 .UNSPECIFIED. ) ;
#22254 = CARTESIAN_POINT ( 'NONE',  ( 26.11404676487257603, -110.5078194225159223, -24.64483677384961879 ) ) ;
#22255 = CARTESIAN_POINT ( 'NONE',  ( 32.73300124599740002, -81.52272205837138586, -84.80615050150450429 ) ) ;
#22256 = CARTESIAN_POINT ( 'NONE',  ( -1.031422197589711764, -12.69107518035532856, -44.01264471863841266 ) ) ;
#22257 = ORIENTED_EDGE ( 'NONE', *, *, #23686, .F. ) ;
#22258 = CARTESIAN_POINT ( 'NONE',  ( -55.24390624410018802, -0.007503127514277506058, -0.007245494385991484328 ) ) ;
#22260 = CARTESIAN_POINT ( 'NONE',  ( -1.619063947482197729, 16.67502769180622835, 43.26576862488415287 ) ) ;
#22259 = CARTESIAN_POINT ( 'NONE',  ( -21.41430102051745266, 30.75470819672112199, -1.815007301162081088 ) ) ;
#22261 = CARTESIAN_POINT ( 'NONE',  ( 16.05277956358201052, -137.6634701901228652, -39.81690014528805222 ) ) ;
#22262 = CARTESIAN_POINT ( 'NONE',  ( 109.1586900883932856, 0.003481399864218433400, -0.006231977675085001445 ) ) ;
#22263 = FACE_OUTER_BOUND ( 'NONE', #17881, .T. ) ;
#22264 = CARTESIAN_POINT ( 'NONE',  ( 25.64692872815575342, -34.58541472378575321, -107.4838747185724515 ) ) ;
#22265 = CARTESIAN_POINT ( 'NONE',  ( 32.73300124599732186, 0.000000000000000000, 0.000000000000000000 ) ) ;
#22266 = CARTESIAN_POINT ( 'NONE',  ( 25.64692872815578184, 110.5102270591925588, -23.16082795281147355 ) ) ;
#22267 = EDGE_CURVE ( 'NONE', #7492, #18707, #18352, .T. ) ;
#22268 = ORIENTED_EDGE ( 'NONE', *, *, #19157, .T. ) ;
#22269 = CARTESIAN_POINT ( 'NONE',  ( 109.1586900883932856, 0.006231977675082105324, -0.003481399864227396716 ) ) ;
#22270 = ADVANCED_FACE ( 'NONE', ( #1678 ), #1516, .T. ) ;
#22271 = SHAPE_REPRESENTATION ( 'pinion 3', ( #27263 ), #2919 ) ;
#22272 = CARTESIAN_POINT ( 'NONE',  ( 2.430230287190592531, -71.49654683843598946, 126.7388733285342823 ) ) ;
#22273 = CARTESIAN_POINT ( 'NONE',  ( 1.833485406944043827, -96.69979900902241354, 108.1939177044922786 ) ) ;
#22274 = B_SPLINE_CURVE_WITH_KNOTS ( 'NONE', 3,
 ( #24895, #5156, #13931, #22743, #14644, #2192, #1404, #19760, #23310, #21118 ),
 .UNSPECIFIED., .F., .F.,
 ( 4, 2, 2, 2, 4 ),
 ( 2.976713740813343128E-16, 0.0003346187017559147311, 0.0006692374035115318488, 0.001003856105267148966, 0.001338474807022765976 ),
 .UNSPECIFIED. ) ;
#22275 = ORIENTED_EDGE ( 'NONE', *, *, #26289, .T. ) ;
#22276 = CARTESIAN_POINT ( 'NONE',  ( 25.98552792386798771, 112.3992180166320480, -12.89843290883410987 ) ) ;
#22277 = ORIENTED_EDGE ( 'NONE', *, *, #23489, .F. ) ;
#22278 = CARTESIAN_POINT ( 'NONE',  ( 109.1721716018069657, 0.008358834333183932583, -0.01488186354166049288 ) ) ;
#22279 = ORIENTED_EDGE ( 'NONE', *, *, #10768, .T. ) ;
#22280 = SHAPE_REPRESENTATION_RELATIONSHIP ( 'NONE' , 'NONE' ,  #7571, #26090 ) ;
#22281 =( BOUNDED_SURFACE ( )  B_SPLINE_SURFACE ( 3, 1, ( 
 ( #28193, #6760 ),
 ( #15504, #24319 ),
 ( #4580, #8495 ),
 ( #11786, #2559 ) ),
 .UNSPECIFIED., .F., .F., .F. ) 
 B_SPLINE_SURFACE_WITH_KNOTS ( ( 4, 4 ),
 ( 2, 2 ),
 ( 0.000000000000000000, 1.000000000000000000 ),
 ( 0.000000000000000000, 1.000000000000000000 ),
 .UNSPECIFIED. ) 
 GEOMETRIC_REPRESENTATION_ITEM ( )  RATIONAL_B_SPLINE_SURFACE ( (
 ( 1.000000000000000000, 1.000000000000000000),
 ( 0.9956975270656954757, 0.8568959468854893125),
 ( 0.9956975270656954757, 0.8568959468854893125),
 ( 1.000000000000000000, 1.000000000000000000) ) ) 
 REPRESENTATION_ITEM ( '' )  SURFACE ( )  );
#22282 = CARTESIAN_POINT ( 'NONE',  ( -20.20700224038492721, 28.44216453106536946, -8.199606986804427677 ) ) ;
#22283 = CARTESIAN_POINT ( 'NONE',  ( 55.49584447822657296, 70.91003759562335063, -15.34602024131217846 ) ) ;
#22284 = CARTESIAN_POINT ( 'NONE',  ( -1.239374126674604337, -42.99367564261289942, -16.50008610789281605 ) ) ;
#22285 = B_SPLINE_CURVE_WITH_KNOTS ( 'NONE', 3,
 ( #17822, #17965, #17545, #19851, #28474, #15822, #26747 ),
 .UNSPECIFIED., .F., .F.,
 ( 4, 3, 4 ),
 ( 5.958491062770612542E-16, 0.02816610861753249956, 0.04000277880656279150 ),
 .UNSPECIFIED. ) ;
#22286 = CARTESIAN_POINT ( 'NONE',  ( 1.834118845439484335, -59.18411796427140814, 132.4921483272726164 ) ) ;
#22287 = ORIENTED_EDGE ( 'NONE', *, *, #8815, .T. ) ;
#22288 = CARTESIAN_POINT ( 'NONE',  ( 5.340103556456464950, -133.7487107983440637, -62.06990747183822066 ) ) ;
#22289 = CARTESIAN_POINT ( 'NONE',  ( 26.11404676487257603, 33.91085499298520034, -108.0249973236464314 ) ) ;
#22290 = CARTESIAN_POINT ( 'NONE',  ( 25.87036335909428075, -98.40409479825397909, -55.67065048714113118 ) ) ;
#22291 = ORIENTED_EDGE ( 'NONE', *, *, #6568, .T. ) ;
#22292 = ORIENTED_EDGE ( 'NONE', *, *, #7824, .T. ) ;
#22293 = VERTEX_POINT ( 'NONE', #21268 ) ;
#22294 = CARTESIAN_POINT ( 'NONE',  ( -1.048172774974284405, -27.73787987941035027, -36.44231470008705998 ) ) ;
#22295 = LINE ( 'NONE', #7048, #3647 ) ;
#22296 = B_SPLINE_CURVE_WITH_KNOTS ( 'NONE', 3,
 ( #4871, #24047, #6900, #2265 ),
 .UNSPECIFIED., .F., .F.,
 ( 4, 4 ),
 ( 0.000000000000000000, 0.01077107196513949622 ),
 .UNSPECIFIED. ) ;
#22297 = CARTESIAN_POINT ( 'NONE',  ( -1.045287976400365970, -37.92705037016778391, -25.66401692419976399 ) ) ;
#22298 = CARTESIAN_POINT ( 'NONE',  ( 55.49584447822657296, -42.42793568432917795, -58.85239198729230026 ) ) ;
#22299 = CARTESIAN_POINT ( 'NONE',  ( -2.904412668506678674, -47.56768199507435213, -2.864640348250463653 ) ) ;
#22300 = CARTESIAN_POINT ( 'NONE',  ( 25.64704443564078318, -91.26857357624521683, -66.47548630737952635 ) ) ;
#22301 = ORIENTED_EDGE ( 'NONE', *, *, #3939, .T. ) ;
#22302 = CARTESIAN_POINT ( 'NONE',  ( 2.433796855181205476, 132.3327394885231456, 60.50726454507948660 ) ) ;
#22303 = CARTESIAN_POINT ( 'NONE',  ( 109.1592201516379674, -0.007780772729118872952, -0.001127733110579658832 ) ) ;
#22304 = DIRECTION ( 'NONE',  ( 1.000000000000000000, -0.000000000000000000, -0.000000000000000000 ) ) ;
#22305 = CARTESIAN_POINT ( 'NONE',  ( -18.41936578851709783, 18.42310649277627022, -38.22933728004698395 ) ) ;
#22306 = CARTESIAN_POINT ( 'NONE',  ( 109.1778270068192853, 0.009307953841270274684, -0.0003511581237512639711 ) ) ;
#22307 = EDGE_CURVE ( 'NONE', #7524, #19216, #2236, .T. ) ;
#22308 = ORIENTED_EDGE ( 'NONE', *, *, #6493, .T. ) ;
#22309 = CARTESIAN_POINT ( 'NONE',  ( 109.1592201516379674, -0.005631912476305732905, -0.005485778713193728215 ) ) ;
#22310 = ORIENTED_EDGE ( 'NONE', *, *, #15120, .F. ) ;
#22311 = CARTESIAN_POINT ( 'NONE',  ( -20.20700224038492721, -27.82980252387812570, 10.08426345511618649 ) ) ;
#22312 = ADVANCED_FACE ( 'NONE', ( #4543 ), #15478, .F. ) ;
#22313 = CARTESIAN_POINT ( 'NONE',  ( 25.64708010899966695, -56.50300922386526992, -97.75667227735142717 ) ) ;
#22314 = ORIENTED_EDGE ( 'NONE', *, *, #10002, .T. ) ;
#22315 = EDGE_CURVE ( 'NONE', #26223, #25791, #4294, .T. ) ;
#22316 = VERTEX_POINT ( 'NONE', #8883 ) ;
#22317 = ORIENTED_EDGE ( 'NONE', *, *, #10544, .T. ) ;
#22318 = CARTESIAN_POINT ( 'NONE',  ( -20.20700224038492721, 27.82980252387819675, -10.08426345511598932 ) ) ;
#22319 = CARTESIAN_POINT ( 'NONE',  ( -20.20997486282892552, 3.551351076220724598E-15, -29.60348406988233450 ) ) ;
#22320 = CARTESIAN_POINT ( 'NONE',  ( 9.884929003653626367, 144.4113244745771851, 42.50195158091081993 ) ) ;
#22321 =( BOUNDED_SURFACE ( )  B_SPLINE_SURFACE ( 3, 1, ( 
 ( #18240, #11925 ),
 ( #9777, #25043 ),
 ( #11789, #5443 ),
 ( #25474, #7773 ) ),
 .UNSPECIFIED., .F., .F., .F. ) 
 B_SPLINE_SURFACE_WITH_KNOTS ( ( 4, 4 ),
 ( 2, 2 ),
 ( 0.000000000000000000, 1.000000000000000000 ),
 ( 0.000000000000000000, 1.000000000000000000 ),
 .UNSPECIFIED. ) 
 GEOMETRIC_REPRESENTATION_ITEM ( )  RATIONAL_B_SPLINE_SURFACE ( (
 ( 1.000000000000000000, 1.000000000000000000),
 ( 0.9934239774497838349, 0.8357310067453913582),
 ( 0.9934239774497838349, 0.8357310067453913582),
 ( 1.000000000000000000, 1.000000000000000000) ) ) 
 REPRESENTATION_ITEM ( '' )  SURFACE ( )  );
#22322 = CARTESIAN_POINT ( 'NONE',  ( 10.93730112725990367, -84.82621002473354110, -125.1380233598488019 ) ) ;
#22323 = VERTEX_POINT ( 'NONE', #21541 ) ;
#22324 = CARTESIAN_POINT ( 'NONE',  ( 10.93730112726003156, 84.82621002473607064, -125.1380233598471960 ) ) ;
#22325 = EDGE_CURVE ( 'NONE', #4812, #20099, #5687, .T. ) ;
#22326 = FACE_OUTER_BOUND ( 'NONE', #6113, .T. ) ;
#22327 = ORIENTED_EDGE ( 'NONE', *, *, #4246, .F. ) ;
#22328 = CARTESIAN_POINT ( 'NONE',  ( 1.833485406944043827, 85.72460230293849293, -117.0814567582535659 ) ) ;
#22329 = VERTEX_POINT ( 'NONE', #6436 ) ;
#22330 = CARTESIAN_POINT ( 'NONE',  ( -7.078251931573406708, 44.92740138729204347, 26.33626633876174239 ) ) ;
#22331 = B_SPLINE_CURVE_WITH_KNOTS ( 'NONE', 3,
 ( #22869, #11472, #11334, #19970, #27001, #20245, #9333, #9175 ),
 .UNSPECIFIED., .F., .F.,
 ( 4, 2, 2, 4 ),
 ( 8.673617379884035472E-19, 0.0002429592666046771939, 0.0004859185332093535203, 0.0009718370664186919703 ),
 .UNSPECIFIED. ) ;
#22332 = CARTESIAN_POINT ( 'NONE',  ( -21.41430102051745266, 29.81033373822138799, 7.777552968935449229 ) ) ;
#22333 = CARTESIAN_POINT ( 'NONE',  ( -2.265401668238148591, 46.93990709177546705, 2.645701981445969686 ) ) ;
#22334 = CARTESIAN_POINT ( 'NONE',  ( 19.66333377628711432, 24.23123354948839747, 135.6014041990442252 ) ) ;
#22335 = DIRECTION ( 'NONE',  ( 0.000000000000000000, 5.223019709707975211E-21, -1.000000000000000000 ) ) ;
#22336 = EDGE_CURVE ( 'NONE', #13485, #14349, #21114, .T. ) ;
#22337 = CARTESIAN_POINT ( 'NONE',  ( 10.93730112725992853, -56.95489579269655422, -140.0398180619117738 ) ) ;
#22338 = DIRECTION ( 'NONE',  ( -1.000000000000000000, -0.000000000000000000, -0.000000000000000000 ) ) ;
#22339 = EDGE_CURVE ( 'NONE', #7653, #21943, #4647, .T. ) ;
#22340 = CARTESIAN_POINT ( 'NONE',  ( 26.11404676487259024, 97.48350837663691948, -57.58742681967348176 ) ) ;
#22341 = CARTESIAN_POINT ( 'NONE',  ( -1.259920593601978833, 44.39818421957814820, -12.06711544331578168 ) ) ;
#22342 = CARTESIAN_POINT ( 'NONE',  ( 1.833485406944057594, 141.8265699653871366, -30.69200235378795227 ) ) ;
#22343 = CARTESIAN_POINT ( 'NONE',  ( -1.113427685306987991, 38.22586258295232398, 25.34053733836490707 ) ) ;
#22344 = AXIS2_PLACEMENT_3D ( 'NONE', #8693, #21649, #2058 ) ;
#22345 = ORIENTED_EDGE ( 'NONE', *, *, #5675, .F. ) ;
#22346 = ORIENTED_EDGE ( 'NONE', *, *, #17635, .T. ) ;
#22347 = CARTESIAN_POINT ( 'NONE',  ( 25.87036335909424878, 24.47383578007130112, 110.3794299719620682 ) ) ;
#22348 = CARTESIAN_POINT ( 'NONE',  ( 109.1586900883932856, 0.004851151255037359014, 0.005236795036860563031 ) ) ;
#22349 = ORIENTED_EDGE ( 'NONE', *, *, #17056, .F. ) ;
#22350 = ORIENTED_EDGE ( 'NONE', *, *, #5260, .F. ) ;
#22351 = ORIENTED_EDGE ( 'NONE', *, *, #20304, .F. ) ;
#22352 = CARTESIAN_POINT ( 'NONE',  ( -20.38016308990357572, -1.509191766064412299, -29.73560196176845238 ) ) ;
#22353 = CARTESIAN_POINT ( 'NONE',  ( -1.048996300304507523, 36.59642367107745997, -27.53442103413706477 ) ) ;
#22354 = B_SPLINE_CURVE_WITH_KNOTS ( 'NONE', 3,
 ( #25723, #19638, #10594, #21525 ),
 .UNSPECIFIED., .F., .F.,
 ( 4, 4 ),
 ( 0.000000000000000000, 0.01077107196513848661 ),
 .UNSPECIFIED. ) ;
#22355 = CARTESIAN_POINT ( 'NONE',  ( -1.050231094221198536, 43.63617436699759367, 13.91061116148147292 ) ) ;
#22356 = CARTESIAN_POINT ( 'NONE',  ( -55.24300891470650754, 0.005486913146700745682, -0.008142823778062297305 ) ) ;
#22357 = CARTESIAN_POINT ( 'NONE',  ( -55.24271866751342941, 0.006671293903669565407, -0.006757859501006440936 ) ) ;
#22358 = CARTESIAN_POINT ( 'NONE',  ( -1.155001620486255209, -45.85729774065936937, -2.068551059060163677 ) ) ;
#22359 = CARTESIAN_POINT ( 'NONE',  ( 26.11404676487259024, -103.8885755249566643, -45.01677474591514283 ) ) ;
#22360 = DIRECTION ( 'NONE',  ( 0.7637818620346800147, 0.6451161201712181104, 0.02150485345384620800 ) ) ;
#22361 = CARTESIAN_POINT ( 'NONE',  ( -20.20700224038492721, -16.58740185276692358, 24.51628800869065827 ) ) ;
#22362 = CARTESIAN_POINT ( 'NONE',  ( 10.93730112725936721, 145.2260730187397542, 42.00474393596321931 ) ) ;
#22363 = CARTESIAN_POINT ( 'NONE',  ( 109.1592201516379674, -0.004867031887019586216, -0.006174480289199391417 ) ) ;
#22364 =( BOUNDED_SURFACE ( )  B_SPLINE_SURFACE ( 3, 1, ( 
 ( #5210, #18007 ),
 ( #24808, #15866 ),
 ( #13986, #5060 ),
 ( #7533, #11544 ) ),
 .UNSPECIFIED., .F., .F., .F. ) 
 B_SPLINE_SURFACE_WITH_KNOTS ( ( 4, 4 ),
 ( 2, 2 ),
 ( 0.000000000000000000, 1.000000000000000000 ),
 ( 0.000000000000000000, 1.000000000000000000 ),
 .UNSPECIFIED. ) 
 GEOMETRIC_REPRESENTATION_ITEM ( )  RATIONAL_B_SPLINE_SURFACE ( (
 ( 1.000000000000000000, 1.000000000000000000),
 ( 0.7789835883360576307, 0.9689951854195403280),
 ( 0.7789835883360576307, 0.9689951854195403280),
 ( 1.000000000000000000, 1.000000000000000000) ) ) 
 REPRESENTATION_ITEM ( '' )  SURFACE ( )  );
#22365 = EDGE_CURVE ( 'NONE', #8723, #14914, #11844, .T. ) ;
#22366 = CARTESIAN_POINT ( 'NONE',  ( -7.733045908741329022, -47.75066202881810540, -21.80378472388470001 ) ) ;
#22367 = CARTESIAN_POINT ( 'NONE',  ( -7.078251931573406708, -5.101176922831029081, -51.82710018979473432 ) ) ;
#22368 = FACE_BOUND ( 'NONE', #14181, .T. ) ;
#22369 = EDGE_CURVE ( 'NONE', #1487, #18251, #14846, .T. ) ;
#22370 = ORIENTED_EDGE ( 'NONE', *, *, #20442, .F. ) ;
#22372 = CARTESIAN_POINT ( 'NONE',  ( 25.64703792032471696, -66.48786612795814221, -91.25955007190280810 ) ) ;
#22371 = CARTESIAN_POINT ( 'NONE',  ( -55.25719721206881729, 0.008651607285661618019, -0.007063345920781386421 ) ) ;
#22373 = CARTESIAN_POINT ( 'NONE',  ( 25.73574536432413495, -22.69874377039358038, -110.6664861019686583 ) ) ;
#22374 = CARTESIAN_POINT ( 'NONE',  ( 25.64708010899961721, 45.97512510001905639, 103.1273237223351344 ) ) ;
#22375 = FACE_OUTER_BOUND ( 'NONE', #26192, .T. ) ;
#22376 = CARTESIAN_POINT ( 'NONE',  ( -4.178947244162637631, -31.41809272265950170, -37.51424432987639079 ) ) ;
#22377 = ORIENTED_EDGE ( 'NONE', *, *, #3188, .F. ) ;
#22378 = CARTESIAN_POINT ( 'NONE',  ( 32.73300124599735739, -3.836798148479648507, 117.5726003567929610 ) ) ;
#22379 = ORIENTED_EDGE ( 'NONE', *, *, #20477, .F. ) ;
#22380 = CARTESIAN_POINT ( 'NONE',  ( 2.263178607246706164, -84.32376080825635256, 118.4461883615812070 ) ) ;
#22381 = VERTEX_POINT ( 'NONE', #17640 ) ;
#22382 = DIRECTION ( 'NONE',  ( 0.7563875759206388771, -0.2351350468682826267, 0.6104009704506950795 ) ) ;
#22383 = ORIENTED_EDGE ( 'NONE', *, *, #24817, .F. ) ;
#22384 = CARTESIAN_POINT ( 'NONE',  ( 1.832998868059858122, -96.70023740551049229, -108.1944082009167403 ) ) ;
#22385 = VERTEX_POINT ( 'NONE', #24009 ) ;
#22386 = CARTESIAN_POINT ( 'NONE',  ( -1.045287976400365970, -45.76855895860947498, -1.530335034933654859 ) ) ;
#22387 = B_SPLINE_CURVE_WITH_KNOTS ( 'NONE', 3,
 ( #16132, #9663, #1303, #2902, #11679, #25076, #3182 ),
 .UNSPECIFIED., .F., .F.,
 ( 4, 3, 4 ),
 ( 1.062518129035794345E-17, 0.0007657099931970561164, 0.001530725384384652287 ),
 .UNSPECIFIED. ) ;
#22388 = DIRECTION ( 'NONE',  ( 0.000000000000000000, 0.000000000000000000, 1.000000000000000000 ) ) ;
#22389 = CARTESIAN_POINT ( 'NONE',  ( 2.433796855181205476, 137.9325382748285165, 46.34326152018790168 ) ) ;
#22390 = CARTESIAN_POINT ( 'NONE',  ( 1.833603222531957622, 29.73464781350257624, 142.0304769734129877 ) ) ;
#22391 = EDGE_CURVE ( 'NONE', #7760, #5960, #9455, .T. ) ;
#22392 = CARTESIAN_POINT ( 'NONE',  ( 109.1586059443104944, -0.006570129623060891148, 0.002622205828288661032 ) ) ;
#22393 = CARTESIAN_POINT ( 'NONE',  ( -20.20700224038492721, 24.51628800869048419, -16.58740185276719359 ) ) ;
#22394 = CARTESIAN_POINT ( 'NONE',  ( 2.433796855181233454, 71.49415740225254012, -126.7346379669248222 ) ) ;
#22395 = EDGE_CURVE ( 'NONE', #2245, #6115, #13199, .T. ) ;
#22396 = CARTESIAN_POINT ( 'NONE',  ( 25.64670758986457955, -110.3390515846396909, -23.96231489925003899 ) ) ;
#22397 = CARTESIAN_POINT ( 'NONE',  ( 32.73300124599740002, -89.94078864464006529, -75.82012867748569818 ) ) ;
#22398 = DIRECTION ( 'NONE',  ( -1.000000000000000000, -0.000000000000000000, -0.000000000000000000 ) ) ;
#22399 =( BOUNDED_SURFACE ( )  B_SPLINE_SURFACE ( 3, 1, ( 
 ( #21337, #3781 ),
 ( #8394, #23515 ),
 ( #6103, #10416 ),
 ( #3491, #23804 ) ),
 .UNSPECIFIED., .F., .F., .F. ) 
 B_SPLINE_SURFACE_WITH_KNOTS ( ( 4, 4 ),
 ( 2, 2 ),
 ( 0.000000000000000000, 1.000000000000000000 ),
 ( 0.000000000000000000, 1.000000000000000000 ),
 .UNSPECIFIED. ) 
 GEOMETRIC_REPRESENTATION_ITEM ( )  RATIONAL_B_SPLINE_SURFACE ( (
 ( 1.000000000000000000, 1.000000000000000000),
 ( 0.6386103224230316178, 0.9954351624131538845),
 ( 0.6386103224230316178, 0.9954351624131538845),
 ( 1.000000000000000000, 1.000000000000000000) ) ) 
 REPRESENTATION_ITEM ( '' )  SURFACE ( )  );
#22400 = ADVANCED_FACE ( 'NONE', ( #2372 ), #23094, .F. ) ;
#22401 = VERTEX_POINT ( 'NONE', #20513 ) ;
#22402 = CARTESIAN_POINT ( 'NONE',  ( -1.031422197589716205, 43.06660437151310816, -15.60268798220652187 ) ) ;
#22404 = CARTESIAN_POINT ( 'NONE',  ( -2.911734481061364566, -40.13920818157090054, -25.69892591260251535 ) ) ;
#22403 = CARTESIAN_POINT ( 'NONE',  ( 8.186469777911003831, 145.3272523831809053, -34.43598809570011099 ) ) ;
#22405 = CARTESIAN_POINT ( 'NONE',  ( 32.73300124599735739, -110.6325518752276622, 39.98094346392273479 ) ) ;
#22406 = CARTESIAN_POINT ( 'NONE',  ( 13.84597867724967379, 135.8932891738225806, -55.26821062125426920 ) ) ;
#22407 = CARTESIAN_POINT ( 'NONE',  ( -23.77929240705206482, -35.93174012244168836, 4.877832571065307654 ) ) ;
#22408 = EDGE_CURVE ( 'NONE', #21273, #7383, #2927, .T. ) ;
#22409 = EDGE_LOOP ( 'NONE', ( #26293, #2836, #8463, #21400 ) ) ;
#22410 = CARTESIAN_POINT ( 'NONE',  ( 25.73574536432417048, 98.23578516675037520, -55.78561308781378614 ) ) ;
#22411 = CARTESIAN_POINT ( 'NONE',  ( -1.619063947482197729, 46.30105812165548684, 2.489035965910320503 ) ) ;
#22412 = VERTEX_POINT ( 'NONE', #10136 ) ;
#22413 = CARTESIAN_POINT ( 'NONE',  ( 5.340103579038252057, -88.52145169228889188, -117.9209211655066696 ) ) ;
#22414 = ORIENTED_EDGE ( 'NONE', *, *, #28325, .F. ) ;
#22415 = DIRECTION ( 'NONE',  ( -1.000000000000000000, -0.000000000000000000, -0.000000000000000000 ) ) ;
#22417 = CARTESIAN_POINT ( 'NONE',  ( -21.41427618760446450, -30.75468365310881325, -1.815001260755733536 ) ) ;
#22416 = B_SPLINE_CURVE_WITH_KNOTS ( 'NONE', 3,
 ( #19267, #21853, #26032, #28039 ),
 .UNSPECIFIED., .F., .F.,
 ( 4, 4 ),
 ( 3.048060820747882759E-16, 0.01077107486149818383 ),
 .UNSPECIFIED. ) ;
#22418 = ORIENTED_EDGE ( 'NONE', *, *, #22838, .T. ) ;
#22419 = CARTESIAN_POINT ( 'NONE',  ( 25.64681081121879203, 112.2483031020015147, -12.21581276189692211 ) ) ;
#22420 = ORIENTED_EDGE ( 'NONE', *, *, #3879, .T. ) ;
#22421 = CARTESIAN_POINT ( 'NONE',  ( 13.84597867724975551, -132.0026437215596786, -64.00674338125978124 ) ) ;
#22422 = ORIENTED_EDGE ( 'NONE', *, *, #6733, .F. ) ;
#22423 = CARTESIAN_POINT ( 'NONE',  ( -55.25719721206881729, 0.006045473558784881206, 0.009391134844728978373 ) ) ;
#22424 = CARTESIAN_POINT ( 'NONE',  ( 24.01988960052052491, -115.5642432877696848, 61.78678588189985277 ) ) ;
#22425 = EDGE_CURVE ( 'NONE', #3673, #19518, #16707, .T. ) ;
#22426 = B_SPLINE_CURVE_WITH_KNOTS ( 'NONE', 3,
 ( #26401, #2203, #1789, #10735 ),
 .UNSPECIFIED., .F., .F.,
 ( 4, 4 ),
 ( 3.628665131031684266E-16, 0.01077107486149826536 ),
 .UNSPECIFIED. ) ;
#22427 = CARTESIAN_POINT ( 'NONE',  ( 25.64708228042120908, 107.3971738194636458, -34.85404436489383784 ) ) ;
#22428 = CARTESIAN_POINT ( 'NONE',  ( 10.93730112725990011, -151.0983828010091656, -4.928439153521871674 ) ) ;
#22429 = LINE ( 'NONE', #17936, #71 ) ;
#22430 = ADVANCED_FACE ( 'NONE', ( #27676 ), #17012, .T. ) ;
#22431 = ORIENTED_EDGE ( 'NONE', *, *, #7030, .T. ) ;
#22432 = CARTESIAN_POINT ( 'NONE',  ( 9.884929003653626367, 150.0922431698404864, 11.54837932063081674 ) ) ;
#22433 = CARTESIAN_POINT ( 'NONE',  ( -55.24271866751342941, -0.008488649505345844185, 0.004256484107793130807 ) ) ;
#22434 = CARTESIAN_POINT ( 'NONE',  ( 10.93730112725997294, 36.23586118136742584, -146.7718404940639516 ) ) ;
#22435 = ORIENTED_EDGE ( 'NONE', *, *, #24485, .F. ) ;
#22436 = EDGE_CURVE ( 'NONE', #2536, #7054, #13119, .T. ) ;
#22437 = ORIENTED_EDGE ( 'NONE', *, *, #22967, .F. ) ;
#22438 = CARTESIAN_POINT ( 'NONE',  ( 55.49584447822657296, 66.16986612640775434, 29.75369869230976860 ) ) ;
#22439 = CARTESIAN_POINT ( 'NONE',  ( -25.21435515916043713, -30.48034229288650820, -16.39063784838731053 ) ) ;
#22440 = CARTESIAN_POINT ( 'NONE',  ( 25.86096068574582318, -24.48003142199159043, 110.3716997142157510 ) ) ;
#22441 = CARTESIAN_POINT ( 'NONE',  ( -4.178947244162567465, -37.51424432987625579, 31.41809272265961539 ) ) ;
#22442 = LINE ( 'NONE', #6475, #20745 ) ;
#22443 = CARTESIAN_POINT ( 'NONE',  ( 26.04756280548354042, 47.04636360340825263, 102.9366382251194807 ) ) ;
#22444 = ORIENTED_EDGE ( 'NONE', *, *, #12634, .T. ) ;
#22445 = CARTESIAN_POINT ( 'NONE',  ( 2.433796855181233454, 145.5024947199069913, -1.451562450950139249 ) ) ;
#22446 = CARTESIAN_POINT ( 'NONE',  ( -1.323439229708149867, -16.42345129173367013, -43.04565903621277556 ) ) ;
#22447 = CIRCLE ( 'NONE', #24290, 151.1787379149930359 ) ;
#22448 = CARTESIAN_POINT ( 'NONE',  ( 1.833603222531971610, -145.1089511853978422, -0.4449221977534632000 ) ) ;
#22449 = CARTESIAN_POINT ( 'NONE',  ( -23.79248802219728276, 13.25839849636400203, 30.42578156345371454 ) ) ;
#22450 =( BOUNDED_SURFACE ( )  B_SPLINE_SURFACE ( 3, 1, ( 
 ( #24169, #10506 ),
 ( #6199, #12651 ),
 ( #19274, #15216 ),
 ( #28047, #23897 ) ),
 .UNSPECIFIED., .F., .F., .F. ) 
 B_SPLINE_SURFACE_WITH_KNOTS ( ( 4, 4 ),
 ( 2, 2 ),
 ( 0.000000000000000000, 1.000000000000000000 ),
 ( 0.000000000000000000, 1.000000000000000000 ),
 .UNSPECIFIED. ) 
 GEOMETRIC_REPRESENTATION_ITEM ( )  RATIONAL_B_SPLINE_SURFACE ( (
 ( 1.000000000000000000, 1.000000000000000000),
 ( 0.9956975270656955868, 0.8568959468854907557),
 ( 0.9956975270656955868, 0.8568959468854907557),
 ( 1.000000000000000000, 1.000000000000000000) ) ) 
 REPRESENTATION_ITEM ( '' )  SURFACE ( )  );
#22451 = CARTESIAN_POINT ( 'NONE',  ( 109.1624594426973118, 0.01102230012606810090, 0.01154818537151459067 ) ) ;
#22452 = ORIENTED_EDGE ( 'NONE', *, *, #15897, .F. ) ;
#22453 = CARTESIAN_POINT ( 'NONE',  ( 109.1586059443104944, -0.002447596125905633375, 0.006637156007973973003 ) ) ;
#22454 = VERTEX_POINT ( 'NONE', #23671 ) ;
#22455 = CARTESIAN_POINT ( 'NONE',  ( 1.893872463202025624, 142.1730500379302384, -29.24569695044102602 ) ) ;
#22456 = CARTESIAN_POINT ( 'NONE',  ( 2.263178607246643992, -142.5035407554793494, -28.85718361841066582 ) ) ;
#22457 = ORIENTED_EDGE ( 'NONE', *, *, #18337, .T. ) ;
#22458 = B_SPLINE_CURVE_WITH_KNOTS ( 'NONE', 3,
 ( #18136, #26624, #11377, #11521, #20297, #3042 ),
 .UNSPECIFIED., .F., .F.,
 ( 4, 2, 4 ),
 ( 9.745765416140531346E-18, 0.0006311636237756831393, 0.001262327247551356521 ),
 .UNSPECIFIED. ) ;
#22459 =( BOUNDED_SURFACE ( )  B_SPLINE_SURFACE ( 3, 1, ( 
 ( #26203, #15395 ),
 ( #24646, #16553 ),
 ( #12100, #16413 ),
 ( #11950, #27343 ) ),
 .UNSPECIFIED., .F., .F., .F. ) 
 B_SPLINE_SURFACE_WITH_KNOTS ( ( 4, 4 ),
 ( 2, 2 ),
 ( 0.000000000000000000, 1.000000000000000000 ),
 ( 0.000000000000000000, 1.000000000000000000 ),
 .UNSPECIFIED. ) 
 GEOMETRIC_REPRESENTATION_ITEM ( )  RATIONAL_B_SPLINE_SURFACE ( (
 ( 1.000000000000000000, 1.000000000000000000),
 ( 0.9956975270656954757, 0.8568959468854893125),
 ( 0.9956975270656954757, 0.8568959468854893125),
 ( 1.000000000000000000, 1.000000000000000000) ) ) 
 REPRESENTATION_ITEM ( '' )  SURFACE ( )  );
#22460 = EDGE_LOOP ( 'NONE', ( #5168, #20598, #15915, #9502 ) ) ;
#22461 = ORIENTED_EDGE ( 'NONE', *, *, #6087, .F. ) ;
#22462 = CARTESIAN_POINT ( 'NONE',  ( -24.53239521893646469, 14.09666242510788337, -30.86654523348667567 ) ) ;
#22463 = AXIS2_PLACEMENT_3D ( 'NONE', #22510, #11275, #24383 ) ;
#22464 = CARTESIAN_POINT ( 'NONE',  ( -20.20700224038492721, 28.44216453106548315, 8.199606986804035103 ) ) ;
#22465 = CARTESIAN_POINT ( 'NONE',  ( -24.53237795827024570, -33.25734978085267102, -6.738475012719991497 ) ) ;
#22466 = VECTOR ( 'NONE', #11421, 1000.000000000000000 ) ;
#22467 = CARTESIAN_POINT ( 'NONE',  ( 28.37644542392843405, -69.76573497039019855, -102.9230687709016081 ) ) ;
#22468 = CARTESIAN_POINT ( 'NONE',  ( -20.47566262905010603, 23.19796652405701565, 18.81547655725221091 ) ) ;
#22469 = ORIENTED_EDGE ( 'NONE', *, *, #15901, .T. ) ;
#22470 = CARTESIAN_POINT ( 'NONE',  ( -20.47566262905009538, -25.06314747784824348, 16.24827521404678521 ) ) ;
#22471 = ADVANCED_FACE ( 'NONE', ( #28092 ), #5414, .F. ) ;
#22472 = CARTESIAN_POINT ( 'NONE',  ( 25.64708010899964918, -103.1273237223352766, 45.97512510001868691 ) ) ;
#22473 = CARTESIAN_POINT ( 'NONE',  ( -2.904412668506656026, 44.35433137608966092, 17.42365698954652586 ) ) ;
#22474 = ORIENTED_EDGE ( 'NONE', *, *, #2933, .F. ) ;
#22475 = ADVANCED_FACE ( 'NONE', ( #5450, #8809 ), #301, .F. ) ;
#22476 = ORIENTED_EDGE ( 'NONE', *, *, #7257, .F. ) ;
#22477 = CARTESIAN_POINT ( 'NONE',  ( -9.156249394959713683, -38.89149400288378899, 38.17928057392034447 ) ) ;
#22478 = CARTESIAN_POINT ( 'NONE',  ( 26.28373643307399377, 123.8418562193902659, -30.57614217577341620 ) ) ;
#22479 = CARTESIAN_POINT ( 'NONE',  ( 2.433796855181205476, -145.5024947199069629, -1.451562450951161987 ) ) ;
#22480 = EDGE_CURVE ( 'NONE', #3442, #8511, #17332, .T. ) ;
#22481 = B_SPLINE_CURVE_WITH_KNOTS ( 'NONE', 3,
 ( #8147, #23269, #3519, #25566, #19207, #12301, #1777, #17184 ),
 .UNSPECIFIED., .F., .F.,
 ( 4, 2, 2, 4 ),
 ( 0.000000000000000000, 0.002761524886576556103, 0.005523049773153112206, 0.01104609954630622441 ),
 .UNSPECIFIED. ) ;
#22482 = CARTESIAN_POINT ( 'NONE',  ( 109.1624594426973260, -0.006066618937909569638, -0.01476644236456057385 ) ) ;
#22483 = CARTESIAN_POINT ( 'NONE',  ( -55.25719721206881729, -0.006045473558784178643, -0.009391134844729129294 ) ) ;
#22484 = CARTESIAN_POINT ( 'NONE',  ( -1.044557008772706297, 44.03203053429572833, -12.57891310333364210 ) ) ;
#22485 = CARTESIAN_POINT ( 'NONE',  ( -20.20700224038492010, -8.199606986804138131, 28.44216453106544762 ) ) ;
#22486 = CARTESIAN_POINT ( 'NONE',  ( -20.21097721650785672, -17.67178726257375487, -23.76068422213751674 ) ) ;
#22487 = CARTESIAN_POINT ( 'NONE',  ( -1.058197053496178874, 44.07533330186787168, -12.47644286888530019 ) ) ;
#22488 = CARTESIAN_POINT ( 'NONE',  ( 55.79472521941426777, -48.13855120843846436, -54.55111121764132776 ) ) ;
#22489 = CARTESIAN_POINT ( 'NONE',  ( -24.53237795827028833, 3.868415699416160258, 33.71192251888858493 ) ) ;
#22490 = EDGE_LOOP ( 'NONE', ( #17170, #10837, #19353, #14249 ) ) ;
#22491 = CARTESIAN_POINT ( 'NONE',  ( 1.833206308920067196, -96.54250175814047452, -108.3342547309375306 ) ) ;
#22492 = B_SPLINE_CURVE_WITH_KNOTS ( 'NONE', 3,
 ( #10936, #6340, #19699, #6764, #19987, #13506 ),
 .UNSPECIFIED., .F., .F.,
 ( 4, 2, 4 ),
 ( 1.042864983293993125E-17, 0.0006311571484585992839, 0.001262314296917197484 ),
 .UNSPECIFIED. ) ;
#22493 = CARTESIAN_POINT ( 'NONE',  ( 1.834118845439484335, -117.2918069668795056, -85.43746956709969709 ) ) ;
#22494 = ORIENTED_EDGE ( 'NONE', *, *, #9403, .F. ) ;
#22495 = VERTEX_POINT ( 'NONE', #2603 ) ;
#22496 = ORIENTED_EDGE ( 'NONE', *, *, #4084, .T. ) ;
#22497 =( BOUNDED_SURFACE ( )  B_SPLINE_SURFACE ( 3, 1, ( 
 ( #14984, #4049 ),
 ( #17283, #15112 ),
 ( #4189, #23372 ),
 ( #3623, #12400 ) ),
 .UNSPECIFIED., .F., .F., .F. ) 
 B_SPLINE_SURFACE_WITH_KNOTS ( ( 4, 4 ),
 ( 2, 2 ),
 ( 0.000000000000000000, 1.000000000000000000 ),
 ( 0.000000000000000000, 1.000000000000000000 ),
 .UNSPECIFIED. ) 
 GEOMETRIC_REPRESENTATION_ITEM ( )  RATIONAL_B_SPLINE_SURFACE ( (
 ( 1.000000000000000000, 1.000000000000000000),
 ( 0.9934239774497837239, 0.8357310067453919133),
 ( 0.9934239774497837239, 0.8357310067453919133),
 ( 1.000000000000000000, 1.000000000000000000) ) ) 
 REPRESENTATION_ITEM ( '' )  SURFACE ( )  );
#22498 = CARTESIAN_POINT ( 'NONE',  ( -1.049817751779873465, 37.35030165458175588, -26.50542916749582645 ) ) ;
#22499 = CARTESIAN_POINT ( 'NONE',  ( -55.24340739397742084, 0.006539691034612836289, -0.007744344507854826129 ) ) ;
#22500 = CARTESIAN_POINT ( 'NONE',  ( -4.162674018437130030, -18.33413805792406492, 45.34593312138898824 ) ) ;
#22501 = EDGE_CURVE ( 'NONE', #21108, #5582, #8428, .T. ) ;
#22502 = CARTESIAN_POINT ( 'NONE',  ( -20.37983603106074071, -16.25728007463423808, -24.94323704205431369 ) ) ;
#22503 = CARTESIAN_POINT ( 'NONE',  ( -55.24271866751342941, -0.008488649505342596782, -0.004256484107795601053 ) ) ;
#22504 = CARTESIAN_POINT ( 'NONE',  ( 26.11404676487257603, -112.4785329405481065, -12.95861723607569438 ) ) ;
#22505 = CARTESIAN_POINT ( 'NONE',  ( 2.433796855181205476, 16.65276281464756636, -144.5536872373190533 ) ) ;
#22506 = CARTESIAN_POINT ( 'NONE',  ( 25.98107933586700469, 33.92073193606590564, 107.9289867379274312 ) ) ;
#22507 = CARTESIAN_POINT ( 'NONE',  ( 55.79472521941428198, 48.13855120843958701, -54.55111121764033300 ) ) ;
#22508 = CARTESIAN_POINT ( 'NONE',  ( -6.574463467970653063, -47.03022655117387529, 20.55340846381182018 ) ) ;
#22509 = CARTESIAN_POINT ( 'NONE',  ( -20.57838717382308147, -16.28767523336139078, -25.16001208503099917 ) ) ;
#22510 = CARTESIAN_POINT ( 'NONE',  ( -40.00000000000000000, 0.000000000000000000, 0.000000000000000000 ) ) ;
#22511 = ORIENTED_EDGE ( 'NONE', *, *, #6968, .T. ) ;
#22513 = FACE_OUTER_BOUND ( 'NONE', #6814, .T. ) ;
#22512 = LINE ( 'NONE', #22808, #24975 ) ;
#22514 = CARTESIAN_POINT ( 'NONE',  ( 13.36082413113063083, -135.4964217943302458, -70.90215303572267658 ) ) ;
#22515 = CARTESIAN_POINT ( 'NONE',  ( 32.73300124599740002, 72.21147546950675178, -92.86301839379947864 ) ) ;
#22516 = CARTESIAN_POINT ( 'NONE',  ( -20.20612091757419648, 29.57813639663782013, 1.137293889216468790 ) ) ;
#22517 = CARTESIAN_POINT ( 'NONE',  ( -1.259972190295300054, 16.33417789844434509, 43.01178231151312303 ) ) ;
#22518 = VERTEX_POINT ( 'NONE', #25181 ) ;
#22519 = CARTESIAN_POINT ( 'NONE',  ( 109.1592201516379674, -0.006649399203953420406, -0.004194960840980667231 ) ) ;
#22520 = ORIENTED_EDGE ( 'NONE', *, *, #11019, .T. ) ;
#22521 = CARTESIAN_POINT ( 'NONE',  ( 26.11404676487259024, 103.8885755249575453, -45.01677474591305383 ) ) ;
#22522 = CARTESIAN_POINT ( 'NONE',  ( -20.24419206586950892, -23.20105925399712987, 18.44224248888897577 ) ) ;
#22523 = ORIENTED_EDGE ( 'NONE', *, *, #9432, .F. ) ;
#22524 = VERTEX_POINT ( 'NONE', #4914 ) ;
#22525 = DIRECTION ( 'NONE',  ( -1.000000000000000000, -0.000000000000000000, -0.000000000000000000 ) ) ;
#22526 = VECTOR ( 'NONE', #27674, 1000.000000000000000 ) ;
#22527 = ORIENTED_EDGE ( 'NONE', *, *, #19717, .F. ) ;
#22528 = B_SPLINE_CURVE_WITH_KNOTS ( 'NONE', 3,
 ( #646, #19938, #9437, #13303, #220, #7000 ),
 .UNSPECIFIED., .F., .F.,
 ( 4, 2, 4 ),
 ( 3.565531997320606436E-16, 0.003576372551511159629, 0.007152745103021962772 ),
 .UNSPECIFIED. ) ;
#22529 = ORIENTED_EDGE ( 'NONE', *, *, #8024, .T. ) ;
#22530 = DIRECTION ( 'NONE',  ( -1.000000000000000000, -0.000000000000000000, -0.000000000000000000 ) ) ;
#22531 = EDGE_CURVE ( 'NONE', #25702, #1293, #21479, .T. ) ;
#22532 = EDGE_CURVE ( 'NONE', #25711, #17719, #10835, .T. ) ;
#22533 = B_SPLINE_CURVE_WITH_KNOTS ( 'NONE', 3,
 ( #12929, #19686, #686, #9340, #12060, #14060, #11626 ),
 .UNSPECIFIED., .F., .F.,
 ( 4, 3, 4 ),
 ( 0.000000000000000000, 0.02398743853561428538, 0.04000277880656220864 ),
 .UNSPECIFIED. ) ;
#22534 = LINE ( 'NONE', #20358, #24407 ) ;
#22535 = EDGE_CURVE ( 'NONE', #1639, #6924, #1546, .T. ) ;
#22536 =( BOUNDED_SURFACE ( )  B_SPLINE_SURFACE ( 3, 1, ( 
 ( #10535, #13231 ),
 ( #28346, #2282 ),
 ( #4325, #11091 ),
 ( #22021, #148 ) ),
 .UNSPECIFIED., .F., .F., .F. ) 
 B_SPLINE_SURFACE_WITH_KNOTS ( ( 4, 4 ),
 ( 2, 2 ),
 ( 0.000000000000000000, 1.000000000000000000 ),
 ( 0.000000000000000000, 1.000000000000000000 ),
 .UNSPECIFIED. ) 
 GEOMETRIC_REPRESENTATION_ITEM ( )  RATIONAL_B_SPLINE_SURFACE ( (
 ( 1.000000000000000000, 1.000000000000000000),
 ( 0.6386103224230316178, 0.9954351624131538845),
 ( 0.6386103224230316178, 0.9954351624131538845),
 ( 1.000000000000000000, 1.000000000000000000) ) ) 
 REPRESENTATION_ITEM ( '' )  SURFACE ( )  );
#22537 = CARTESIAN_POINT ( 'NONE',  ( -1.019300379054419725, -25.26451264419615939, 38.21680004809191189 ) ) ;
#22538 = CARTESIAN_POINT ( 'NONE',  ( -1.583189561560253589, 36.01941156322789084, -29.24830400313178558 ) ) ;
#22539 = B_SPLINE_CURVE_WITH_KNOTS ( 'NONE', 3,
 ( #27081, #7693, #23093, #24821, #25099, #5364, #16595 ),
 .UNSPECIFIED., .F., .F.,
 ( 4, 3, 4 ),
 ( 5.601303642928431203E-16, 0.02816610861753243017, 0.04000277880656278456 ),
 .UNSPECIFIED. ) ;
#22540 = CARTESIAN_POINT ( 'NONE',  ( 109.1586900883932856, 0.005715190711481724431, -0.004277182003227242291 ) ) ;
#22541 = CARTESIAN_POINT ( 'NONE',  ( 32.73300124599732186, 0.000000000000000000, 0.000000000000000000 ) ) ;
#22542 = CIRCLE ( 'NONE', #15147, 34.60786435723138510 ) ;
#22543 = DIRECTION ( 'NONE',  ( 1.000000000000000000, -6.938893903907226837E-18, 1.734723475976806709E-18 ) ) ;
#22544 = CARTESIAN_POINT ( 'NONE',  ( 25.64670758986456889, -0.4979020485385241557, 112.9099239813695448 ) ) ;
#22545 = CARTESIAN_POINT ( 'NONE',  ( -1.050230347699841582, 0.2550051351977194458, 45.79907861674081460 ) ) ;
#22546 = EDGE_LOOP ( 'NONE', ( #22745, #22474, #26739, #14983 ) ) ;
#22547 = CARTESIAN_POINT ( 'NONE',  ( -23.77929240705207192, -17.17389748746940370, 31.93650644494359270 ) ) ;
#22549 = CARTESIAN_POINT ( 'NONE',  ( 25.64670758986457244, 45.46974729533283721, 103.3508631837546119 ) ) ;
#22548 = CARTESIAN_POINT ( 'NONE',  ( -1.619063947482194177, 29.22875152547808852, 35.99532424477347092 ) ) ;
#22550 = CARTESIAN_POINT ( 'NONE',  ( -20.57838717382308147, 1.611677988432778319, 29.92853265176829325 ) ) ;
#22551 = DIRECTION ( 'NONE',  ( 0.000000000000000000, 0.000000000000000000, 1.000000000000000000 ) ) ;
#22552 = CARTESIAN_POINT ( 'NONE',  ( -23.79223135445719706, 24.83942264280432610, 22.01133905265658441 ) ) ;
#22553 = VERTEX_POINT ( 'NONE', #15693 ) ;
#22554 = CARTESIAN_POINT ( 'NONE',  ( 25.70243777736191149, 98.18050844655147102, -55.83795591307026029 ) ) ;
#22555 = DIRECTION ( 'NONE',  ( -0.7637818620346800147, -0.6201872550346679835, -0.1788995134688763367 ) ) ;
#22556 = CARTESIAN_POINT ( 'NONE',  ( 26.28373643307408614, -91.96212244992437945, 88.40064398364035014 ) ) ;
#22557 = ORIENTED_EDGE ( 'NONE', *, *, #24817, .T. ) ;
#22558 = CARTESIAN_POINT ( 'NONE',  ( 1.834118845439484335, 96.96525081350146991, -107.9567937753783298 ) ) ;
#22559 = ORIENTED_EDGE ( 'NONE', *, *, #1469, .F. ) ;
#22560 = CARTESIAN_POINT ( 'NONE',  ( -1.464342487929867209, -16.57334911911542363, -43.13914623307952922 ) ) ;
#22561 = ADVANCED_FACE ( 'NONE', ( #13389 ), #19730, .T. ) ;
#22562 = VECTOR ( 'NONE', #15227, 999.9999999999998863 ) ;
#22563 = CARTESIAN_POINT ( 'NONE',  ( -1.464342487929843450, 2.431462367721978435, 46.14921266389554688 ) ) ;
#22564 = AXIS2_PLACEMENT_3D ( 'NONE', #18484, #11579, #12012 ) ;
#22565 = EDGE_LOOP ( 'NONE', ( #20404, #17093, #889, #13121 ) ) ;
#22566 = CARTESIAN_POINT ( 'NONE',  ( -20.24399999263415495, -27.76448601145549233, -10.36954246768234889 ) ) ;
#22567 = AXIS2_PLACEMENT_3D ( 'NONE', #21099, #8042, #25588 ) ;
#22568 = EDGE_CURVE ( 'NONE', #13087, #10554, #169, .T. ) ;
#22569 = VERTEX_POINT ( 'NONE', #22340 ) ;
#22570 = FACE_OUTER_BOUND ( 'NONE', #14046, .T. ) ;
#22571 = ORIENTED_EDGE ( 'NONE', *, *, #6738, .T. ) ;
#22572 =( LENGTH_UNIT ( ) NAMED_UNIT ( * ) SI_UNIT ( .MILLI., .METRE. ) );
#22573 = CARTESIAN_POINT ( 'NONE',  ( -20.47566338032535782, -10.72601609985042792, -27.87687989047296355 ) ) ;
#22574 =( BOUNDED_SURFACE ( )  B_SPLINE_SURFACE ( 3, 1, ( 
 ( #9522, #20886 ),
 ( #5193, #13968 ),
 ( #18725, #2747 ),
 ( #27498, #1171 ) ),
 .UNSPECIFIED., .F., .F., .F. ) 
 B_SPLINE_SURFACE_WITH_KNOTS ( ( 4, 4 ),
 ( 2, 2 ),
 ( 0.000000000000000000, 1.000000000000000000 ),
 ( 0.000000000000000000, 1.000000000000000000 ),
 .UNSPECIFIED. ) 
 GEOMETRIC_REPRESENTATION_ITEM ( )  RATIONAL_B_SPLINE_SURFACE ( (
 ( 1.000000000000000000, 1.000000000000000000),
 ( 0.9934239774497838349, 0.8357310067453913582),
 ( 0.9934239774497838349, 0.8357310067453913582),
 ( 1.000000000000000000, 1.000000000000000000) ) ) 
 REPRESENTATION_ITEM ( '' )  SURFACE ( )  );
#22575 = CARTESIAN_POINT ( 'NONE',  ( 2.433796855181219243, 28.83182736670734059, -142.6247129145645829 ) ) ;
#22576 = CARTESIAN_POINT ( 'NONE',  ( 25.64700659047696263, 110.3963107228936309, 23.69811251893771242 ) ) ;
#22577 = ORIENTED_EDGE ( 'NONE', *, *, #7766, .F. ) ;
#22578 = CARTESIAN_POINT ( 'NONE',  ( 9.884929003653608603, 50.49804566712312237, -141.8132360130352936 ) ) ;
#22579 = CARTESIAN_POINT ( 'NONE',  ( 1.894214914920949289, -96.41356089048353795, 108.5033568857721491 ) ) ;
#22580 = CARTESIAN_POINT ( 'NONE',  ( 109.1586900883932856, -0.006561743627143346892, 0.002810909342011579538 ) ) ;
#22581 = ORIENTED_EDGE ( 'NONE', *, *, #19812, .F. ) ;
#22582 = AXIS2_PLACEMENT_3D ( 'NONE', #8734, #10900, #28297 ) ;
#22583 = ORIENTED_EDGE ( 'NONE', *, *, #8404, .T. ) ;
#22584 = CARTESIAN_POINT ( 'NONE',  ( -1.045287976400362417, 37.92705037016796155, 25.66401692419947977 ) ) ;
#22585 = CARTESIAN_POINT ( 'NONE',  ( 109.1587776205901861, 0.005390665547495581203, -0.004965871434398060232 ) ) ;
#22587 = CARTESIAN_POINT ( 'NONE',  ( -1.619063947482197729, -38.92136151114888776, 25.20140673341416360 ) ) ;
#22586 = CARTESIAN_POINT ( 'NONE',  ( 26.11404676487259024, 10.71016160607567080, 112.7148551500680753 ) ) ;
#22588 = CONICAL_SURFACE ( 'NONE', #2327, 117.6351876552689504, 0.9945805576725580410 ) ;
#22589 = B_SPLINE_CURVE_WITH_KNOTS ( 'NONE', 3,
 ( #3291, #10063, #20692, #9486 ),
 .UNSPECIFIED., .F., .F.,
 ( 4, 4 ),
 ( 0.000000000000000000, 0.01077107196513853692 ),
 .UNSPECIFIED. ) ;
#22590 = CARTESIAN_POINT ( 'NONE',  ( -7.733045908741315699, 52.15131830128827062, 5.980865481988326238 ) ) ;
#22591 = CARTESIAN_POINT ( 'NONE',  ( -1.045287976400386842, -28.14015102489780062, 36.12803364096639314 ) ) ;
#22592 = CARTESIAN_POINT ( 'NONE',  ( -12.82751273423883198, -35.32125660155422509, 33.78816682541326344 ) ) ;
#22593 = CARTESIAN_POINT ( 'NONE',  ( -8.786685647604720373, -47.14957014837338534, -25.35688121747513435 ) ) ;
#22594 = ORIENTED_EDGE ( 'NONE', *, *, #18829, .F. ) ;
#22595 = FACE_OUTER_BOUND ( 'NONE', #16766, .T. ) ;
#22596 = CARTESIAN_POINT ( 'NONE',  ( 109.1589550718175161, -0.005233222325307201363, -0.005477029346534909721 ) ) ;
#22597 = CONICAL_SURFACE ( 'NONE', #27172, 34.60786435723138510, 0.8559913436420825139 ) ;
#22598 = CARTESIAN_POINT ( 'NONE',  ( 25.64699802086725455, 12.03888878460473855, 112.2675771984164754 ) ) ;
#22599 = CARTESIAN_POINT ( 'NONE',  ( -25.21435515916043713, 15.02493970636190745, 31.17620025257570759 ) ) ;
#22600 = CARTESIAN_POINT ( 'NONE',  ( -25.21435515916025594, 1.749597353048488237E-16, -4.373993382621220594E-17 ) ) ;
#22601 = VERTEX_POINT ( 'NONE', #11385 ) ;
#22602 = DIRECTION ( 'NONE',  ( -1.000000000000000000, -0.000000000000000000, -0.000000000000000000 ) ) ;
#22603 = EDGE_CURVE ( 'NONE', #20657, #17799, #5006, .T. ) ;
#22604 = CARTESIAN_POINT ( 'NONE',  ( -24.53239521893651087, 6.738460611583212412, 33.25736993155762633 ) ) ;
#22605 = CARTESIAN_POINT ( 'NONE',  ( 14.74894986621300319, 4.541450660883840889E-15, -37.50000000000001421 ) ) ;
#22606 = ORIENTED_EDGE ( 'NONE', *, *, #24190, .F. ) ;
#22607 = EDGE_CURVE ( 'NONE', #26713, #6333, #20458, .T. ) ;
#22608 = ORIENTED_EDGE ( 'NONE', *, *, #23105, .T. ) ;
#22609 = EDGE_LOOP ( 'NONE', ( #2757, #19396, #4514, #19464 ) ) ;
#22610 = EDGE_CURVE ( 'NONE', #15531, #6453, #18994, .T. ) ;
#22611 = CIRCLE ( 'NONE', #1456, 53.53553390275978785 ) ;
#22612 = VECTOR ( 'NONE', #19346, 1000.000000000000114 ) ;
#22613 = CARTESIAN_POINT ( 'NONE',  ( -20.21097721712958517, 28.05863618200121934, 9.464413111084452268 ) ) ;
#22614 = EDGE_CURVE ( 'NONE', #16496, #27145, #138, .T. ) ;
#22615 = CARTESIAN_POINT ( 'NONE',  ( 1.833485406944043827, -132.3460930279887293, -59.50871042846357994 ) ) ;
#22616 = AXIS2_PLACEMENT_3D ( 'NONE', #20451, #13969, #22634 ) ;
#22617 = CARTESIAN_POINT ( 'NONE',  ( 1.831572820252009626, -108.4969585352548478, -96.36280042116040079 ) ) ;
#22618 = DIRECTION ( 'NONE',  ( 0.000000000000000000, 0.000000000000000000, 1.000000000000000000 ) ) ;
#22619 = ORIENTED_EDGE ( 'NONE', *, *, #12440, .F. ) ;
#22620 = CARTESIAN_POINT ( 'NONE',  ( -55.24390624410018802, 0.001811362924362862900, -0.01027195578988028025 ) ) ;
#22621 = CARTESIAN_POINT ( 'NONE',  ( 25.64700659047694131, 34.67498789830447947, 107.4550658295752470 ) ) ;
#22622 = DIRECTION ( 'NONE',  ( 0.000000000000000000, 0.000000000000000000, 1.000000000000000000 ) ) ;
#22623 = EDGE_LOOP ( 'NONE', ( #3306, #12422, #11430, #24834 ) ) ;
#22624 = EDGE_LOOP ( 'NONE', ( #22674, #23815, #12182, #9310 ) ) ;
#22625 = FACE_OUTER_BOUND ( 'NONE', #27323, .T. ) ;
#22626 = CARTESIAN_POINT ( 'NONE',  ( -1.619063947482197729, 2.489035965910801895, 46.30105812165545842 ) ) ;
#22627 = CARTESIAN_POINT ( 'NONE',  ( 1.834118845439484335, -144.3336252355296097, -14.99112450600394553 ) ) ;
#22628 = CARTESIAN_POINT ( 'NONE',  ( 13.36082413113063083, 151.2941478187910604, -22.28175172543404869 ) ) ;
#22629 = B_SPLINE_CURVE_WITH_KNOTS ( 'NONE', 3,
 ( #20111, #24883, #22579, #13633, #22731, #11475 ),
 .UNSPECIFIED., .F., .F.,
 ( 4, 2, 4 ),
 ( 0.000000000000000000, 0.0006311571484585993923, 0.001262314296917198785 ),
 .UNSPECIFIED. ) ;
#22630 = CARTESIAN_POINT ( 'NONE',  ( 2.430230287190581429, -107.1617224697457544, -98.44218333480878869 ) ) ;
#22631 = CARTESIAN_POINT ( 'NONE',  ( 32.73300124599735739, -16.10546300444903167, 116.5274707358854869 ) ) ;
#22632 = ORIENTED_EDGE ( 'NONE', *, *, #4443, .F. ) ;
#22633 = CARTESIAN_POINT ( 'NONE',  ( -1.031422197589716205, 12.69107518035502835, -44.01264471863851924 ) ) ;
#22634 = DIRECTION ( 'NONE',  ( 0.000000000000000000, 0.000000000000000000, 1.000000000000000000 ) ) ;
#22635 = CARTESIAN_POINT ( 'NONE',  ( -25.21435515916025594, 1.749597353048488237E-16, -4.373993382621220594E-17 ) ) ;
#22636 =( BOUNDED_SURFACE ( )  B_SPLINE_SURFACE ( 3, 1, ( 
 ( #9060, #4735 ),
 ( #7197, #17815 ),
 ( #18244, #24761 ),
 ( #13508, #26889 ) ),
 .UNSPECIFIED., .F., .F., .F. ) 
 B_SPLINE_SURFACE_WITH_KNOTS ( ( 4, 4 ),
 ( 2, 2 ),
 ( 0.000000000000000000, 1.000000000000000000 ),
 ( 0.000000000000000000, 1.000000000000000000 ),
 .UNSPECIFIED. ) 
 GEOMETRIC_REPRESENTATION_ITEM ( )  RATIONAL_B_SPLINE_SURFACE ( (
 ( 1.000000000000000000, 1.000000000000000000),
 ( 0.9956975270656954757, 0.8568959468854893125),
 ( 0.9956975270656954757, 0.8568959468854893125),
 ( 1.000000000000000000, 1.000000000000000000) ) ) 
 REPRESENTATION_ITEM ( '' )  SURFACE ( )  );
#22637 = CARTESIAN_POINT ( 'NONE',  ( 109.1624594426973260, -0.01358749486988124894, -0.008380433676406191107 ) ) ;
#22638 = CIRCLE ( 'NONE', #12501, 12.50000000000000178 ) ;
#22639 = EDGE_LOOP ( 'NONE', ( #11294, #27803, #2484, #5839 ) ) ;
#22640 = DIRECTION ( 'NONE',  ( 0.7071067811865465735, 2.453269466693394677E-16, -0.7071067811865485719 ) ) ;
#22641 = ORIENTED_EDGE ( 'NONE', *, *, #3936, .T. ) ;
#22642 = EDGE_CURVE ( 'NONE', #26863, #11014, #26614, .T. ) ;
#22643 = ORIENTED_EDGE ( 'NONE', *, *, #12391, .T. ) ;
#22644 = ORIENTED_EDGE ( 'NONE', *, *, #11695, .F. ) ;
#22645 = CARTESIAN_POINT ( 'NONE',  ( 25.64681081121880624, -102.9795863647025556, -46.30456157731431688 ) ) ;
#22646 = CARTESIAN_POINT ( 'NONE',  ( 2.430230287190572103, -31.67257033707601011, 142.0258656395020864 ) ) ;
#22647 = ADVANCED_FACE ( 'NONE', ( #19123 ), #625, .F. ) ;
#22648 = B_SPLINE_CURVE_WITH_KNOTS ( 'NONE', 3,
 ( #17099, #26712, #20093, #4418 ),
 .UNSPECIFIED., .F., .F.,
 ( 4, 4 ),
 ( 0.000000000000000000, 0.01077107196513880406 ),
 .UNSPECIFIED. ) ;
#22649 = CARTESIAN_POINT ( 'NONE',  ( -1.583189561560256253, -36.01941156322767057, 29.24830400313204493 ) ) ;
#22650 = CARTESIAN_POINT ( 'NONE',  ( 26.28373643307406482, 48.05579805965698625, -118.1623717393430582 ) ) ;
#22651 = CIRCLE ( 'NONE', #104, 151.1787379149930359 ) ;
#22652 = UNCERTAINTY_MEASURE_WITH_UNIT (LENGTH_MEASURE( 1.000000000000000082E-05 ), #24161, 'distance_accuracy_value', 'NONE');
#22653 = CARTESIAN_POINT ( 'NONE',  ( -1.619063947482197729, -16.67502769180532596, 43.26576862488450104 ) ) ;
#22654 = CARTESIAN_POINT ( 'NONE',  ( 32.73300124599738581, -62.10906484417165530, -99.90245962373897726 ) ) ;
#22655 = VECTOR ( 'NONE', #11331, 1000.000000000000114 ) ;
#22656 = AXIS2_PLACEMENT_3D ( 'NONE', #10160, #7866, #23264 ) ;
#22657 = CARTESIAN_POINT ( 'NONE',  ( -20.20700224038492721, -28.44216453106531617, 8.199606986804630182 ) ) ;
#22658 = CARTESIAN_POINT ( 'NONE',  ( 32.73300124599738581, 84.80615050150476009, -81.52272205837115848 ) ) ;
#22659 = FACE_OUTER_BOUND ( 'NONE', #27488, .T. ) ;
#22660 = B_SPLINE_CURVE_WITH_KNOTS ( 'NONE', 3,
 ( #2574, #19707, #9363, #11220, #13361, #26469, #10942 ),
 .UNSPECIFIED., .F., .F.,
 ( 4, 3, 4 ),
 ( 1.734723475976807094E-18, 0.009512539173626382780, 0.02506242213020817150 ),
 .UNSPECIFIED. ) ;
#22661 = CARTESIAN_POINT ( 'NONE',  ( 1.833485406944057594, -85.72460230293616235, -117.0814567582553281 ) ) ;
#22662 = CARTESIAN_POINT ( 'NONE',  ( 10.93730112725990011, -119.3442956573265974, -92.80059208661810999 ) ) ;
#22663 = CARTESIAN_POINT ( 'NONE',  ( -1.044556982611280382, -25.56989963842174873, 37.98985389331836870 ) ) ;
#22664 = LINE ( 'NONE', #20764, #6427 ) ;
#22665 = CARTESIAN_POINT ( 'NONE',  ( 25.98552792386801968, -22.46612985365048232, 110.8838436908325917 ) ) ;
#22666 = CARTESIAN_POINT ( 'NONE',  ( -1.048996300304502194, -36.59642367107725391, 27.53442103413733122 ) ) ;
#22667 = CARTESIAN_POINT ( 'NONE',  ( 109.1778270068192853, -0.006489198140359578836, -0.006682187084648886881 ) ) ;
#22668 = CARTESIAN_POINT ( 'NONE',  ( 25.64692872815575342, 84.12425003484143815, -75.31297890941186779 ) ) ;
#22669 = ORIENTED_EDGE ( 'NONE', *, *, #6536, .F. ) ;
#22670 =( BOUNDED_SURFACE ( )  B_SPLINE_SURFACE ( 3, 1, ( 
 ( #5046, #11961 ),
 ( #3049, #3468 ),
 ( #22783, #20887 ),
 ( #27355, #9819 ) ),
 .UNSPECIFIED., .F., .F., .F. ) 
 B_SPLINE_SURFACE_WITH_KNOTS ( ( 4, 4 ),
 ( 2, 2 ),
 ( 0.000000000000000000, 1.000000000000000000 ),
 ( 0.000000000000000000, 1.000000000000000000 ),
 .UNSPECIFIED. ) 
 GEOMETRIC_REPRESENTATION_ITEM ( )  RATIONAL_B_SPLINE_SURFACE ( (
 ( 1.000000000000000000, 1.000000000000000000),
 ( 0.9956975270656955868, 0.8568959468854907557),
 ( 0.9956975270656955868, 0.8568959468854907557),
 ( 1.000000000000000000, 1.000000000000000000) ) ) 
 REPRESENTATION_ITEM ( '' )  SURFACE ( )  );
#22671 = VERTEX_POINT ( 'NONE', #27604 ) ;
#22672 = CARTESIAN_POINT ( 'NONE',  ( -5.986830583229483693, -19.95149887249887399, -46.64941882410793283 ) ) ;
#22673 = CARTESIAN_POINT ( 'NONE',  ( 26.11404676487259024, 12.95861723607453619, 112.4785329405482628 ) ) ;
#22674 = ORIENTED_EDGE ( 'NONE', *, *, #9336, .F. ) ;
#22675 = ADVANCED_FACE ( 'NONE', ( #25745 ), #19197, .F. ) ;
#22676 = CIRCLE ( 'NONE', #17583, 34.60786435723138510 ) ;
#22677 = ORIENTED_EDGE ( 'NONE', *, *, #8029, .F. ) ;
#22678 = AXIS2_PLACEMENT_3D ( 'NONE', #13112, #10960, #2025 ) ;
#22679 = EDGE_LOOP ( 'NONE', ( #26473, #2785 ) ) ;
#22680 = EDGE_CURVE ( 'NONE', #21489, #20545, #9930, .T. ) ;
#22681 = EDGE_CURVE ( 'NONE', #2573, #3393, #17695, .T. ) ;
#22682 = CARTESIAN_POINT ( 'NONE',  ( 1.832998868059858122, 59.50898020732689986, -132.3466930259787944 ) ) ;
#22683 = EDGE_CURVE ( 'NONE', #14104, #10838, #10183, .T. ) ;
#22684 = CARTESIAN_POINT ( 'NONE',  ( -55.25719721206881729, -0.004044147484874425005, 0.01041086141212271658 ) ) ;
#22685 = VECTOR ( 'NONE', #19198, 1000.000000000000000 ) ;
#22686 = CARTESIAN_POINT ( 'NONE',  ( -1.048994561756786625, -13.42228657661154401, -43.78680886990936472 ) ) ;
#22687 = CARTESIAN_POINT ( 'NONE',  ( 25.64692872815577473, -66.62748454953222677, 91.15762468787718831 ) ) ;
#22688 = CARTESIAN_POINT ( 'NONE',  ( 2.433796855181219243, 107.1581411821798895, -98.43889364293755762 ) ) ;
#22689 = CARTESIAN_POINT ( 'NONE',  ( 32.73300124599740002, 97.37344512919945316, -66.00340565729239017 ) ) ;
#22690 = CARTESIAN_POINT ( 'NONE',  ( -55.24300891470648622, 0.002702093572889911754, 0.009439835024157509913 ) ) ;
#22691 = DIRECTION ( 'NONE',  ( 0.000000000000000000, 0.000000000000000000, 1.000000000000000000 ) ) ;
#22692 = CARTESIAN_POINT ( 'NONE',  ( 8.186469777910573953, 137.8131828745823952, 57.56191611950351472 ) ) ;
#22693 = CARTESIAN_POINT ( 'NONE',  ( -1.050229599974477734, 27.12684363859256109, -36.90196321294305193 ) ) ;
#22694 = CARTESIAN_POINT ( 'NONE',  ( 25.73574536432415627, 83.41179791497867768, 76.18908113044783192 ) ) ;
#22695 = VECTOR ( 'NONE', #15970, 1000.000000000000000 ) ;
#22696 = ORIENTED_EDGE ( 'NONE', *, *, #27190, .T. ) ;
#22697 = EDGE_LOOP ( 'NONE', ( #20430, #9769, #633, #5633 ) ) ;
#22698 = CARTESIAN_POINT ( 'NONE',  ( 28.37603512858359522, 13.77584568114293617, 113.9023475466375288 ) ) ;
#22700 = CARTESIAN_POINT ( 'NONE',  ( -1.463510566862821660, 25.15876608740871490, 38.76366072687751796 ) ) ;
#22699 = CARTESIAN_POINT ( 'NONE',  ( 1.833485406944043827, -15.69895494453482598, 144.2578170162062463 ) ) ;
#22701 = CARTESIAN_POINT ( 'NONE',  ( 25.70243777736186885, -84.42566495012501093, 75.03063812272023370 ) ) ;
#22702 = DIRECTION ( 'NONE',  ( 0.000000000000000000, 0.000000000000000000, 1.000000000000000000 ) ) ;
#22703 = CARTESIAN_POINT ( 'NONE',  ( -22.23342874802668589, 24.24669006619402367, 20.31166691703097982 ) ) ;
#22704 = EDGE_CURVE ( 'NONE', #19926, #11082, #887, .T. ) ;
#22705 = EDGE_LOOP ( 'NONE', ( #25893, #15266, #5652, #488 ) ) ;
#22706 = CARTESIAN_POINT ( 'NONE',  ( 28.43349137099853863, 124.1860347533531979, -4.052139611198855462 ) ) ;
#22707 = CARTESIAN_POINT ( 'NONE',  ( -21.41427618760457463, 16.60878262545457318, 25.94789270595488517 ) ) ;
#22708 = CARTESIAN_POINT ( 'NONE',  ( 30.58324630866349025, 74.24222250960228564, 95.47492154584176660 ) ) ;
#22709 = ORIENTED_EDGE ( 'NONE', *, *, #11863, .F. ) ;
#22710 = CARTESIAN_POINT ( 'NONE',  ( -9.156249394959713683, 9.022661520477768704, -53.74753343182706544 ) ) ;
#22712 = ORIENTED_EDGE ( 'NONE', *, *, #2518, .F. ) ;
#22711 = EDGE_CURVE ( 'NONE', #22316, #23136, #25633, .T. ) ;
#22713 = CARTESIAN_POINT ( 'NONE',  ( 1.832998868059858122, -125.4013017422225857, -73.01698022778488451 ) ) ;
#22714 = CARTESIAN_POINT ( 'NONE',  ( -9.156249394959706578, -38.17928057391962682, 38.89149400288449243 ) ) ;
#22715 = CARTESIAN_POINT ( 'NONE',  ( 30.59141879584292667, -66.10404588653725000, -95.58042137919522929 ) ) ;
#22716 =( BOUNDED_SURFACE ( )  B_SPLINE_SURFACE ( 3, 1, ( 
 ( #16295, #7685 ),
 ( #27219, #25090 ),
 ( #9678, #13845 ),
 ( #11981, #20468 ) ),
 .UNSPECIFIED., .F., .F., .F. ) 
 B_SPLINE_SURFACE_WITH_KNOTS ( ( 4, 4 ),
 ( 2, 2 ),
 ( 0.000000000000000000, 1.000000000000000000 ),
 ( 0.000000000000000000, 1.000000000000000000 ),
 .UNSPECIFIED. ) 
 GEOMETRIC_REPRESENTATION_ITEM ( )  RATIONAL_B_SPLINE_SURFACE ( (
 ( 1.000000000000000000, 1.000000000000000000),
 ( 0.6386103224230316178, 0.9954351624131538845),
 ( 0.6386103224230316178, 0.9954351624131538845),
 ( 1.000000000000000000, 1.000000000000000000) ) ) 
 REPRESENTATION_ITEM ( '' )  SURFACE ( )  );
#22717 = ORIENTED_EDGE ( 'NONE', *, *, #13903, .T. ) ;
#22718 = CARTESIAN_POINT ( 'NONE',  ( -20.37983603106074426, -27.81368274044719868, -10.62371319148630455 ) ) ;
#22719 = VERTEX_POINT ( 'NONE', #16534 ) ;
#22720 = CARTESIAN_POINT ( 'NONE',  ( -23.79248802219730052, -30.42578156345377849, 13.25839849636389367 ) ) ;
#22721 = ORIENTED_EDGE ( 'NONE', *, *, #20276, .F. ) ;
#22722 = DIRECTION ( 'NONE',  ( 1.333107886233864114E-15, -0.1349691616810116124, 0.9908497996140105402 ) ) ;
#22723 = B_SPLINE_CURVE_WITH_KNOTS ( 'NONE', 3,
 ( #22389, #15753, #18190, #4825, #20206, #4678 ),
 .UNSPECIFIED., .F., .F.,
 ( 4, 2, 4 ),
 ( 1.474514954580286030E-17, 0.0006311636237757010286, 0.001262327247551387095 ),
 .UNSPECIFIED. ) ;
#22724 = B_SPLINE_CURVE_WITH_KNOTS ( 'NONE', 3,
 ( #8736, #4271, #23604, #2674, #15341, #20087, #4843, #21975, #18210, #9453 ),
 .UNSPECIFIED., .F., .F.,
 ( 4, 3, 3, 4 ),
 ( 1.962615573354718958E-17, 0.0002669560319015498121, 0.0005492286108966249738, 0.0008315040496093325378 ),
 .UNSPECIFIED. ) ;
#22725 = CARTESIAN_POINT ( 'NONE',  ( 21.16825799904893657, -103.5479404090030897, -87.29264348877946134 ) ) ;
#22726 = FACE_OUTER_BOUND ( 'NONE', #12046, .T. ) ;
#22727 = CARTESIAN_POINT ( 'NONE',  ( -1.019300379054419725, -25.26451264419615939, 38.21680004809191189 ) ) ;
#22728 = CARTESIAN_POINT ( 'NONE',  ( 1.833691583653537460, -125.8462703805704166, 72.24637705290446377 ) ) ;
#22729 = ORIENTED_EDGE ( 'NONE', *, *, #3156, .F. ) ;
#22730 = CARTESIAN_POINT ( 'NONE',  ( 10.93730112725972248, -36.23586118136624634, 146.7718404940640653 ) ) ;
#22731 = CARTESIAN_POINT ( 'NONE',  ( 2.263178607246683516, -96.24282447295516363, 108.9830946142710530 ) ) ;
#22732 = CARTESIAN_POINT ( 'NONE',  ( 32.73300124599735739, -16.10546300444903167, 116.5274707358854869 ) ) ;
#22733 = ORIENTED_EDGE ( 'NONE', *, *, #19949, .F. ) ;
#22734 = ORIENTED_EDGE ( 'NONE', *, *, #24487, .T. ) ;
#22735 = ORIENTED_EDGE ( 'NONE', *, *, #20012, .F. ) ;
#22736 = CARTESIAN_POINT ( 'NONE',  ( -1.048996300304502194, 37.49570739463922564, 26.29666317565261124 ) ) ;
#22737 = CARTESIAN_POINT ( 'NONE',  ( -9.156249394959706578, -48.32878616080991208, 25.18996226954667605 ) ) ;
#22739 = CARTESIAN_POINT ( 'NONE',  ( 10.93730112726007775, 51.37919228020501805, -142.1801301103781725 ) ) ;
#22738 = FACE_OUTER_BOUND ( 'NONE', #15044, .T. ) ;
#22740 = CARTESIAN_POINT ( 'NONE',  ( -8.786685647604706162, -38.68584556812290032, 37.00619870957955015 ) ) ;
#22741 = CARTESIAN_POINT ( 'NONE',  ( 1.833809397773869865, 144.2961330457379177, 15.34508223002496941 ) ) ;
#22742 = CARTESIAN_POINT ( 'NONE',  ( 1.833485406944057594, 72.09189602597886903, -125.9346397303427665 ) ) ;
#22743 = CARTESIAN_POINT ( 'NONE',  ( -1.113548883309548376, -28.52482525634917820, 35.91246368318234516 ) ) ;
#22744 = EDGE_CURVE ( 'NONE', #12412, #4347, #6057, .T. ) ;
#22745 = ORIENTED_EDGE ( 'NONE', *, *, #10538, .T. ) ;
#22746 = CARTESIAN_POINT ( 'NONE',  ( -25.21435515916043713, -25.00736669481004526, 23.92354251275963861 ) ) ;
#22747 = CARTESIAN_POINT ( 'NONE',  ( 32.73300124599735028, -8.473903470906931190, 117.3295799645429156 ) ) ;
#22748 = CARTESIAN_POINT ( 'NONE',  ( 25.64681081121880624, 11.38886654529674303, 112.3352186517031157 ) ) ;
#22749 = CARTESIAN_POINT ( 'NONE',  ( 109.1586900883932856, -0.005236795036860577776, 0.004851151255037344269 ) ) ;
#22750 = EDGE_CURVE ( 'NONE', #12091, #24050, #25260, .T. ) ;
#22751 = CARTESIAN_POINT ( 'NONE',  ( 32.73300124599741423, -97.37344512919810313, -66.00340565729437969 ) ) ;
#22753 = CARTESIAN_POINT ( 'NONE',  ( 109.1592201516379674, 0.004368284148529012062, 0.006536841731953418715 ) ) ;
#22752 = B_SPLINE_CURVE_WITH_KNOTS ( 'NONE', 3,
 ( #7856, #14154, #26868, #5388, #5688, #23259, #22428 ),
 .UNSPECIFIED., .F., .F.,
 ( 4, 3, 4 ),
 ( 0.000000000000000000, 0.02398743853561347353, 0.04000277880656219476 ),
 .UNSPECIFIED. ) ;
#22754 = ORIENTED_EDGE ( 'NONE', *, *, #18333, .F. ) ;
#22755 = CARTESIAN_POINT ( 'NONE',  ( 109.1778270068192853, -0.008360410075186638576, -0.004106684808172209912 ) ) ;
#22756 = CARTESIAN_POINT ( 'NONE',  ( -10.86508079875781085, 50.32133009257468359, -9.118642906269416315 ) ) ;
#22757 = CARTESIAN_POINT ( 'NONE',  ( -55.25719721206881729, 0.008651607285661618019, -0.007063345920781386421 ) ) ;
#22758 = ORIENTED_EDGE ( 'NONE', *, *, #27490, .F. ) ;
#22759 = ORIENTED_EDGE ( 'NONE', *, *, #26538, .F. ) ;
#22760 = ORIENTED_EDGE ( 'NONE', *, *, #5328, .T. ) ;
#22761 =( BOUNDED_SURFACE ( )  B_SPLINE_SURFACE ( 3, 1, ( 
 ( #27824, #23383 ),
 ( #19050, #18907 ),
 ( #12694, #16892 ),
 ( #21342, #27534 ) ),
 .UNSPECIFIED., .F., .F., .F. ) 
 B_SPLINE_SURFACE_WITH_KNOTS ( ( 4, 4 ),
 ( 2, 2 ),
 ( 0.000000000000000000, 1.000000000000000000 ),
 ( 0.000000000000000000, 1.000000000000000000 ),
 .UNSPECIFIED. ) 
 GEOMETRIC_REPRESENTATION_ITEM ( )  RATIONAL_B_SPLINE_SURFACE ( (
 ( 1.000000000000000000, 1.000000000000000000),
 ( 0.7789835883360576307, 0.9689951854195403280),
 ( 0.7789835883360576307, 0.9689951854195403280),
 ( 1.000000000000000000, 1.000000000000000000) ) ) 
 REPRESENTATION_ITEM ( '' )  SURFACE ( )  );
#22762 = DIRECTION ( 'NONE',  ( 0.000000000000000000, 5.223019709708233256E-21, -1.000000000000000000 ) ) ;
#22763 = CARTESIAN_POINT ( 'NONE',  ( 6.224689322667630975, 108.2965163446074399, 100.9623537450655419 ) ) ;
#22764 = CARTESIAN_POINT ( 'NONE',  ( -55.24340739397742084, 0.005344433640973447058, 0.008612749836246493332 ) ) ;
#22765 = CARTESIAN_POINT ( 'NONE',  ( -23.77929240705205416, 15.74261278740719128, 32.66578242509729790 ) ) ;
#22766 = CARTESIAN_POINT ( 'NONE',  ( 2.433796855181205476, 107.1581411821785821, 98.43889364293895028 ) ) ;
#22767 = ORIENTED_EDGE ( 'NONE', *, *, #23837, .T. ) ;
#22768 = CARTESIAN_POINT ( 'NONE',  ( -15.02187109954780553, 33.49412687891621232, 32.04062513125082035 ) ) ;
#22769 = CARTESIAN_POINT ( 'NONE',  ( 109.1589550718174877, -0.002553077953671659388, 0.007132058561965940943 ) ) ;
#22770 = CARTESIAN_POINT ( 'NONE',  ( 25.98552792386802679, -45.02923844025552569, 103.7897946223263830 ) ) ;
#22771 = ORIENTED_EDGE ( 'NONE', *, *, #25670, .T. ) ;
#22772 = EDGE_CURVE ( 'NONE', #1034, #18134, #1893, .T. ) ;
#22773 = ORIENTED_EDGE ( 'NONE', *, *, #15120, .T. ) ;
#22774 = CARTESIAN_POINT ( 'NONE',  ( -55.25297051322618813, 0.007247191603132027878, 0.01306918787467585205 ) ) ;
#22775 = ADVANCED_FACE ( 'NONE', ( #1965 ), #18044, .T. ) ;
#22776 = CARTESIAN_POINT ( 'NONE',  ( -24.53237795827031320, 33.25734978085278470, 6.738475012719742807 ) ) ;
#22777 = CARTESIAN_POINT ( 'NONE',  ( -8.786685647604887350, 53.04920435127183254, 7.199674155859139724 ) ) ;
#22778 = CARTESIAN_POINT ( 'NONE',  ( 32.73300124599732186, 0.000000000000000000, 0.000000000000000000 ) ) ;
#22779 = CARTESIAN_POINT ( 'NONE',  ( 2.063896406836605024, -107.0521644432410682, -98.19887492195967127 ) ) ;
#22780 = CARTESIAN_POINT ( 'NONE',  ( -1.048996300304514850, -45.79145529752467070, 0.7649764263856586588 ) ) ;
#22781 = ORIENTED_EDGE ( 'NONE', *, *, #3039, .T. ) ;
#22782 = CARTESIAN_POINT ( 'NONE',  ( -8.786685647604885574, 6.096987947571466530E-17, -1.524246986892866633E-17 ) ) ;
#22783 = CARTESIAN_POINT ( 'NONE',  ( 109.1589550718175161, 0.007507020724820355310, -0.001014448720249569230 ) ) ;
#22784 = EDGE_CURVE ( 'NONE', #1034, #15045, #11038, .T. ) ;
#22785 = CARTESIAN_POINT ( 'NONE',  ( -2.265401668238145483, -36.42007794497270368, -29.73100299756553966 ) ) ;
#22786 = FACE_OUTER_BOUND ( 'NONE', #12063, .T. ) ;
#22787 = CARTESIAN_POINT ( 'NONE',  ( 25.64708228042119131, -107.3971738194634185, 34.85404436489458391 ) ) ;
#22788 = EDGE_CURVE ( 'NONE', #11885, #8709, #18671, .T. ) ;
#22789 = ORIENTED_EDGE ( 'NONE', *, *, #3029, .T. ) ;
#22790 = CARTESIAN_POINT ( 'NONE',  ( -1.583189561560253589, -11.94859433442870866, 44.83405390829683057 ) ) ;
#22791 = ORIENTED_EDGE ( 'NONE', *, *, #5462, .T. ) ;
#22792 = ORIENTED_EDGE ( 'NONE', *, *, #10522, .T. ) ;
#22793 = VECTOR ( 'NONE', #21986, 1000.000000000000227 ) ;
#22794 = ORIENTED_EDGE ( 'NONE', *, *, #21782, .F. ) ;
#22795 = CARTESIAN_POINT ( 'NONE',  ( 0.000000000000000000, 0.000000000000000000, 0.000000000000000000 ) ) ;
#22796 = CARTESIAN_POINT ( 'NONE',  ( 2.063896406836609909, 125.1295119249449499, -73.79559738457622586 ) ) ;
#22797 = CARTESIAN_POINT ( 'NONE',  ( -10.86508079875774158, -50.67624451685647102, -6.877801422380581009 ) ) ;
#22798 = CARTESIAN_POINT ( 'NONE',  ( -4.162674018437144241, 25.90909455705170217, 41.48630000627025538 ) ) ;
#22799 = CARTESIAN_POINT ( 'NONE',  ( -18.41936578851717599, 5.707900577128148356, -42.05131332928112187 ) ) ;
#22800 = CARTESIAN_POINT ( 'NONE',  ( 25.64660436782552821, -75.12017330820535221, 84.29628170537232279 ) ) ;
#22801 = CARTESIAN_POINT ( 'NONE',  ( 25.73574536432416338, 107.6875787074511521, -34.14219540448021206 ) ) ;
#22802 = EDGE_CURVE ( 'NONE', #8105, #6339, #8876, .T. ) ;
#22803 = FACE_OUTER_BOUND ( 'NONE', #4260, .T. ) ;
#22804 = CARTESIAN_POINT ( 'NONE',  ( 5.340103556456505807, -139.5040934094288332, -47.74933482044516353 ) ) ;
#22805 = CARTESIAN_POINT ( 'NONE',  ( -20.20700224038492721, -28.44216453106531617, 8.199606986804630182 ) ) ;
#22806 = LINE ( 'NONE', #3074, #23875 ) ;
#22807 = EDGE_CURVE ( 'NONE', #11372, #18716, #13460, .T. ) ;
#22809 = CARTESIAN_POINT ( 'NONE',  ( 28.43349137099837876, -21.85613782299062180, 122.3147591366315510 ) ) ;
#22808 = CARTESIAN_POINT ( 'NONE',  ( 99.22246935314075245, -70.00000000000000000, 40.00000000000003553 ) ) ;
#22810 =( REPRESENTATION_RELATIONSHIP ('NONE','NONE', #15430, #747 ) REPRESENTATION_RELATIONSHIP_WITH_TRANSFORMATION ( #3833 )SHAPE_REPRESENTATION_RELATIONSHIP( ) );
#22811 = FACE_OUTER_BOUND ( 'NONE', #7272, .T. ) ;
#22812 = CARTESIAN_POINT ( 'NONE',  ( -1.049819825607596124, -36.75053263699369666, 27.33096219556280815 ) ) ;
#22813 = CARTESIAN_POINT ( 'NONE',  ( 32.73300124599735028, 66.00340565729339914, 97.37344512919882789 ) ) ;
#22814 = CARTESIAN_POINT ( 'NONE',  ( 10.93730112725983439, -146.7718404940644916, 36.23586118136483236 ) ) ;
#22815 = EDGE_LOOP ( 'NONE', ( #7517, #2433, #22377, #24398 ) ) ;
#22816 = CARTESIAN_POINT ( 'NONE',  ( 21.16825799904907868, 32.46271504707934241, 131.4851843440076209 ) ) ;
#22817 = ORIENTED_EDGE ( 'NONE', *, *, #26959, .T. ) ;
#22818 = CARTESIAN_POINT ( 'NONE',  ( 1.894214914920929749, -16.12044375672191165, -144.2521558665609973 ) ) ;
#22819 = CARTESIAN_POINT ( 'NONE',  ( 25.81918753295380142, 12.74259626488151476, 112.3053965977761663 ) ) ;
#22820 = ORIENTED_EDGE ( 'NONE', *, *, #10563, .F. ) ;
#22821 = ORIENTED_EDGE ( 'NONE', *, *, #8677, .T. ) ;
#22822 = EDGE_LOOP ( 'NONE', ( #10745, #9454, #5118, #2890 ) ) ;
#22823 = B_SPLINE_CURVE_WITH_KNOTS ( 'NONE', 3,
 ( #22586, #20408, #832, #7913 ),
 .UNSPECIFIED., .F., .F.,
 ( 4, 4 ),
 ( 1.055191096010040543E-17, 0.008383560773332703400 ),
 .UNSPECIFIED. ) ;
#22824 = B_SPLINE_CURVE_WITH_KNOTS ( 'NONE', 3,
 ( #9516, #22332, #7356, #20445, #22776, #24651 ),
 .UNSPECIFIED., .F., .F.,
 ( 4, 2, 4 ),
 ( 0.000000000000000000, 0.003570751334075638293, 0.007141502668151268780 ),
 .UNSPECIFIED. ) ;
#22825 = DIRECTION ( 'NONE',  ( 0.000000000000000000, 5.223019709708233256E-21, -1.000000000000000000 ) ) ;
#22826 = CARTESIAN_POINT ( 'NONE',  ( 55.49584447822657296, 72.18163437663950788, -7.317474139114888310 ) ) ;
#22827 = CARTESIAN_POINT ( 'NONE',  ( 109.1587776205901861, 0.005978137617721842115, 0.004240403845331894121 ) ) ;
#22828 = CARTESIAN_POINT ( 'NONE',  ( 1.833838850093452821, 144.3148362521194485, -15.16810397409632927 ) ) ;
#22829 = CARTESIAN_POINT ( 'NONE',  ( 1.833838850093440165, 30.17001957361989994, 141.9387658801232703 ) ) ;
#22830 = CARTESIAN_POINT ( 'NONE',  ( 26.11404676487259024, -97.48350837663652158, 57.58742681967414256 ) ) ;
#22831 = CARTESIAN_POINT ( 'NONE',  ( 109.1592201516379674, -0.0005146241775907877628, 0.007845213074660000591 ) ) ;
#22832 = CARTESIAN_POINT ( 'NONE',  ( 2.433796855181233454, 13.76554153471886366, -144.8571464219887730 ) ) ;
#22833 = EDGE_CURVE ( 'NONE', #3159, #182, #11180, .T. ) ;
#22834 = CARTESIAN_POINT ( 'NONE',  ( 1.834118845439484335, 59.18411796427052707, 132.4921483272730143 ) ) ;
#22836 = CARTESIAN_POINT ( 'NONE',  ( 13.36082413113061307, -137.0038452127796234, -67.94366799842953242 ) ) ;
#22835 = CARTESIAN_POINT ( 'NONE',  ( -55.25297051322618813, 0.002853887643042873987, -0.01466904165775150676 ) ) ;
#22837 = DIRECTION ( 'NONE',  ( 0.000000000000000000, 0.000000000000000000, 1.000000000000000000 ) ) ;
#22839 = ORIENTED_EDGE ( 'NONE', *, *, #26274, .F. ) ;
#22838 = EDGE_CURVE ( 'NONE', #9163, #25441, #7367, .T. ) ;
#22840 = ORIENTED_EDGE ( 'NONE', *, *, #1774, .T. ) ;
#22841 = CARTESIAN_POINT ( 'NONE',  ( 109.1592201516379674, -0.006174480289199440856, 0.004867031887019522031 ) ) ;
#22843 = CARTESIAN_POINT ( 'NONE',  ( -20.57838717382308147, 7.715628353033680220, -28.96176188950220975 ) ) ;
#22842 = LINE ( 'NONE', #656, #1032 ) ;
#22844 = EDGE_CURVE ( 'NONE', #2065, #7617, #4953, .T. ) ;
#22845 = CARTESIAN_POINT ( 'NONE',  ( 10.93730112725978287, -97.44200844886353252, 115.5857507957700250 ) ) ;
#22846 = DIRECTION ( 'NONE',  ( 0.000000000000000000, 0.000000000000000000, 1.000000000000000000 ) ) ;
#22847 = CARTESIAN_POINT ( 'NONE',  ( -1.323830074806774837, -35.86387698262934265, -28.92190886481852274 ) ) ;
#22848 = EDGE_LOOP ( 'NONE', ( #5876, #23055, #14645, #8028 ) ) ;
#22849 = CARTESIAN_POINT ( 'NONE',  ( 55.79472521941428198, -6.880567342320201618, 72.42790650415570042 ) ) ;
#22850 = CARTESIAN_POINT ( 'NONE',  ( -1.058197053496162665, 45.77356582045591438, 1.754224732379708662 ) ) ;
#22851 = CARTESIAN_POINT ( 'NONE',  ( -1.583189561560252701, 43.29471907393764951, 16.68617981233657943 ) ) ;
#22852 = ORIENTED_EDGE ( 'NONE', *, *, #15477, .F. ) ;
#22853 = FACE_OUTER_BOUND ( 'NONE', #24367, .T. ) ;
#22854 = CARTESIAN_POINT ( 'NONE',  ( 2.433796855181205476, -132.3327394885227477, -60.50726454508036056 ) ) ;
#22855 = B_SPLINE_CURVE_WITH_KNOTS ( 'NONE', 3,
 ( #16239, #409, #840, #7478 ),
 .UNSPECIFIED., .F., .F.,
 ( 4, 4 ),
 ( 1.906343156168368086E-16, 0.001982023823822943315 ),
 .UNSPECIFIED. ) ;
#22856 = CARTESIAN_POINT ( 'NONE',  ( -55.24390624410018802, -0.001811362924359030029, -0.01027195578987783083 ) ) ;
#22857 = CARTESIAN_POINT ( 'NONE',  ( 32.73300124599739291, -66.00340565729273123, -97.37344512919924000 ) ) ;
#22858 = ORIENTED_EDGE ( 'NONE', *, *, #25536, .T. ) ;
#22859 = DIRECTION ( 'NONE',  ( 0.5914120900931444380, -0.7693434820005567998, 0.2415416038592884396 ) ) ;
#22860 = ORIENTED_EDGE ( 'NONE', *, *, #26478, .F. ) ;
#22861 = CARTESIAN_POINT ( 'NONE',  ( 25.64670758986456534, -45.46974729533215509, -103.3508631837548677 ) ) ;
#22862 = CARTESIAN_POINT ( 'NONE',  ( 28.37599760073042177, 1.794331790581030983, -114.7183216384031113 ) ) ;
#22863 = ORIENTED_EDGE ( 'NONE', *, *, #7736, .T. ) ;
#22864 =( NAMED_UNIT ( * ) PLANE_ANGLE_UNIT ( ) SI_UNIT ( $, .RADIAN. ) );
#22865 = ADVANCED_FACE ( 'NONE', ( #17785 ), #1712, .F. ) ;
#22866 = CARTESIAN_POINT ( 'NONE',  ( 26.11404676487257603, 98.61392875273364211, 55.62948129436280453 ) ) ;
#22867 = CARTESIAN_POINT ( 'NONE',  ( 109.1586900883932856, -0.006479576224398268976, 0.002995460350188374095 ) ) ;
#22868 = FACE_OUTER_BOUND ( 'NONE', #20683, .T. ) ;
#22869 = CARTESIAN_POINT ( 'NONE',  ( 26.11404676487257603, -113.2169081140374232, 1.130420376096734847 ) ) ;
#22870 = ADVANCED_FACE ( 'NONE', ( #12762 ), #3567, .F. ) ;
#22871 = ORIENTED_EDGE ( 'NONE', *, *, #9161, .F. ) ;
#22872 = EDGE_CURVE ( 'NONE', #19971, #20059, #9155, .T. ) ;
#22873 = CARTESIAN_POINT ( 'NONE',  ( -1.050229599974468409, -14.39582765040431944, 43.47850826583067629 ) ) ;
#22875 = CARTESIAN_POINT ( 'NONE',  ( 109.1721716018069657, 0.01706748904932341507, -0.0002019688922673717113 ) ) ;
#22874 = CARTESIAN_POINT ( 'NONE',  ( -20.57838717382308147, 29.92853265176831812, 1.611677988432465014 ) ) ;
#22876 = CARTESIAN_POINT ( 'NONE',  ( -8.786685647604890903, -37.00619870957961410, -38.68584556812286479 ) ) ;
#22877 = ORIENTED_EDGE ( 'NONE', *, *, #3384, .T. ) ;
#22878 = ORIENTED_EDGE ( 'NONE', *, *, #19595, .T. ) ;
#22879 = ORIENTED_EDGE ( 'NONE', *, *, #20035, .F. ) ;
#22880 = CARTESIAN_POINT ( 'NONE',  ( -1.049817751779888786, 36.75003908324330837, 27.33161971822157810 ) ) ;
#22881 = CARTESIAN_POINT ( 'NONE',  ( -55.24300891470650754, 0.007734635432136952211, -0.006048736206179535120 ) ) ;
#22883 = CARTESIAN_POINT ( 'NONE',  ( -23.79223135445718995, -7.157574570129374258, -32.40779366744832402 ) ) ;
#22882 = CARTESIAN_POINT ( 'NONE',  ( -16.86833981943424376, -43.82216161736207738, 5.948101187262031964 ) ) ;
#22884 = CARTESIAN_POINT ( 'NONE',  ( 28.37644542392841629, 46.84227702240779223, 115.1790646972551144 ) ) ;
#22885 = B_SPLINE_CURVE_WITH_KNOTS ( 'NONE', 3,
 ( #16378, #20974, #16824, #12071, #14355, #23022, #25173, #1402, #12209, #1260 ),
 .UNSPECIFIED., .F., .F.,
 ( 4, 3, 3, 4 ),
 ( 5.003707553108401214E-17, 0.0002669559177086214242, 0.0005339118354151109816, 0.001067817517169154708 ),
 .UNSPECIFIED. ) ;
#22886 = CARTESIAN_POINT ( 'NONE',  ( -1.031422197589711987, -12.69107518035471394, 44.01264471863858319 ) ) ;
#22887 = CARTESIAN_POINT ( 'NONE',  ( -1.056502255334264895, -27.33667001641194361, -36.75727364034722200 ) ) ;
#22888 = CARTESIAN_POINT ( 'NONE',  ( 25.64681081121879203, 46.30456157731467925, -102.9795863647023850 ) ) ;
#22889 = ORIENTED_EDGE ( 'NONE', *, *, #19086, .F. ) ;
#22890 = CARTESIAN_POINT ( 'NONE',  ( 8.186469829614440030, 122.8338389144559244, -84.95702201190418634 ) ) ;
#22891 = CARTESIAN_POINT ( 'NONE',  ( -4.780792508754314163, -32.07473752860752825, 37.74278713234433269 ) ) ;
#22892 = CARTESIAN_POINT ( 'NONE',  ( -20.24419206586953379, 28.55732805495827265, 7.929973069813099684 ) ) ;
#22893 = CARTESIAN_POINT ( 'NONE',  ( 5.340103556456469391, -135.6222865117685217, 57.86178752079269572 ) ) ;
#22894 = CARTESIAN_POINT ( 'NONE',  ( 28.37603512858451182, 111.8384105897145133, -25.60641750873795175 ) ) ;
#22895 = CARTESIAN_POINT ( 'NONE',  ( 28.37599760073041821, -104.0705811520810897, -48.29934869928272434 ) ) ;
#22896 = CARTESIAN_POINT ( 'NONE',  ( -28.13707043255157103, -18.06394523322463641, -14.07296284901326189 ) ) ;
#22897 =( BOUNDED_SURFACE ( )  B_SPLINE_SURFACE ( 3, 1, ( 
 ( #9461, #3119 ),
 ( #3265, #11899 ),
 ( #2835, #27432 ),
 ( #14177, #5416 ) ),
 .UNSPECIFIED., .F., .F., .F. ) 
 B_SPLINE_SURFACE_WITH_KNOTS ( ( 4, 4 ),
 ( 2, 2 ),
 ( 0.000000000000000000, 1.000000000000000000 ),
 ( 0.000000000000000000, 1.000000000000000000 ),
 .UNSPECIFIED. ) 
 GEOMETRIC_REPRESENTATION_ITEM ( )  RATIONAL_B_SPLINE_SURFACE ( (
 ( 1.000000000000000000, 1.000000000000000000),
 ( 0.9960225298536222738, 0.9999952330161893110),
 ( 0.9960225298536222738, 0.9999952330161893110),
 ( 1.000000000000000000, 1.000000000000000000) ) ) 
 REPRESENTATION_ITEM ( '' )  SURFACE ( )  );
#22898 = CARTESIAN_POINT ( 'NONE',  ( -23.79223135445719706, 7.157574570129600744, 32.40779366744824586 ) ) ;
#22899 = ORIENTED_EDGE ( 'NONE', *, *, #22744, .F. ) ;
#22900 = ORIENTED_EDGE ( 'NONE', *, *, #23257, .T. ) ;
#22901 = B_SPLINE_CURVE_WITH_KNOTS ( 'NONE', 3,
 ( #19546, #111, #26305, #11053 ),
 .UNSPECIFIED., .F., .F.,
 ( 4, 4 ),
 ( 0.000000000000000000, 0.008383560773332715543 ),
 .UNSPECIFIED. ) ;
#22902 = B_SPLINE_CURVE_WITH_KNOTS ( 'NONE', 3,
 ( #1642, #12854, #27981, #21505, #21647, #21797, #1918 ),
 .UNSPECIFIED., .F., .F.,
 ( 4, 3, 4 ),
 ( 0.000000000000000000, 0.02398743853561384476, 0.04000277880656215312 ),
 .UNSPECIFIED. ) ;
#22903 = CARTESIAN_POINT ( 'NONE',  ( 1.833485406944043827, 30.69200235379130959, -141.8265699653863976 ) ) ;
#22904 = CARTESIAN_POINT ( 'NONE',  ( 9.884929003653626367, -65.04493172071387619, -135.7578851563892215 ) ) ;
#22905 = EDGE_CURVE ( 'NONE', #21696, #14673, #26983, .T. ) ;
#22906 = CARTESIAN_POINT ( 'NONE',  ( -90.83090735639699176, 0.000000000000000000, 0.000000000000000000 ) ) ;
#22907 = EDGE_CURVE ( 'NONE', #27330, #13865, #9759, .T. ) ;
#22908 = CARTESIAN_POINT ( 'NONE',  ( 32.73300124599739291, -66.00340565729273123, -97.37344512919924000 ) ) ;
#22909 = CARTESIAN_POINT ( 'NONE',  ( 13.84597867724971287, 20.08297016719580697, -145.3211459389822835 ) ) ;
#22910 = EDGE_LOOP ( 'NONE', ( #24312, #19986, #24467, #23201 ) ) ;
#22911 = CARTESIAN_POINT ( 'NONE',  ( 2.433796855181233454, 84.34988187691088513, -118.5671979538048504 ) ) ;
#22912 = ADVANCED_FACE ( 'NONE', ( #24858 ), #25100, .F. ) ;
#22913 = CARTESIAN_POINT ( 'NONE',  ( 109.1589550718174877, 0.004900004919104999912, 0.005777059646704606720 ) ) ;
#22914 = ORIENTED_EDGE ( 'NONE', *, *, #1726, .F. ) ;
#22915 = B_SPLINE_CURVE_WITH_KNOTS ( 'NONE', 3,
 ( #15877, #24685, #2775, #26236, #15288, #2185 ),
 .UNSPECIFIED., .F., .F.,
 ( 4, 2, 4 ),
 ( 4.906538933386797396E-18, 0.0004335151646191519543, 0.0008670303292382989212 ),
 .UNSPECIFIED. ) ;
#22916 = ORIENTED_EDGE ( 'NONE', *, *, #19891, .F. ) ;
#22917 = CARTESIAN_POINT ( 'NONE',  ( -9.156249394959706578, -24.29252099376457608, 48.78605533024762764 ) ) ;
#22918 = CARTESIAN_POINT ( 'NONE',  ( -9.156249394959706578, -25.18996226954649131, -48.32878616081000445 ) ) ;
#22919 = CARTESIAN_POINT ( 'NONE',  ( 10.93730112725996229, -20.69552240458240888, -149.7554878793151545 ) ) ;
#22920 = DIRECTION ( 'NONE',  ( -1.000000000000000000, -0.000000000000000000, -0.000000000000000000 ) ) ;
#22921 = CARTESIAN_POINT ( 'NONE',  ( -4.178947244162635855, 3.367451375481794074, 48.81675275154071869 ) ) ;
#22922 = CARTESIAN_POINT ( 'NONE',  ( 1.833691583653556334, -138.1170938425794930, 44.50270951807501518 ) ) ;
#22923 = EDGE_LOOP ( 'NONE', ( #1004, #22476, #20341, #22733 ) ) ;
#22924 = CARTESIAN_POINT ( 'NONE',  ( -1.619063947482201282, 44.80407745103784123, -11.94059994246174838 ) ) ;
#22925 = CARTESIAN_POINT ( 'NONE',  ( -1.113548883309547266, -25.34012683631582519, -38.22628252420800976 ) ) ;
#22926 = B_SPLINE_CURVE_WITH_KNOTS ( 'NONE', 3,
 ( #10911, #1979, #17657, #6317, #15066, #26436 ),
 .UNSPECIFIED., .F., .F.,
 ( 4, 2, 4 ),
 ( 0.000000000000000000, 0.0006311571484586089333, 0.001262314296917217650 ),
 .UNSPECIFIED. ) ;
#22927 = B_SPLINE_CURVE_WITH_KNOTS ( 'NONE', 3,
 ( #15054, #14926, #24146, #17647, #4131, #13180, #26017, #21837 ),
 .UNSPECIFIED., .F., .F.,
 ( 4, 2, 2, 4 ),
 ( 0.000000000000000000, 0.002761524886576596435, 0.005523049773153192871, 0.01104609954630638054 ),
 .UNSPECIFIED. ) ;
#22928 = CARTESIAN_POINT ( 'NONE',  ( -1.031422197589716205, 1.530725436378091553, 45.78027046666442601 ) ) ;
#22929 = CARTESIAN_POINT ( 'NONE',  ( -4.780792508754313275, -42.16805077400938728, 25.98388465890126042 ) ) ;
#22930 = CARTESIAN_POINT ( 'NONE',  ( -1.056502255334264895, 43.72121397317241787, 13.66916755949804951 ) ) ;
#22931 = VERTEX_POINT ( 'NONE', #13749 ) ;
#22932 = CARTESIAN_POINT ( 'NONE',  ( -55.25719721206881729, 0.007063345920781645762, 0.008651607285661163521 ) ) ;
#22933 = ORIENTED_EDGE ( 'NONE', *, *, #4502, .T. ) ;
#22934 = ORIENTED_EDGE ( 'NONE', *, *, #9136, .F. ) ;
#22935 = ORIENTED_EDGE ( 'NONE', *, *, #5361, .T. ) ;
#22936 = EDGE_CURVE ( 'NONE', #309, #10869, #16219, .T. ) ;
#22937 = B_SPLINE_CURVE_WITH_KNOTS ( 'NONE', 3,
 ( #21763, #13114, #9, #21900, #10962, #17563, #26353, #6654 ),
 .UNSPECIFIED., .F., .F.,
 ( 4, 2, 2, 4 ),
 ( 0.000000000000000000, 0.002761524886576660620, 0.005523049773153321240, 0.01104609954630662513 ),
 .UNSPECIFIED. ) ;
#22938 = FACE_OUTER_BOUND ( 'NONE', #12167, .T. ) ;
#22939 = EDGE_CURVE ( 'NONE', #3393, #4316, #24196, .T. ) ;
#22940 = UNCERTAINTY_MEASURE_WITH_UNIT (LENGTH_MEASURE( 1.000000000000000082E-05 ), #12714, 'distance_accuracy_value', 'NONE');
#22941 = CARTESIAN_POINT ( 'NONE',  ( -7.733045908741338792, -21.80378472388456501, 47.75066202881817645 ) ) ;
#22942 = CARTESIAN_POINT ( 'NONE',  ( -6.588769196390763305, 26.02756986588603993, 44.25609997968876996 ) ) ;
#22943 = EDGE_CURVE ( 'NONE', #11824, #15305, #3938, .T. ) ;
#22944 = CARTESIAN_POINT ( 'NONE',  ( 32.73300124599732897, 117.3295799645430151, 8.473903470906510194 ) ) ;
#22945 = ORIENTED_EDGE ( 'NONE', *, *, #14621, .T. ) ;
#22946 = CARTESIAN_POINT ( 'NONE',  ( 8.186469829614388516, 3.468244397269210300, -149.3111477833938352 ) ) ;
#22947 = VECTOR ( 'NONE', #25243, 1000.000000000000000 ) ;
#22948 = CARTESIAN_POINT ( 'NONE',  ( 10.93730112725990367, -108.9902118373734652, -104.7670965581022671 ) ) ;
#22949 = CARTESIAN_POINT ( 'NONE',  ( 1.833485406944043827, -85.72460230293772554, 117.0814567582541201 ) ) ;
#22950 = DIRECTION ( 'NONE',  ( 0.000000000000000000, 0.000000000000000000, 1.000000000000000000 ) ) ;
#22951 = AXIS2_PLACEMENT_3D ( 'NONE', #17687, #2717, #9197 ) ;
#22952 = DIRECTION ( 'NONE',  ( 1.000000000000000000, -6.938893903907226837E-18, 1.734723475976806709E-18 ) ) ;
#22953 = B_SPLINE_CURVE_WITH_KNOTS ( 'NONE', 3,
 ( #7170, #26996, #11764, #9168 ),
 .UNSPECIFIED., .F., .F.,
 ( 4, 4 ),
 ( 3.628665131031684266E-16, 0.01077107486149801903 ),
 .UNSPECIFIED. ) ;
#22954 = CARTESIAN_POINT ( 'NONE',  ( -20.57838717382308147, -25.16001208503117326, -16.28767523336112433 ) ) ;
#22955 = DIRECTION ( 'NONE',  ( 0.5914120900931444380, -0.4101107478122166805, 0.6942916636548092102 ) ) ;
#22956 = CARTESIAN_POINT ( 'NONE',  ( -25.21435515916043357, -34.29329011225959079, -4.655591116594231416 ) ) ;
#22957 = CARTESIAN_POINT ( 'NONE',  ( 1.832998868059858122, 84.86110816369759391, -117.7096351258379485 ) ) ;
#22958 = CARTESIAN_POINT ( 'NONE',  ( 1.833206310202334377, -107.3376456496887812, 97.64934828277057477 ) ) ;
#22959 = EDGE_LOOP ( 'NONE', ( #12072, #14385, #15942, #20136 ) ) ;
#22960 = CARTESIAN_POINT ( 'NONE',  ( 109.1778270068192853, 0.008360410075186669801, 0.004106684808172150064 ) ) ;
#22961 = VERTEX_POINT ( 'NONE', #7017 ) ;
#22962 = CARTESIAN_POINT ( 'NONE',  ( 28.37603512858360233, -22.09615328858523498, 112.5845402829047970 ) ) ;
#22963 = CARTESIAN_POINT ( 'NONE',  ( 26.11404676487259024, 103.8885755249569485, 45.01677474591446781 ) ) ;
#22964 = ORIENTED_EDGE ( 'NONE', *, *, #24716, .F. ) ;
#22965 = VERTEX_POINT ( 'NONE', #2529 ) ;
#22966 = ORIENTED_EDGE ( 'NONE', *, *, #20109, .T. ) ;
#22967 = EDGE_CURVE ( 'NONE', #16711, #19505, #949, .T. ) ;
#22968 = B_SPLINE_CURVE_WITH_KNOTS ( 'NONE', 3,
 ( #19610, #22797, #7379, #18450, #18289, #27071, #9539 ),
 .UNSPECIFIED., .F., .F.,
 ( 4, 3, 4 ),
 ( 9.269414991073849107E-17, 0.009512539173626381045, 0.02506242213020854620 ),
 .UNSPECIFIED. ) ;
#22969 = EDGE_CURVE ( 'NONE', #6918, #14537, #24431, .T. ) ;
#22970 = ORIENTED_EDGE ( 'NONE', *, *, #4383, .F. ) ;
#22971 = CARTESIAN_POINT ( 'NONE',  ( -55.24340739397742084, -0.008612749836246226184, 0.005344433640972935315 ) ) ;
#22972 = ADVANCED_FACE ( 'NONE', ( #369 ), #16263, .F. ) ;
#22973 = CARTESIAN_POINT ( 'NONE',  ( -55.24390624410018802, -0.01032895241566633357, -0.001451500391952961289 ) ) ;
#22974 = B_SPLINE_CURVE_WITH_KNOTS ( 'NONE', 3,
 ( #21870, #2126, #24180, #13212, #26458, #22003, #11069, #268, #17679, #22742 ),
 .UNSPECIFIED., .F., .F.,
 ( 4, 3, 3, 4 ),
 ( 5.003707553108401214E-17, 0.0002669559177086480413, 0.0005339118354151201973, 0.001067817517169143433 ),
 .UNSPECIFIED. ) ;
#22975 = EDGE_CURVE ( 'NONE', #21026, #9703, #8391, .T. ) ;
#22976 = CARTESIAN_POINT ( 'NONE',  ( -19.53423201713129842, 3.678323623448370869E-15, -28.92774122539760384 ) ) ;
#22977 = CARTESIAN_POINT ( 'NONE',  ( 10.93730112725932635, 0.000000000000000000, 0.000000000000000000 ) ) ;
#22978 = CARTESIAN_POINT ( 'NONE',  ( -1.045287976400362417, -1.530335034934427574, -45.76855895860943235 ) ) ;
#22979 = FACE_OUTER_BOUND ( 'NONE', #14317, .T. ) ;
#22980 = CARTESIAN_POINT ( 'NONE',  ( 1.834118845439484335, 58.85894970554917194, 132.6369225636075839 ) ) ;
#22981 = FILL_AREA_STYLE ('',( #14161 ) ) ;
#22982 = VERTEX_POINT ( 'NONE', #3671 ) ;
#22983 = VERTEX_POINT ( 'NONE', #25572 ) ;
#22984 = DIRECTION ( 'NONE',  ( -0.5946245182733607137, 0.4701913299128860912, -0.6521823330502943827 ) ) ;
#22986 = CARTESIAN_POINT ( 'NONE',  ( 25.65782528836479770, 56.95887699624874756, -97.50004228081002111 ) ) ;
#22985 = CARTESIAN_POINT ( 'NONE',  ( 8.186469829614434701, 63.89871393833212920, -134.9918587494107953 ) ) ;
#22987 = CARTESIAN_POINT ( 'NONE',  ( -20.20700224038492721, -24.51628800869035274, 16.58740185276737122 ) ) ;
#22988 = CARTESIAN_POINT ( 'NONE',  ( 1.893872463202057821, 138.3372034345896679, -43.94661640105876899 ) ) ;
#22989 = ORIENTED_EDGE ( 'NONE', *, *, #4568, .T. ) ;
#22990 = ORIENTED_EDGE ( 'NONE', *, *, #19472, .T. ) ;
#22991 = CARTESIAN_POINT ( 'NONE',  ( 8.186469829614230420, -49.43817854882404106, 140.9315935955037276 ) ) ;
#22992 = CARTESIAN_POINT ( 'NONE',  ( 25.69398547355837792, -35.60637981494781457, -107.1830796521258264 ) ) ;
#22993 = CARTESIAN_POINT ( 'NONE',  ( 1.833721034905616776, -14.81406766076032078, 144.3516387774751877 ) ) ;
#22994 = ORIENTED_EDGE ( 'NONE', *, *, #6675, .T. ) ;
#22995 = CARTESIAN_POINT ( 'NONE',  ( 25.64699802086724034, -97.66487797954053462, 56.66140964017699844 ) ) ;
#22996 = EDGE_CURVE ( 'NONE', #24138, #7370, #26557, .T. ) ;
#22997 = VERTEX_POINT ( 'NONE', #21237 ) ;
#22998 = CARTESIAN_POINT ( 'NONE',  ( 10.93730112725932635, 0.000000000000000000, 0.000000000000000000 ) ) ;
#22999 = EDGE_CURVE ( 'NONE', #21238, #1868, #20396, .T. ) ;
#23000 = DIRECTION ( 'NONE',  ( 0.7563875759206388771, 0.3556158456312978888, 0.5490129373055215867 ) ) ;
#23001 = CARTESIAN_POINT ( 'NONE',  ( 26.28373643307398311, -60.14387450369918042, 112.4918671811459490 ) ) ;
#23002 = ORIENTED_EDGE ( 'NONE', *, *, #1572, .T. ) ;
#23003 = ADVANCED_FACE ( 'NONE', ( #12309 ), #10551, .F. ) ;
#23004 = APPLICATION_PROTOCOL_DEFINITION ( 'draft international standard', 'automotive_design', 1998, #27763 ) ;
#23005 = B_SPLINE_CURVE_WITH_KNOTS ( 'NONE', 3,
 ( #26309, #6886, #10788, #116 ),
 .UNSPECIFIED., .F., .F.,
 ( 4, 4 ),
 ( 2.416688344895611942E-16, 0.008383748772659726026 ),
 .UNSPECIFIED. ) ;
#23006 = CARTESIAN_POINT ( 'NONE',  ( 26.11404676487257603, 110.9778746459749641, -22.43340081644658213 ) ) ;
#23007 = CARTESIAN_POINT ( 'NONE',  ( 2.433796855181219243, 132.3327394885239698, -60.50726454507772445 ) ) ;
#23008 = CARTESIAN_POINT ( 'NONE',  ( -20.20700224038492721, 29.58392382092673500, 0.9908225410479544193 ) ) ;
#23009 = ORIENTED_EDGE ( 'NONE', *, *, #21295, .F. ) ;
#23010 = DIRECTION ( 'NONE',  ( 1.000000000000000000, -6.938893903907226837E-18, 1.734723475976806709E-18 ) ) ;
#23012 = CARTESIAN_POINT ( 'NONE',  ( -1.049817751779881680, 43.71287583013727129, -13.66628317065001674 ) ) ;
#23011 = DIRECTION ( 'NONE',  ( 0.000000000000000000, 5.223019709708233256E-21, -1.000000000000000000 ) ) ;
#23013 = CARTESIAN_POINT ( 'NONE',  ( -25.21435515916043713, -23.92354251275954979, -25.00736669481013053 ) ) ;
#23014 = ORIENTED_EDGE ( 'NONE', *, *, #23450, .F. ) ;
#23015 = VERTEX_POINT ( 'NONE', #5850 ) ;
#23016 = VERTEX_POINT ( 'NONE', #1518 ) ;
#23017 = CARTESIAN_POINT ( 'NONE',  ( -8.786685647604890903, -23.24040270374424466, -48.22796981442760256 ) ) ;
#23018 = CARTESIAN_POINT ( 'NONE',  ( 55.79472521941426777, -72.42790650415579989, 6.880567342319468871 ) ) ;
#23020 = CARTESIAN_POINT ( 'NONE',  ( 25.64700659047692355, 12.02873506870318998, -112.2686754657454316 ) ) ;
#23019 = CARTESIAN_POINT ( 'NONE',  ( 24.01988960052050359, 103.4492499592085437, 80.44223964539884264 ) ) ;
#23021 = CARTESIAN_POINT ( 'NONE',  ( -20.24419206586952313, -7.929973069813210707, 28.55732805495823712 ) ) ;
#23022 = CARTESIAN_POINT ( 'NONE',  ( 1.833838850855499913, -132.5281727421681524, -59.10274688031982748 ) ) ;
#23023 = CARTESIAN_POINT ( 'NONE',  ( 25.64681081121879203, -83.63051021305953725, 75.86069728268962820 ) ) ;
#23024 = CARTESIAN_POINT ( 'NONE',  ( 32.73300124599737160, -117.5726003567929610, 3.836798148478423265 ) ) ;
#23025 = ORIENTED_EDGE ( 'NONE', *, *, #5353, .T. ) ;
#23026 = CARTESIAN_POINT ( 'NONE',  ( 28.37644542392846247, -116.9383271603242491, -42.25924161794007006 ) ) ;
#23027 = CARTESIAN_POINT ( 'NONE',  ( -8.786685647604890903, -37.00619870957961410, -38.68584556812286479 ) ) ;
#23028 = CARTESIAN_POINT ( 'NONE',  ( 25.64681081121879203, -66.70335573067929147, 91.10197563707923507 ) ) ;
#23029 = DIRECTION ( 'NONE',  ( 0.000000000000000000, 0.000000000000000000, 1.000000000000000000 ) ) ;
#23030 = AXIS2_PLACEMENT_3D ( 'NONE', #4528, #26545, #21817 ) ;
#23031 = CARTESIAN_POINT ( 'NONE',  ( -55.24390624410018802, 0.004572280736703349113, -0.009374879212967143077 ) ) ;
#23032 = CARTESIAN_POINT ( 'NONE',  ( -16.86833981943424021, -39.83928801320577406, 19.19877306373892978 ) ) ;
#23033 = CARTESIAN_POINT ( 'NONE',  ( 26.11404676487257603, -102.9690087468798509, -47.08215554553621729 ) ) ;
#23034 = AXIS2_PLACEMENT_3D ( 'NONE', #22541, #26689, #13593 ) ;
#23035 = ORIENTED_EDGE ( 'NONE', *, *, #14098, .F. ) ;
#23037 = CARTESIAN_POINT ( 'NONE',  ( 26.04756280548353686, -12.93458011762399984, -112.4366864265128783 ) ) ;
#23036 = B_SPLINE_CURVE_WITH_KNOTS ( 'NONE', 3,
 ( #24176, #11064, #22294, #123, #21999, #13346, #4433, #11205, #19979, #15501, #264, #17806, #2554 ),
 .UNSPECIFIED., .F., .F.,
 ( 4, 3, 3, 3, 4 ),
 ( 9.813077866773594792E-18, 0.0007657099931970512375, 0.001531419946797918071, 0.002296279302920157302, 0.003061450627205767206 ),
 .UNSPECIFIED. ) ;
#23038 = CONICAL_SURFACE ( 'NONE', #20705, 34.60786435723138510, 0.8559913436420825139 ) ;
#23039 = DIRECTION ( 'NONE',  ( 0.000000000000000000, 5.223019709708233256E-21, -1.000000000000000000 ) ) ;
#23040 = CARTESIAN_POINT ( 'NONE',  ( -20.57838717382308147, -18.89542499756516847, -23.26537097894098594 ) ) ;
#23041 = EDGE_CURVE ( 'NONE', #26014, #27008, #20758, .T. ) ;
#23042 = ORIENTED_EDGE ( 'NONE', *, *, #12184, .F. ) ;
#23043 = EDGE_LOOP ( 'NONE', ( #17460, #6347, #23638, #9420 ) ) ;
#23044 = EDGE_CURVE ( 'NONE', #24848, #16392, #17993, .T. ) ;
#23045 = ADVANCED_FACE ( 'NONE', ( #10175 ), #19362, .F. ) ;
#23046 = CARTESIAN_POINT ( 'NONE',  ( -1.049817751779892117, -45.79652915392414769, -0.5106138415325238711 ) ) ;
#23047 = CARTESIAN_POINT ( 'NONE',  ( 2.108393763691205347, 73.75286979200633652, -125.1820217068188015 ) ) ;
#23048 = CIRCLE ( 'NONE', #10617, 117.6351876552689504 ) ;
#23049 = CARTESIAN_POINT ( 'NONE',  ( 32.73300124599735739, -51.32617430724984331, 105.8473486001049224 ) ) ;
#23050 = CARTESIAN_POINT ( 'NONE',  ( 25.64660436782553177, 97.49251393956843970, -56.95711784271874478 ) ) ;
#23051 = CARTESIAN_POINT ( 'NONE',  ( 1.833206308920056538, -144.3905119031281004, 14.42724735286800986 ) ) ;
#23052 = VECTOR ( 'NONE', #3129, 1000.000000000000114 ) ;
#23053 = CARTESIAN_POINT ( 'NONE',  ( -1.031422197589711764, 43.06660437151329290, 15.60268798220593034 ) ) ;
#23054 = CARTESIAN_POINT ( 'NONE',  ( -20.20700224038492721, 18.19058640100257662, 23.35150625415638714 ) ) ;
#23055 = ORIENTED_EDGE ( 'NONE', *, *, #16857, .T. ) ;
#23056 = VECTOR ( 'NONE', #2665, 1000.000000000000000 ) ;
#23057 = ORIENTED_EDGE ( 'NONE', *, *, #28105, .T. ) ;
#23058 = CARTESIAN_POINT ( 'NONE',  ( -55.24390624410018802, -0.004896917417127438256, -0.009209468562451287102 ) ) ;
#23059 = CARTESIAN_POINT ( 'NONE',  ( 109.1721716018069657, -0.01281875973824533367, -0.01127028715940098409 ) ) ;
#23060 = CARTESIAN_POINT ( 'NONE',  ( -25.21435515916043357, 31.17620025257608418, 15.02493970636113474 ) ) ;
#23061 = CARTESIAN_POINT ( 'NONE',  ( -20.57838717382308147, -28.96176188950224528, -7.715628353033566533 ) ) ;
#23062 = CARTESIAN_POINT ( 'NONE',  ( 1.831572820252008738, -107.1759352627499595, -97.82994539998490779 ) ) ;
#23063 =( BOUNDED_SURFACE ( )  B_SPLINE_SURFACE ( 3, 1, ( 
 ( #6561, #21815 ),
 ( #1940, #8440 ),
 ( #15456, #10746 ),
 ( #24265, #21666 ) ),
 .UNSPECIFIED., .F., .F., .F. ) 
 B_SPLINE_SURFACE_WITH_KNOTS ( ( 4, 4 ),
 ( 2, 2 ),
 ( 0.000000000000000000, 1.000000000000000000 ),
 ( 0.000000000000000000, 1.000000000000000000 ),
 .UNSPECIFIED. ) 
 GEOMETRIC_REPRESENTATION_ITEM ( )  RATIONAL_B_SPLINE_SURFACE ( (
 ( 1.000000000000000000, 1.000000000000000000),
 ( 0.9934239774497837239, 0.8357310067453919133),
 ( 0.9934239774497837239, 0.8357310067453919133),
 ( 1.000000000000000000, 1.000000000000000000) ) ) 
 REPRESENTATION_ITEM ( '' )  SURFACE ( )  );
#23064 = CARTESIAN_POINT ( 'NONE',  ( 1.833721034905618774, -137.8972080590635017, 45.17977675814267968 ) ) ;
#23065 = DIRECTION ( 'NONE',  ( -1.000000000000000000, -0.000000000000000000, -0.000000000000000000 ) ) ;
#23066 = ORIENTED_EDGE ( 'NONE', *, *, #21518, .F. ) ;
#23067 = CARTESIAN_POINT ( 'NONE',  ( 25.98107933586728535, 84.80123094405293216, -74.88680433646143797 ) ) ;
#23068 = CARTESIAN_POINT ( 'NONE',  ( 1.833485406944043827, 15.69895494453577101, -144.2578170162061326 ) ) ;
#23069 = DIRECTION ( 'NONE',  ( -1.000000000000000000, -0.000000000000000000, -0.000000000000000000 ) ) ;
#23070 = CARTESIAN_POINT ( 'NONE',  ( 109.1586900883932856, 0.004113747440992326053, -0.005833932871491330496 ) ) ;
#23071 = EDGE_CURVE ( 'NONE', #17905, #8156, #12156, .T. ) ;
#23072 = ORIENTED_EDGE ( 'NONE', *, *, #1076, .F. ) ;
#23073 = ORIENTED_EDGE ( 'NONE', *, *, #24837, .F. ) ;
#23074 = CARTESIAN_POINT ( 'NONE',  ( 25.70243777736192214, 22.76560620137062330, 110.6300896395617741 ) ) ;
#23075 = AXIS2_PLACEMENT_3D ( 'NONE', #27662, #27514, #8239 ) ;
#23076 = CARTESIAN_POINT ( 'NONE',  ( -20.57838717382308147, 18.89542499756533545, 23.26537097894084383 ) ) ;
#23077 = ORIENTED_EDGE ( 'NONE', *, *, #24199, .F. ) ;
#23078 = VECTOR ( 'NONE', #27267, 1000.000000000000000 ) ;
#23079 = EDGE_CURVE ( 'NONE', #26786, #4240, #27425, .T. ) ;
#23080 = EDGE_CURVE ( 'NONE', #10456, #22401, #21786, .T. ) ;
#23081 = ORIENTED_EDGE ( 'NONE', *, *, #12959, .F. ) ;
#23082 = ORIENTED_EDGE ( 'NONE', *, *, #8339, .F. ) ;
#23083 = CONICAL_SURFACE ( 'NONE', #25827, 117.6351876552689504, 0.9945805576725580410 ) ;
#23084 = CARTESIAN_POINT ( 'NONE',  ( 25.64700659047696263, -110.3963107228934746, -23.69811251893846560 ) ) ;
#23085 = CARTESIAN_POINT ( 'NONE',  ( 28.37644542392840563, -119.4444529625692724, 34.54617949428059376 ) ) ;
#23086 = CARTESIAN_POINT ( 'NONE',  ( -1.031422197589711987, 45.78027046666443312, -1.530725436377622151 ) ) ;
#23087 = CARTESIAN_POINT ( 'NONE',  ( 2.108985857320863744, -13.91228467251917067, 144.6256801373126564 ) ) ;
#23088 = CARTESIAN_POINT ( 'NONE',  ( -8.786685647604720373, -47.14957014837338534, -25.35688121747513435 ) ) ;
#23089 = CARTESIAN_POINT ( 'NONE',  ( -7.711401346138401891, 6.030154970217631138, 52.11446537925907307 ) ) ;
#23090 = CARTESIAN_POINT ( 'NONE',  ( -25.21435515916043713, 25.00736669481056751, 23.92354251275909505 ) ) ;
#23091 = CARTESIAN_POINT ( 'NONE',  ( -21.41427618760457463, 16.60878262545457318, 25.94789270595488517 ) ) ;
#23092 = CARTESIAN_POINT ( 'NONE',  ( 25.69398547355839213, -110.3177996916215733, 24.20764173643367556 ) ) ;
#23093 = CARTESIAN_POINT ( 'NONE',  ( 21.16825799904904315, -119.4343305756974587, -63.85626241912861900 ) ) ;
#23095 = VECTOR ( 'NONE', #19003, 1000.000000000000227 ) ;
#23094 =( BOUNDED_SURFACE ( )  B_SPLINE_SURFACE ( 3, 1, ( 
 ( #22262, #2523 ),
 ( #9307, #4971 ),
 ( #16051, #20082 ),
 ( #2971, #11746 ) ),
 .UNSPECIFIED., .F., .F., .F. ) 
 B_SPLINE_SURFACE_WITH_KNOTS ( ( 4, 4 ),
 ( 2, 2 ),
 ( 0.000000000000000000, 1.000000000000000000 ),
 ( 0.000000000000000000, 1.000000000000000000 ),
 .UNSPECIFIED. ) 
 GEOMETRIC_REPRESENTATION_ITEM ( )  RATIONAL_B_SPLINE_SURFACE ( (
 ( 1.000000000000000000, 1.000000000000000000),
 ( 0.9960225298536222738, 0.9999952330161893110),
 ( 0.9960225298536222738, 0.9999952330161893110),
 ( 1.000000000000000000, 1.000000000000000000) ) ) 
 REPRESENTATION_ITEM ( '' )  SURFACE ( )  );
#23096 = EDGE_CURVE ( 'NONE', #9151, #22124, #10868, .T. ) ;
#23097 = CARTESIAN_POINT ( 'NONE',  ( 6.224689322667630975, 145.3353551538644979, -28.26953958630477004 ) ) ;
#23098 = CARTESIAN_POINT ( 'NONE',  ( 8.186469829614354765, -148.1306754360700211, -19.05650981809974098 ) ) ;
#23099 = CARTESIAN_POINT ( 'NONE',  ( 13.84597867724974307, 35.16314962060035754, -142.4258194868989449 ) ) ;
#23100 = CARTESIAN_POINT ( 'NONE',  ( -55.24198130335446422, 0.009170435128245573234, 0.001516807524708093389 ) ) ;
#23101 = DIRECTION ( 'NONE',  ( -1.000000000000000000, -0.000000000000000000, -0.000000000000000000 ) ) ;
#23102 = EDGE_CURVE ( 'NONE', #17407, #22931, #25213, .T. ) ;
#23103 = VERTEX_POINT ( 'NONE', #6698 ) ;
#23104 = CARTESIAN_POINT ( 'NONE',  ( -1.259972190295308936, 25.19627397134298263, -38.49631882650656678 ) ) ;
#23105 = EDGE_CURVE ( 'NONE', #23707, #6993, #3819, .T. ) ;
#23106 = EDGE_LOOP ( 'NONE', ( #25716, #5055, #12034, #4988 ) ) ;
#23107 = CARTESIAN_POINT ( 'NONE',  ( 2.430230287190589422, 142.0258656395025980, -31.67257033707363689 ) ) ;
#23108 = CARTESIAN_POINT ( 'NONE',  ( -1.050231094221210748, 27.12595454131558981, 36.90262059116437854 ) ) ;
#23109 = VERTEX_POINT ( 'NONE', #21804 ) ;
#23110 = ORIENTED_EDGE ( 'NONE', *, *, #10305, .T. ) ;
#23111 = ORIENTED_EDGE ( 'NONE', *, *, #7450, .T. ) ;
#23112 = VECTOR ( 'NONE', #19104, 999.9999999999998863 ) ;
#23113 = CARTESIAN_POINT ( 'NONE',  ( 1.832998868059890096, -125.9352106559988869, 72.09222286251041112 ) ) ;
#23114 = AXIS2_PLACEMENT_3D ( 'NONE', #1669, #6292, #28007 ) ;
#23115 = CARTESIAN_POINT ( 'NONE',  ( 109.1589550718175161, 0.006669585340474266412, 0.003591809816099548244 ) ) ;
#23116 = CARTESIAN_POINT ( 'NONE',  ( 25.87036335909426299, 107.8283083010004617, 33.99475147239049022 ) ) ;
#23117 = DIRECTION ( 'NONE',  ( 0.000000000000000000, 5.223019709707975211E-21, -1.000000000000000000 ) ) ;
#23118 = CARTESIAN_POINT ( 'NONE',  ( -1.539763995773680838, 29.16712963492463473, -35.94321074656906490 ) ) ;
#23119 = CARTESIAN_POINT ( 'NONE',  ( 1.833750490713698111, -58.77746103890191165, -132.6726660571949594 ) ) ;
#23120 = CARTESIAN_POINT ( 'NONE',  ( 8.186469829614223315, 27.65107825763956839, 146.7694295239425060 ) ) ;
#23122 = CARTESIAN_POINT ( 'NONE',  ( 2.433796855181205476, 57.85512797797890272, 133.5135467655520074 ) ) ;
#23121 = CARTESIAN_POINT ( 'NONE',  ( 1.833485406944043827, 59.50871042846404180, -132.3460930279885019 ) ) ;
#23123 = CARTESIAN_POINT ( 'NONE',  ( -20.20700224038492721, -16.58740185276692358, 24.51628800869065827 ) ) ;
#23124 = EDGE_CURVE ( 'NONE', #27239, #27540, #19351, .T. ) ;
#23125 = ORIENTED_EDGE ( 'NONE', *, *, #27365, .F. ) ;
#23126 = ORIENTED_EDGE ( 'NONE', *, *, #26808, .F. ) ;
#23127 = AXIS2_PLACEMENT_3D ( 'NONE', #14690, #21458, #15100 ) ;
#23128 = CARTESIAN_POINT ( 'NONE',  ( -1.050231094221210526, -26.71409683968590798, 37.20185272688488709 ) ) ;
#23129 = EDGE_CURVE ( 'NONE', #22983, #607, #26919, .T. ) ;
#23131 = CARTESIAN_POINT ( 'NONE',  ( -1.058197053496154671, 25.48582931365525184, 38.06270006878825995 ) ) ;
#23130 = CARTESIAN_POINT ( 'NONE',  ( 1.833721034905659630, 85.58110185770094347, 117.1867194831481669 ) ) ;
#23132 = CARTESIAN_POINT ( 'NONE',  ( -8.259864102781671491, -22.52209142944967368, -47.98931516265586339 ) ) ;
#23133 = CARTESIAN_POINT ( 'NONE',  ( 26.11404676487256893, -92.25884714080449100, 65.63269960453210672 ) ) ;
#23134 = ORIENTED_EDGE ( 'NONE', *, *, #27698, .F. ) ;
#23135 = VECTOR ( 'NONE', #19240, 1000.000000000000000 ) ;
#23136 = VERTEX_POINT ( 'NONE', #26115 ) ;
#23137 = CARTESIAN_POINT ( 'NONE',  ( -4.162674018437135359, -25.90909455705140729, -41.48630000627045433 ) ) ;
#23138 = AXIS2_PLACEMENT_3D ( 'NONE', #19801, #9023, #22117 ) ;
#23139 = EDGE_CURVE ( 'NONE', #24558, #15270, #8729, .T. ) ;
#23140 = CARTESIAN_POINT ( 'NONE',  ( -1.155001620486273861, 35.88346938217592452, 28.62773628245626867 ) ) ;
#23141 = CARTESIAN_POINT ( 'NONE',  ( -1.056502255334264895, 27.33667001641221717, 36.75727364034702305 ) ) ;
#23142 = EDGE_LOOP ( 'NONE', ( #5172, #21913, #25920, #14893 ) ) ;
#23143 = CARTESIAN_POINT ( 'NONE',  ( 6.224689322667630975, -145.3353551538643273, 28.26953958630572217 ) ) ;
#23144 = CARTESIAN_POINT ( 'NONE',  ( -28.41354790283022069, -21.64275480268742058, 8.345538364877306492 ) ) ;
#23145 = ADVANCED_FACE ( 'NONE', ( #61 ), #14415, .F. ) ;
#23146 = VERTEX_POINT ( 'NONE', #4190 ) ;
#23147 = CIRCLE ( 'NONE', #19443, 53.53553390275978785 ) ;
#23148 = CARTESIAN_POINT ( 'NONE',  ( -4.473127245936431073, -31.51789735524165081, 37.94261489385753094 ) ) ;
#23149 = ORIENTED_EDGE ( 'NONE', *, *, #25101, .T. ) ;
#23150 = CARTESIAN_POINT ( 'NONE',  ( -20.38016308990357928, 7.753479680700950283, -28.74660391518346714 ) ) ;
#23151 = CARTESIAN_POINT ( 'NONE',  ( 55.49584447822657296, 71.02133150427273733, -14.82242356767866021 ) ) ;
#23152 = DIRECTION ( 'NONE',  ( 1.000000000000000000, 2.681782354340591992E-16, -3.486856684240843286E-17 ) ) ;
#23153 = AXIS2_PLACEMENT_3D ( 'NONE', #2662, #19943, #22101 ) ;
#23154 = CARTESIAN_POINT ( 'NONE',  ( 2.430230287190589422, 57.85706160874325832, -133.5180086894985436 ) ) ;
#23155 = CONICAL_SURFACE ( 'NONE', #26794, 34.60786435723138510, 0.8559913436420825139 ) ;
#23156 = LINE ( 'NONE', #16807, #10260 ) ;
#23157 = LINE ( 'NONE', #25726, #6955 ) ;
#23158 = CARTESIAN_POINT ( 'NONE',  ( -20.20612091757419648, 29.57813639663782013, 1.137293889216468790 ) ) ;
#23159 = B_SPLINE_CURVE_WITH_KNOTS ( 'NONE', 3,
 ( #15510, #2715, #11488, #272, #26742, #9193 ),
 .UNSPECIFIED., .F., .F.,
 ( 4, 2, 4 ),
 ( 7.372574772901430151E-18, 0.0006311636237756744656, 0.001262327247551341559 ),
 .UNSPECIFIED. ) ;
#23160 = ORIENTED_EDGE ( 'NONE', *, *, #7829, .T. ) ;
#23161 = CARTESIAN_POINT ( 'NONE',  ( -55.25297051322618813, 0.006313402748432478395, 0.01354497706059498707 ) ) ;
#23163 = CARTESIAN_POINT ( 'NONE',  ( 109.1624594426973118, 0.01476644236456989799, 0.006066618937910955682 ) ) ;
#23162 = CARTESIAN_POINT ( 'NONE',  ( 26.28373643307437391, 97.52903534490830850, 82.21796085350655403 ) ) ;
#23164 = CARTESIAN_POINT ( 'NONE',  ( 25.64681081121879203, 97.99105938547923245, 56.09509703373377931 ) ) ;
#23165 = VERTEX_POINT ( 'NONE', #8800 ) ;
#23166 = B_SPLINE_CURVE_WITH_KNOTS ( 'NONE', 3,
 ( #20889, #9969, #7812, #16570, #25365, #5639 ),
 .UNSPECIFIED., .F., .F.,
 ( 4, 2, 4 ),
 ( 0.000000000000000000, 0.0004335151646191525506, 0.0008670303292383051011 ),
 .UNSPECIFIED. ) ;
#23167 = ORIENTED_EDGE ( 'NONE', *, *, #23720, .F. ) ;
#23168 = ORIENTED_EDGE ( 'NONE', *, *, #27400, .T. ) ;
#23169 = LINE ( 'NONE', #19238, #10185 ) ;
#23170 = CARTESIAN_POINT ( 'NONE',  ( -25.21435515916043713, -31.17620025257576799, 15.02493970636179377 ) ) ;
#23171 = EDGE_CURVE ( 'NONE', #19971, #7054, #14895, .T. ) ;
#23173 = CARTESIAN_POINT ( 'NONE',  ( 5.340103579038339099, 139.5040934216406754, -47.74933483136739198 ) ) ;
#23172 = CARTESIAN_POINT ( 'NONE',  ( -1.619063947482197729, -38.92136151114888776, 25.20140673341416360 ) ) ;
#23174 = CARTESIAN_POINT ( 'NONE',  ( -23.79223135445719350, 30.42557260166829636, 13.25822371132262845 ) ) ;
#23175 = CARTESIAN_POINT ( 'NONE',  ( 2.430230287190589422, -126.7388733285340123, -71.49654683843642999 ) ) ;
#23176 = ORIENTED_EDGE ( 'NONE', *, *, #22844, .T. ) ;
#23177 = CARTESIAN_POINT ( 'NONE',  ( -55.24271866751342941, 0.008488649505343330570, 0.004256484107795472684 ) ) ;
#23178 = CARTESIAN_POINT ( 'NONE',  ( 16.05277956358202474, -143.2298391883442719, 4.672229451527324606 ) ) ;
#23179 = ORIENTED_EDGE ( 'NONE', *, *, #10235, .T. ) ;
#23180 = CARTESIAN_POINT ( 'NONE',  ( 32.73300124599740002, -110.6325518752271080, -39.98094346392423404 ) ) ;
#23181 = CARTESIAN_POINT ( 'NONE',  ( 32.73300124599739291, -20.69176323058542621, -115.8010721414085538 ) ) ;
#23182 = CARTESIAN_POINT ( 'NONE',  ( 109.1592201516379674, -0.007620268632968129653, -0.001934867487012907703 ) ) ;
#23183 = EDGE_CURVE ( 'NONE', #26534, #8900, #15744, .T. ) ;
#23184 = CARTESIAN_POINT ( 'NONE',  ( 10.93730112725977932, -108.9902118373748863, 104.7670965581006755 ) ) ;
#23185 = CARTESIAN_POINT ( 'NONE',  ( 2.433796855181205476, -118.5671979538062146, 84.34988187690890982 ) ) ;
#23186 = VERTEX_POINT ( 'NONE', #10827 ) ;
#23187 = CARTESIAN_POINT ( 'NONE',  ( -4.473127245936434626, -49.22197550883367256, 3.196405119334318812 ) ) ;
#23188 = CARTESIAN_POINT ( 'NONE',  ( 13.84597867724976439, -112.1633818588832554, 94.55652763153787532 ) ) ;
#23189 = CARTESIAN_POINT ( 'NONE',  ( 9.884929003653626367, -57.36421526887254885, 139.1775604444702026 ) ) ;
#23190 = ORIENTED_EDGE ( 'NONE', *, *, #18564, .T. ) ;
#23191 = CARTESIAN_POINT ( 'NONE',  ( -55.24198130335446422, -0.001391250620101175178, -0.009190321388310287998 ) ) ;
#23192 = ORIENTED_EDGE ( 'NONE', *, *, #2468, .T. ) ;
#23193 = CARTESIAN_POINT ( 'NONE',  ( 109.1721716018069657, -0.006757465437538680460, 0.01567407524362086566 ) ) ;
#23194 = CARTESIAN_POINT ( 'NONE',  ( 25.69398547355838502, -102.8740393624597402, 46.61500694509608422 ) ) ;
#23195 = CARTESIAN_POINT ( 'NONE',  ( -1.045287976400362417, -12.68782741917263657, 44.00138577190661948 ) ) ;
#23196 = CARTESIAN_POINT ( 'NONE',  ( 1.833750490713699666, 138.0897889879345257, -44.58740205676186008 ) ) ;
#23197 = ORIENTED_EDGE ( 'NONE', *, *, #24763, .F. ) ;
#23198 = CARTESIAN_POINT ( 'NONE',  ( 1.833721034905634317, 142.0123736691687384, 29.82176961966964512 ) ) ;
#23199 = CARTESIAN_POINT ( 'NONE',  ( -6.574463467970653952, 38.37705091668375701, -34.08059230520056104 ) ) ;
#23200 = CARTESIAN_POINT ( 'NONE',  ( 25.64681081121880624, -45.54494737132293380, 103.3177883989777825 ) ) ;
#23201 = ORIENTED_EDGE ( 'NONE', *, *, #23852, .T. ) ;
#23202 = ORIENTED_EDGE ( 'NONE', *, *, #21088, .T. ) ;
#23203 = CARTESIAN_POINT ( 'NONE',  ( 1.833485406944043827, -30.69200235379031838, 141.8265699653866250 ) ) ;
#23204 = CARTESIAN_POINT ( 'NONE',  ( -55.24390624410018802, 0.01032895241566708991, 0.001451500391952845713 ) ) ;
#23205 = ADVANCED_FACE ( 'NONE', ( #19724 ), #17334, .F. ) ;
#23206 = CARTESIAN_POINT ( 'NONE',  ( 30.58324630866347604, -74.24222250960175984, -95.47492154584236346 ) ) ;
#23207 = CARTESIAN_POINT ( 'NONE',  ( 2.433796855181233454, 1.451562450949631211, 145.5024947199069913 ) ) ;
#23208 = CARTESIAN_POINT ( 'NONE',  ( 109.1592201516379674, 0.007748443302134881173, 0.001331853079201419324 ) ) ;
#23209 = CARTESIAN_POINT ( 'NONE',  ( -1.539763995773683503, 2.469814354917492238, -46.22267697748602444 ) ) ;
#23210 = LINE ( 'NONE', #7957, #27653 ) ;
#23211 = ORIENTED_EDGE ( 'NONE', *, *, #15957, .F. ) ;
#23212 = CARTESIAN_POINT ( 'NONE',  ( 24.01988960052069189, 100.1926921796494412, -84.46375358746813333 ) ) ;
#23213 = CARTESIAN_POINT ( 'NONE',  ( -20.57838717382308147, 27.96569011373101077, 10.78122205916971055 ) ) ;
#23214 = CARTESIAN_POINT ( 'NONE',  ( -1.045287976400379737, -25.66401692420040703, -37.92705037016734337 ) ) ;
#23215 = EDGE_CURVE ( 'NONE', #9129, #3533, #6791, .T. ) ;
#23216 = EDGE_CURVE ( 'NONE', #12888, #19804, #5995, .T. ) ;
#23217 = CARTESIAN_POINT ( 'NONE',  ( 55.79472521941426777, 21.78881894124704388, 69.41463258328519714 ) ) ;
#23218 = CARTESIAN_POINT ( 'NONE',  ( 32.73300124599736449, -115.8010721414085253, 20.69176323058589162 ) ) ;
#23219 = VERTEX_POINT ( 'NONE', #7084 ) ;
#23220 = CARTESIAN_POINT ( 'NONE',  ( -4.473127245936434626, -12.17046501147483895, 47.80062405537812964 ) ) ;
#23221 = CARTESIAN_POINT ( 'NONE',  ( -8.786685647604896232, -7.199674155858612146, 53.04920435127190359 ) ) ;
#23222 = VERTEX_POINT ( 'NONE', #27046 ) ;
#23223 = ORIENTED_EDGE ( 'NONE', *, *, #4093, .F. ) ;
#23224 = ORIENTED_EDGE ( 'NONE', *, *, #19743, .T. ) ;
#23225 = CARTESIAN_POINT ( 'NONE',  ( -8.786685647604890903, 7.199674155858966529, -53.04920435127184675 ) ) ;
#23226 = EDGE_CURVE ( 'NONE', #10266, #9920, #27581, .T. ) ;
#23227 = CARTESIAN_POINT ( 'NONE',  ( 55.79472521941426777, 72.75035398477136539, 0.7279028900796241652 ) ) ;
#23228 = CARTESIAN_POINT ( 'NONE',  ( 109.1586900883932856, 0.004113747441000917271, 0.005833932871487527982 ) ) ;
#23229 = DIRECTION ( 'NONE',  ( -0.7637818620346801257, 0.6068965246771014233, -0.2198041754873946707 ) ) ;
#23230 =( BOUNDED_SURFACE ( )  B_SPLINE_SURFACE ( 3, 1, ( 
 ( #9463, #7307 ),
 ( #963, #20097 ),
 ( #26861, #383 ),
 ( #816, #15784 ) ),
 .UNSPECIFIED., .F., .F., .F. ) 
 B_SPLINE_SURFACE_WITH_KNOTS ( ( 4, 4 ),
 ( 2, 2 ),
 ( 0.000000000000000000, 1.000000000000000000 ),
 ( 0.000000000000000000, 1.000000000000000000 ),
 .UNSPECIFIED. ) 
 GEOMETRIC_REPRESENTATION_ITEM ( )  RATIONAL_B_SPLINE_SURFACE ( (
 ( 1.000000000000000000, 1.000000000000000000),
 ( 0.9934239774497838349, 0.8357310067453913582),
 ( 0.9934239774497838349, 0.8357310067453913582),
 ( 1.000000000000000000, 1.000000000000000000) ) ) 
 REPRESENTATION_ITEM ( '' )  SURFACE ( )  );
#23231 = EDGE_CURVE ( 'NONE', #6108, #27587, #5638, .T. ) ;
#23232 = CARTESIAN_POINT ( 'NONE',  ( -16.86833981943421890, -43.51541671545732015, -7.884812276281936150 ) ) ;
#23233 = ORIENTED_EDGE ( 'NONE', *, *, #17573, .F. ) ;
#23234 = CARTESIAN_POINT ( 'NONE',  ( 1.833838850093465700, 132.5643663243757260, 59.02145475724694279 ) ) ;
#23235 = CARTESIAN_POINT ( 'NONE',  ( 2.430230287190572103, -107.1617224697457402, -98.44218333480880290 ) ) ;
#23236 = EDGE_CURVE ( 'NONE', #976, #7229, #22824, .T. ) ;
#23237 = CARTESIAN_POINT ( 'NONE',  ( 8.186469829614361871, -140.9315935955035854, -49.43817854882455975 ) ) ;
#23238 = CARTESIAN_POINT ( 'NONE',  ( 55.79472521941428198, 66.75682020267529992, 28.92526238350497536 ) ) ;
#23239 = CARTESIAN_POINT ( 'NONE',  ( 2.433796855181219243, 142.0211193075555798, 31.67151202413018396 ) ) ;
#23240 = CARTESIAN_POINT ( 'NONE',  ( -4.473127245936431073, 47.80062405537802306, -12.17046501147532567 ) ) ;
#23241 = CARTESIAN_POINT ( 'NONE',  ( -1.323830074806760848, -2.318057800980394045, 46.01435746200695576 ) ) ;
#23242 = DIRECTION ( 'NONE',  ( 0.000000000000000000, 5.223019709707975211E-21, -1.000000000000000000 ) ) ;
#23243 = B_SPLINE_CURVE_WITH_KNOTS ( 'NONE', 3,
 ( #27154, #11200, #25595, #5287, #5874, #14492, #5578, #8047, #23012, #7615, #12200, #16939, #10344 ),
 .UNSPECIFIED., .F., .F.,
 ( 4, 3, 3, 3, 4 ),
 ( 8.673617379884035472E-18, 0.0007657099931970570922, 0.001531419946797920890, 0.002296279302920155134, 0.003061450627205761568 ),
 .UNSPECIFIED. ) ;
#23244 = CARTESIAN_POINT ( 'NONE',  ( -1.619063947482197729, -25.20140673341345305, 38.92136151114934961 ) ) ;
#23245 = VECTOR ( 'NONE', #6745, 1000.000000000000227 ) ;
#23246 = ORIENTED_EDGE ( 'NONE', *, *, #6203, .F. ) ;
#23247 = CARTESIAN_POINT ( 'NONE',  ( 94.22246935314088034, 90.00000000000005684, -6.938893903907228378E-15 ) ) ;
#23248 = ORIENTED_EDGE ( 'NONE', *, *, #10105, .T. ) ;
#23249 = CARTESIAN_POINT ( 'NONE',  ( 1.833206310202322387, -15.90849712171641883, -144.2348262833783394 ) ) ;
#23250 = CARTESIAN_POINT ( 'NONE',  ( 30.59138290137870797, 107.2355347544032469, 44.78723476287341043 ) ) ;
#23251 = ORIENTED_EDGE ( 'NONE', *, *, #12265, .T. ) ;
#23252 = VERTEX_POINT ( 'NONE', #16123 ) ;
#23253 = ORIENTED_EDGE ( 'NONE', *, *, #12197, .T. ) ;
#23254 = B_SPLINE_CURVE_WITH_KNOTS ( 'NONE', 3,
 ( #7417, #22390, #2955, #14018, #926, #2656, #22829, #18191, #18487, #11299 ),
 .UNSPECIFIED., .F., .F.,
 ( 4, 3, 3, 4 ),
 ( 3.816391647148975608E-17, 0.0002669559177086169789, 0.0005339118354150987301, 0.001067817517169160346 ),
 .UNSPECIFIED. ) ;
#23255 = FACE_OUTER_BOUND ( 'NONE', #27754, .T. ) ;
#23256 = B_SPLINE_CURVE_WITH_KNOTS ( 'NONE', 3,
 ( #13999, #20483, #6979, #13859 ),
 .UNSPECIFIED., .F., .F.,
 ( 4, 4 ),
 ( 1.040834085586084257E-17, 0.008383560773332703400 ),
 .UNSPECIFIED. ) ;
#23257 = EDGE_CURVE ( 'NONE', #21489, #25711, #22458, .T. ) ;
#23258 =( BOUNDED_SURFACE ( )  B_SPLINE_SURFACE ( 3, 1, ( 
 ( #6471, #27010 ),
 ( #11345, #9052 ),
 ( #24752, #265 ),
 ( #24613, #2556 ) ),
 .UNSPECIFIED., .F., .F., .F. ) 
 B_SPLINE_SURFACE_WITH_KNOTS ( ( 4, 4 ),
 ( 2, 2 ),
 ( 0.000000000000000000, 1.000000000000000000 ),
 ( 0.000000000000000000, 1.000000000000000000 ),
 .UNSPECIFIED. ) 
 GEOMETRIC_REPRESENTATION_ITEM ( )  RATIONAL_B_SPLINE_SURFACE ( (
 ( 1.000000000000000000, 1.000000000000000000),
 ( 0.9934239774497837239, 0.8357310067453919133),
 ( 0.9934239774497837239, 0.8357310067453919133),
 ( 1.000000000000000000, 1.000000000000000000) ) ) 
 REPRESENTATION_ITEM ( '' )  SURFACE ( )  );
#23259 = CARTESIAN_POINT ( 'NONE',  ( 13.84597867724968445, -146.6243035057531756, -4.782757490007365497 ) ) ;
#23260 = EDGE_CURVE ( 'NONE', #28132, #7273, #11125, .T. ) ;
#23261 = CARTESIAN_POINT ( 'NONE',  ( 109.1721716018069657, 0.007126480965770705736, 0.01550977894512768802 ) ) ;
#23262 = CARTESIAN_POINT ( 'NONE',  ( -20.21097721712958872, 8.835581498567860237, 28.26295595852175779 ) ) ;
#23264 = DIRECTION ( 'NONE',  ( 0.000000000000000000, 5.223019709708233256E-21, -1.000000000000000000 ) ) ;
#23263 = CARTESIAN_POINT ( 'NONE',  ( -23.79223135445719706, -16.82181692922836547, -28.60983116549958538 ) ) ;
#23265 = CARTESIAN_POINT ( 'NONE',  ( 1.833691583653597634, 132.7086741139089838, -58.69608658929788447 ) ) ;
#23266 = ORIENTED_EDGE ( 'NONE', *, *, #22267, .F. ) ;
#23267 = VERTEX_POINT ( 'NONE', #13380 ) ;
#23268 = CARTESIAN_POINT ( 'NONE',  ( 1.831572820252008738, 0.9871191512934829326, -145.1082523917586968 ) ) ;
#23270 = CARTESIAN_POINT ( 'NONE',  ( -28.41354790283022069, -5.969609727607868344, 22.41474081378006744 ) ) ;
#23269 = CARTESIAN_POINT ( 'NONE',  ( -8.259864102781506290, -46.42816643551554989, -25.58601832199090609 ) ) ;
#23271 = CARTESIAN_POINT ( 'NONE',  ( -20.20700224038492365, -8.199606986804534259, -28.44216453106533748 ) ) ;
#23272 = CARTESIAN_POINT ( 'NONE',  ( 109.1592201516379674, -0.004194960840980736620, 0.006649399203953376171 ) ) ;
#23273 = CARTESIAN_POINT ( 'NONE',  ( -20.57838717382308147, -16.28767523336102130, 25.16001208503123365 ) ) ;
#23274 = ORIENTED_EDGE ( 'NONE', *, *, #2874, .T. ) ;
#23275 = CARTESIAN_POINT ( 'NONE',  ( 1.833485406944057594, -58.53321471326971448, 132.7804117027886548 ) ) ;
#23276 = CARTESIAN_POINT ( 'NONE',  ( 1.833603222531955179, -15.61050054119129094, 144.2675221341993677 ) ) ;
#23277 = VERTEX_POINT ( 'NONE', #22626 ) ;
#23278 = DIRECTION ( 'NONE',  ( -0.5914120900931443270, 0.2567974902965093342, 0.7643865440136115019 ) ) ;
#23279 = CARTESIAN_POINT ( 'NONE',  ( -6.574463467970653952, -50.12924290857544918, -11.01561683920031776 ) ) ;
#23280 = ORIENTED_EDGE ( 'NONE', *, *, #25438, .F. ) ;
#23281 = EDGE_LOOP ( 'NONE', ( #23073, #25222, #21134, #12930 ) ) ;
#23282 = EDGE_CURVE ( 'NONE', #3864, #26104, #27282, .T. ) ;
#23283 = ORIENTED_EDGE ( 'NONE', *, *, #9716, .F. ) ;
#23284 = FACE_OUTER_BOUND ( 'NONE', #24063, .T. ) ;
#23285 = EDGE_CURVE ( 'NONE', #2580, #15497, #19382, .T. ) ;
#23286 = B_SPLINE_CURVE_WITH_KNOTS ( 'NONE', 3,
 ( #12982, #21622, #14866, #21912, #3793, #2169, #21773 ),
 .UNSPECIFIED., .F., .F.,
 ( 4, 3, 4 ),
 ( 5.818982450679147801E-16, 0.02816610861753245446, 0.04000277880656277762 ),
 .UNSPECIFIED. ) ;
#23287 = CARTESIAN_POINT ( 'NONE',  ( -1.044556982611269058, -44.03203163107536966, -12.57890920527759171 ) ) ;
#23288 = EDGE_CURVE ( 'NONE', #15570, #8163, #9812, .T. ) ;
#23289 = CARTESIAN_POINT ( 'NONE',  ( -55.25719721206881729, 0.01115102788683056123, 0.0006290797159205457727 ) ) ;
#23290 = CARTESIAN_POINT ( 'NONE',  ( 32.73300124599735739, 55.46353551262010484, 103.7392577722178260 ) ) ;
#23291 = CARTESIAN_POINT ( 'NONE',  ( 1.833838850093517214, 1.355257560975019971E-17, -145.1097630783160923 ) ) ;
#23292 = CARTESIAN_POINT ( 'NONE',  ( -20.47566262905010248, 29.82700878811083811, 1.586617686065662447 ) ) ;
#23293 = EDGE_LOOP ( 'NONE', ( #6071, #26520, #6776, #6954 ) ) ;
#23294 = ADVANCED_FACE ( 'NONE', ( #3176 ), #20287, .F. ) ;
#23295 = CARTESIAN_POINT ( 'NONE',  ( -1.048172774974269084, -13.17853518375268074, 43.86067135048633503 ) ) ;
#23297 = CARTESIAN_POINT ( 'NONE',  ( -1.323439229708141207, -46.01398008004442630, 2.317790194800218195 ) ) ;
#23296 = CARTESIAN_POINT ( 'NONE',  ( 10.93730112725990011, -150.7858122213662000, -10.89264110825150489 ) ) ;
#23298 = CARTESIAN_POINT ( 'NONE',  ( 25.98107933586724272, -102.9042679418245854, -47.01057192495372306 ) ) ;
#23299 = VERTEX_POINT ( 'NONE', #21302 ) ;
#23300 = ORIENTED_EDGE ( 'NONE', *, *, #10680, .F. ) ;
#23301 = VERTEX_POINT ( 'NONE', #8088 ) ;
#23302 = CARTESIAN_POINT ( 'NONE',  ( -20.90916690077960638, 7.054312691028996163, -38.93431874629079203 ) ) ;
#23303 = CARTESIAN_POINT ( 'NONE',  ( -20.20997486282892552, 3.551351076220724598E-15, -29.60348406988233450 ) ) ;
#23305 = CARTESIAN_POINT ( 'NONE',  ( 109.1589550718175161, 0.007359857714025723127, -0.001793588804100419752 ) ) ;
#23304 = CARTESIAN_POINT ( 'NONE',  ( 2.430230287190589422, 144.5585181921888420, -16.65331920325590431 ) ) ;
#23306 = CARTESIAN_POINT ( 'NONE',  ( 2.433796855181233454, -60.50726454507816499, -132.3327394885237425 ) ) ;
#23307 = CARTESIAN_POINT ( 'NONE',  ( 109.1587776205901577, 0.004842060007774048359, 0.005502145856754178839 ) ) ;
#23308 = DIRECTION ( 'NONE',  ( 0.5914120900931444380, 0.3352908775637205574, -0.7333565075147343570 ) ) ;
#23309 =( BOUNDED_SURFACE ( )  B_SPLINE_SURFACE ( 3, 1, ( 
 ( #4858, #20393 ),
 ( #16222, #22727 ),
 ( #5283, #7036 ),
 ( #15933, #9332 ) ),
 .UNSPECIFIED., .F., .F., .F. ) 
 B_SPLINE_SURFACE_WITH_KNOTS ( ( 4, 4 ),
 ( 2, 2 ),
 ( 0.000000000000000000, 1.000000000000000000 ),
 ( 0.000000000000000000, 1.000000000000000000 ),
 .UNSPECIFIED. ) 
 GEOMETRIC_REPRESENTATION_ITEM ( )  RATIONAL_B_SPLINE_SURFACE ( (
 ( 1.000000000000000000, 1.000000000000000000),
 ( 0.9934239774497838349, 0.8357310067453913582),
 ( 0.9934239774497838349, 0.8357310067453913582),
 ( 1.000000000000000000, 1.000000000000000000) ) ) 
 REPRESENTATION_ITEM ( '' )  SURFACE ( )  );
#23310 = CARTESIAN_POINT ( 'NONE',  ( -1.539763995773687499, -29.16712963492436828, 35.94321074656927095 ) ) ;
#23311 = EDGE_LOOP ( 'NONE', ( #24419, #9745, #23110, #6809 ) ) ;
#23312 = CARTESIAN_POINT ( 'NONE',  ( 6.224689322667630975, 136.2818611715198642, -57.86870174583292226 ) ) ;
#23313 = CARTESIAN_POINT ( 'NONE',  ( 19.66333377628710366, -24.23123354948742048, -135.6014041990444809 ) ) ;
#23314 = CARTESIAN_POINT ( 'NONE',  ( -1.046935749540012450, 15.35946454248395376, -43.14401153755472507 ) ) ;
#23315 = DIRECTION ( 'NONE',  ( -0.7563875759206388771, 0.6531865459554675457, -0.03500244528123232224 ) ) ;
#23316 = CARTESIAN_POINT ( 'NONE',  ( -21.41430102051751305, 19.54553566814620069, 23.81424706376344247 ) ) ;
#23317 = CARTESIAN_POINT ( 'NONE',  ( 5.340103579038194326, -108.0219267094752809, 100.3626145943030963 ) ) ;
#23318 = B_SPLINE_CURVE_WITH_KNOTS ( 'NONE', 3,
 ( #21285, #3999, #27773, #14521, #15063, #12773, #25753, #5900, #23753, #25894 ),
 .UNSPECIFIED., .F., .F.,
 ( 4, 2, 2, 2, 4 ),
 ( 2.799429325053882983E-16, 0.0003346187017559026965, 0.0006692374035115254520, 0.001003856105267148099, 0.001338474807022770963 ),
 .UNSPECIFIED. ) ;
#23319 = CARTESIAN_POINT ( 'NONE',  ( 32.73300124599739291, -105.8473486001047235, -51.32617430725011332 ) ) ;
#23320 = VERTEX_POINT ( 'NONE', #1295 ) ;
#23321 = B_SPLINE_CURVE_WITH_KNOTS ( 'NONE', 3,
 ( #25614, #1269, #22893, #12079 ),
 .UNSPECIFIED., .F., .F.,
 ( 4, 4 ),
 ( 0.000000000000000000, 0.01077107196513859763 ),
 .UNSPECIFIED. ) ;
#23322 = CARTESIAN_POINT ( 'NONE',  ( 24.01988960052061728, -31.41104197353406491, 127.2243989116373086 ) ) ;
#23323 = CARTESIAN_POINT ( 'NONE',  ( 2.433796855181233454, 118.5671979538056888, 84.34988187690970562 ) ) ;
#23324 = CARTESIAN_POINT ( 'NONE',  ( 6.224689322667647851, 118.2566963816783101, -89.08920297664090526 ) ) ;
#23325 = ORIENTED_EDGE ( 'NONE', *, *, #21129, .T. ) ;
#23326 = CARTESIAN_POINT ( 'NONE',  ( -20.20700224038492365, 10.08426345511628597, 27.82980252387807951 ) ) ;
#23327 = EDGE_CURVE ( 'NONE', #14914, #10905, #5659, .T. ) ;
#23328 = B_SPLINE_CURVE_WITH_KNOTS ( 'NONE', 3,
 ( #14477, #16501, #7892, #12320, #7602, #9899, #18520, #5861, #16804, #10187 ),
 .UNSPECIFIED., .F., .F.,
 ( 4, 2, 2, 2, 4 ),
 ( 2.845980932296679661E-16, 0.0003346187017559042144, 0.0006692374035115238257, 0.001003856105267143329, 0.001338474807022762940 ),
 .UNSPECIFIED. ) ;
#23329 = EDGE_CURVE ( 'NONE', #7408, #8318, #15536, .T. ) ;
#23330 = CARTESIAN_POINT ( 'NONE',  ( 6.224689322667630975, 126.9212313063844562, 76.23997225729313243 ) ) ;
#23331 = CARTESIAN_POINT ( 'NONE',  ( -8.786685647604890903, -48.22796981442785835, -23.24040270374372952 ) ) ;
#23332 = ADVANCED_FACE ( 'NONE', ( #1584 ), #18446, .F. ) ;
#23333 = CARTESIAN_POINT ( 'NONE',  ( -6.588769196390770411, 50.13301368233300082, -11.07780292579711556 ) ) ;
#23334 = VECTOR ( 'NONE', #21994, 1000.000000000000227 ) ;
#23335 = CARTESIAN_POINT ( 'NONE',  ( -21.41430102051751660, -11.22990201072297012, -28.68859753627389253 ) ) ;
#23336 = CARTESIAN_POINT ( 'NONE',  ( 1.833485406944057594, 142.0485807715645876, 29.64752363041592531 ) ) ;
#23337 = B_SPLINE_CURVE_WITH_KNOTS ( 'NONE', 3,
 ( #16379, #16236, #7475, #18686, #3008, #11924, #27458 ),
 .UNSPECIFIED., .F., .F.,
 ( 4, 3, 4 ),
 ( 0.000000000000000000, 0.006568092053401751972, 0.02506242213020840742 ),
 .UNSPECIFIED. ) ;
#23338 = CARTESIAN_POINT ( 'NONE',  ( 1.833485406944043827, -59.50871042846314651, 132.3460930279889567 ) ) ;
#23339 = CARTESIAN_POINT ( 'NONE',  ( -1.259920593601966177, -16.33409644610522449, 43.01175804832023886 ) ) ;
#23340 = CARTESIAN_POINT ( 'NONE',  ( 10.93730112725982195, -145.2260730187404079, 42.00474393596209666 ) ) ;
#23341 = ORIENTED_EDGE ( 'NONE', *, *, #12479, .F. ) ;
#23342 = ORIENTED_EDGE ( 'NONE', *, *, #11896, .F. ) ;
#23343 = CARTESIAN_POINT ( 'NONE',  ( 1.832998868059890096, -14.63705790013914054, -144.3700883710218648 ) ) ;
#23344 = DIRECTION ( 'NONE',  ( -0.7637818620346800147, -0.6451161201712181104, 0.02150485345384613861 ) ) ;
#23345 = DIRECTION ( 'NONE',  ( 0.5946245182733607137, -0.5401723099040960374, 0.5955128528260720255 ) ) ;
#23346 = CARTESIAN_POINT ( 'NONE',  ( 30.59141879584314694, 26.79785525806573432, -113.0806649571965323 ) ) ;
#23347 = CARTESIAN_POINT ( 'NONE',  ( 26.04756280548352620, -92.21166514879054432, -65.62256188141817859 ) ) ;
#23348 = CARTESIAN_POINT ( 'NONE',  ( -4.473127245936434626, 41.70021447285091654, 26.34600523034491815 ) ) ;
#23349 = LINE ( 'NONE', #3599, #4196 ) ;
#23350 = ORIENTED_EDGE ( 'NONE', *, *, #11966, .T. ) ;
#23351 = CARTESIAN_POINT ( 'NONE',  ( 109.1586900883932856, -0.006130969560687385411, 0.003656351050331833278 ) ) ;
#23352 = CARTESIAN_POINT ( 'NONE',  ( 109.1592201516379674, -0.007376275279030860763, -0.002720803050361382969 ) ) ;
#23353 =( BOUNDED_SURFACE ( )  B_SPLINE_SURFACE ( 3, 1, ( 
 ( #13210, #8764 ),
 ( #26047, #6336 ),
 ( #28329, #17119 ),
 ( #17392, #4159 ) ),
 .UNSPECIFIED., .F., .F., .F. ) 
 B_SPLINE_SURFACE_WITH_KNOTS ( ( 4, 4 ),
 ( 2, 2 ),
 ( 0.000000000000000000, 1.000000000000000000 ),
 ( 0.000000000000000000, 1.000000000000000000 ),
 .UNSPECIFIED. ) 
 GEOMETRIC_REPRESENTATION_ITEM ( )  RATIONAL_B_SPLINE_SURFACE ( (
 ( 1.000000000000000000, 1.000000000000000000),
 ( 0.9960225298536222738, 0.9999952330161893110),
 ( 0.9960225298536222738, 0.9999952330161893110),
 ( 1.000000000000000000, 1.000000000000000000) ) ) 
 REPRESENTATION_ITEM ( '' )  SURFACE ( )  );
#23354 = CARTESIAN_POINT ( 'NONE',  ( 26.11404676487257603, -74.91683232331033082, 84.89295829319468112 ) ) ;
#23355 = CARTESIAN_POINT ( 'NONE',  ( -12.94347594948481195, 8.691477019903993906, 47.96504705787742040 ) ) ;
#23356 = DIRECTION ( 'NONE',  ( 0.000000000000000000, -1.000000000000000000, 0.000000000000000000 ) ) ;
#23357 = CARTESIAN_POINT ( 'NONE',  ( 109.1586900883932856, 0.001385221016527459588, -0.007002774699553642249 ) ) ;
#23358 = ORIENTED_EDGE ( 'NONE', *, *, #24311, .F. ) ;
#23359 = CARTESIAN_POINT ( 'NONE',  ( 26.11404676487257603, -57.58742681967381571, -97.48350837663670632 ) ) ;
#23360 = CARTESIAN_POINT ( 'NONE',  ( 55.49584447822657296, -72.55110015779771970, -0.2676470673964289615 ) ) ;
#23361 = ORIENTED_EDGE ( 'NONE', *, *, #4999, .F. ) ;
#23362 = EDGE_LOOP ( 'NONE', ( #27634, #1370, #17397, #6844 ) ) ;
#23363 = VERTEX_POINT ( 'NONE', #14100 ) ;
#23364 = EDGE_CURVE ( 'NONE', #25194, #6927, #21742, .T. ) ;
#23365 = CARTESIAN_POINT ( 'NONE',  ( 25.64704443564078318, -110.4160069635932331, -23.60610532597069877 ) ) ;
#23366 = CARTESIAN_POINT ( 'NONE',  ( -55.25297051322618813, -0.01466904165775103838, -0.002853887643042541354 ) ) ;
#23367 = EDGE_CURVE ( 'NONE', #1868, #17200, #8675, .T. ) ;
#23368 = CARTESIAN_POINT ( 'NONE',  ( 1.831572820252008738, -58.11906524360392012, -132.9644823688601321 ) ) ;
#23369 = EDGE_CURVE ( 'NONE', #9124, #21691, #3522, .T. ) ;
#23370 = B_SPLINE_CURVE_WITH_KNOTS ( 'NONE', 3,
 ( #3350, #23237, #22804, #9988 ),
 .UNSPECIFIED., .F., .F.,
 ( 4, 4 ),
 ( 0.000000000000000000, 0.01077107196513872600 ),
 .UNSPECIFIED. ) ;
#23371 = CARTESIAN_POINT ( 'NONE',  ( 6.224689322667647851, -2.565137105442716781, -148.0369967195763081 ) ) ;
#23372 = CARTESIAN_POINT ( 'NONE',  ( -1.019300379054419947, 12.21833869579527310, 44.15350047934384747 ) ) ;
#23373 = CARTESIAN_POINT ( 'NONE',  ( -1.058473599757816297, 45.77379534793244886, -1.755404039369589997 ) ) ;
#23374 = CARTESIAN_POINT ( 'NONE',  ( -12.82751273423882665, 48.09651489336691554, 8.715310691359739792 ) ) ;
#23375 = CARTESIAN_POINT ( 'NONE',  ( 32.73300124599735739, 39.98094346392311138, 110.6325518752275485 ) ) ;
#23376 = CARTESIAN_POINT ( 'NONE',  ( 10.93730112725972425, -79.81734490845995822, 128.3908183996588264 ) ) ;
#23377 = B_SPLINE_CURVE_WITH_KNOTS ( 'NONE', 3,
 ( #15410, #26499, #17721, #26926, #6951, #24221 ),
 .UNSPECIFIED., .F., .F.,
 ( 4, 2, 4 ),
 ( 1.550807859811640467E-16, 0.003570751334075634390, 0.007141502668151113523 ),
 .UNSPECIFIED. ) ;
#23378 = CARTESIAN_POINT ( 'NONE',  ( 2.433796855181219243, -145.5024947199069913, 1.451562450949123395 ) ) ;
#23379 = DIRECTION ( 'NONE',  ( -1.000000000000000000, -0.000000000000000000, -0.000000000000000000 ) ) ;
#23380 = CARTESIAN_POINT ( 'NONE',  ( 6.224689322667630975, -146.9579047224768260, -18.02516478984294324 ) ) ;
#23381 = FACE_OUTER_BOUND ( 'NONE', #18968, .T. ) ;
#23382 = CARTESIAN_POINT ( 'NONE',  ( 24.01988960052057465, 130.7041393974935772, -9.440825210282081770 ) ) ;
#23383 = CARTESIAN_POINT ( 'NONE',  ( -1.583189561560253589, 43.29471907393742214, -16.68617981233717629 ) ) ;
#23384 = ORIENTED_EDGE ( 'NONE', *, *, #8553, .T. ) ;
#23385 = ORIENTED_EDGE ( 'NONE', *, *, #1369, .F. ) ;
#23386 = CARTESIAN_POINT ( 'NONE',  ( 30.59138290137879324, -21.51300488027205660, 114.2039707400270885 ) ) ;
#23387 =( BOUNDED_SURFACE ( )  B_SPLINE_SURFACE ( 3, 1, ( 
 ( #22423, #2541 ),
 ( #11191, #4421 ),
 ( #2246, #19818 ),
 ( #107, #22130 ) ),
 .UNSPECIFIED., .F., .F., .F. ) 
 B_SPLINE_SURFACE_WITH_KNOTS ( ( 4, 4 ),
 ( 2, 2 ),
 ( 0.000000000000000000, 1.000000000000000000 ),
 ( 0.000000000000000000, 1.000000000000000000 ),
 .UNSPECIFIED. ) 
 GEOMETRIC_REPRESENTATION_ITEM ( )  RATIONAL_B_SPLINE_SURFACE ( (
 ( 1.000000000000000000, 1.000000000000000000),
 ( 0.7789835883360578528, 0.9689951854195403280),
 ( 0.7789835883360578528, 0.9689951854195403280),
 ( 1.000000000000000000, 1.000000000000000000) ) ) 
 REPRESENTATION_ITEM ( '' )  SURFACE ( )  );
#23388 = CARTESIAN_POINT ( 'NONE',  ( -1.046935749539996907, 25.87617179820970748, 37.78548154587966934 ) ) ;
#23389 = ORIENTED_EDGE ( 'NONE', *, *, #27460, .F. ) ;
#23390 = PRODUCT_DEFINITION ( 'UNKNOWN', '', #21775, #11698 ) ;
#23391 = VERTEX_POINT ( 'NONE', #5628 ) ;
#23392 = ORIENTED_EDGE ( 'NONE', *, *, #3759, .T. ) ;
#23393 = ADVANCED_FACE ( 'NONE', ( #19147 ), #7446, .F. ) ;
#23394 =( BOUNDED_SURFACE ( )  B_SPLINE_SURFACE ( 3, 1, ( 
 ( #3786, #21044 ),
 ( #8123, #12556 ),
 ( #23100, #1200 ),
 ( #25246, #5514 ) ),
 .UNSPECIFIED., .F., .F., .F. ) 
 B_SPLINE_SURFACE_WITH_KNOTS ( ( 4, 4 ),
 ( 2, 2 ),
 ( 0.000000000000000000, 1.000000000000000000 ),
 ( 0.000000000000000000, 1.000000000000000000 ),
 .UNSPECIFIED. ) 
 GEOMETRIC_REPRESENTATION_ITEM ( )  RATIONAL_B_SPLINE_SURFACE ( (
 ( 1.000000000000000000, 1.000000000000000000),
 ( 0.9593753223639863714, 0.9995975284513187731),
 ( 0.9593753223639863714, 0.9995975284513187731),
 ( 1.000000000000000000, 1.000000000000000000) ) ) 
 REPRESENTATION_ITEM ( '' )  SURFACE ( )  );
#23395 = CARTESIAN_POINT ( 'NONE',  ( -21.41430102051744910, 7.777552968935758315, -29.81033373822130628 ) ) ;
#23396 = CARTESIAN_POINT ( 'NONE',  ( -55.24271866751342941, 0.001425019990782615698, -0.009388511352197861579 ) ) ;
#23397 = DIRECTION ( 'NONE',  ( 0.7563875759206388771, -0.6104009704506944134, -0.2351350468682844030 ) ) ;
#23398 = CARTESIAN_POINT ( 'NONE',  ( 8.186469829614464899, 146.7694295239429607, -27.65107825763805849 ) ) ;
#23399 = CARTESIAN_POINT ( 'NONE',  ( 109.1586900883932856, -0.001582822706032874097, -0.006960773163852184385 ) ) ;
#23400 = CARTESIAN_POINT ( 'NONE',  ( -1.050230346682673677, -14.15203301556463167, -43.55772679531845881 ) ) ;
#23401 = CARTESIAN_POINT ( 'NONE',  ( 1.833838850855474600, 132.6005571022087395, -58.94016894581336885 ) ) ;
#23402 = EDGE_LOOP ( 'NONE', ( #18839, #17787, #15189, #11045 ) ) ;
#23403 = VERTEX_POINT ( 'NONE', #10929 ) ;
#23404 = DIRECTION ( 'NONE',  ( 0.000000000000000000, 0.000000000000000000, 1.000000000000000000 ) ) ;
#23406 = CARTESIAN_POINT ( 'NONE',  ( 9.884929003653626367, -128.2151425008046886, 78.87917189084865299 ) ) ;
#23405 = CARTESIAN_POINT ( 'NONE',  ( -25.21435515916025594, 1.749597353048488237E-16, -4.373993382621220594E-17 ) ) ;
#23407 = CARTESIAN_POINT ( 'NONE',  ( 10.93730112725932635, 0.000000000000000000, 0.000000000000000000 ) ) ;
#23408 = CARTESIAN_POINT ( 'NONE',  ( 1.833485406944043827, -72.09189602597619739, -125.9346397303442728 ) ) ;
#23409 = EDGE_LOOP ( 'NONE', ( #8304, #12521, #23816, #7604 ) ) ;
#23410 = CARTESIAN_POINT ( 'NONE',  ( -4.473127245936434626, -3.196405119334147837, -49.22197550883366546 ) ) ;
#23411 = FACE_OUTER_BOUND ( 'NONE', #12653, .T. ) ;
#23412 = CARTESIAN_POINT ( 'NONE',  ( 28.43349137099854929, 122.3147591366313947, 21.85613782299017416 ) ) ;
#23413 = ORIENTED_EDGE ( 'NONE', *, *, #27558, .T. ) ;
#23414 = ORIENTED_EDGE ( 'NONE', *, *, #423, .F. ) ;
#23415 = CARTESIAN_POINT ( 'NONE',  ( 2.063896406836605024, -125.1295119249434009, -73.79559738457884066 ) ) ;
#23416 = EDGE_CURVE ( 'NONE', #14330, #1523, #2136, .T. ) ;
#23417 = ORIENTED_EDGE ( 'NONE', *, *, #12117, .F. ) ;
#23418 = VERTEX_POINT ( 'NONE', #4305 ) ;
#23419 = EDGE_CURVE ( 'NONE', #27426, #15681, #5947, .T. ) ;
#23420 = EDGE_CURVE ( 'NONE', #13048, #14557, #28241, .T. ) ;
#23421 = CARTESIAN_POINT ( 'NONE',  ( 1.833750490713699444, 96.89879583303846289, 108.0159692407134031 ) ) ;
#23422 =( BOUNDED_SURFACE ( )  B_SPLINE_SURFACE ( 3, 1, ( 
 ( #22960, #5674 ),
 ( #27681, #3498 ),
 ( #1338, #12282 ),
 ( #21048, #10141 ) ),
 .UNSPECIFIED., .F., .F., .F. ) 
 B_SPLINE_SURFACE_WITH_KNOTS ( ( 4, 4 ),
 ( 2, 2 ),
 ( 0.000000000000000000, 1.000000000000000000 ),
 ( 0.000000000000000000, 1.000000000000000000 ),
 .UNSPECIFIED. ) 
 GEOMETRIC_REPRESENTATION_ITEM ( )  RATIONAL_B_SPLINE_SURFACE ( (
 ( 1.000000000000000000, 1.000000000000000000),
 ( 0.6386103224230316178, 0.9954351624131538845),
 ( 0.6386103224230316178, 0.9954351624131538845),
 ( 1.000000000000000000, 1.000000000000000000) ) ) 
 REPRESENTATION_ITEM ( '' )  SURFACE ( )  );
#23423 = ORIENTED_EDGE ( 'NONE', *, *, #25410, .F. ) ;
#23424 = FACE_OUTER_BOUND ( 'NONE', #26419, .T. ) ;
#23425 = CARTESIAN_POINT ( 'NONE',  ( -12.82751273423881777, 43.04932478553568842, 23.15139349681263070 ) ) ;
#23426 = DIRECTION ( 'NONE',  ( -0.5914120900931443270, 0.4674599267565434091, -0.6570486713847197846 ) ) ;
#23427 = CARTESIAN_POINT ( 'NONE',  ( -20.20700224038492721, -29.58392382092674211, -0.9908225410477480288 ) ) ;
#23428 = CARTESIAN_POINT ( 'NONE',  ( 109.1624594426973118, -0.009754804742280876254, -0.01263706729759555072 ) ) ;
#23429 = CARTESIAN_POINT ( 'NONE',  ( 13.84597867724978570, 137.9700459519987703, 49.85807424839799040 ) ) ;
#23430 = CARTESIAN_POINT ( 'NONE',  ( -1.583189561560252701, 44.83405390829673109, -11.94859433442916874 ) ) ;
#23432 = CARTESIAN_POINT ( 'NONE',  ( 6.224689322667647851, -139.9988794244335679, 48.18553814189983342 ) ) ;
#23431 = CARTESIAN_POINT ( 'NONE',  ( 25.64699802086724745, -97.90265915239990591, -56.24956056770124491 ) ) ;
#23433 = AXIS2_PLACEMENT_3D ( 'NONE', #27454, #1400, #12207 ) ;
#23434 = CARTESIAN_POINT ( 'NONE',  ( -20.57838717382308147, -1.611677988432568709, -29.92853265176830746 ) ) ;
#23435 = ORIENTED_EDGE ( 'NONE', *, *, #15590, .T. ) ;
#23436 = EDGE_LOOP ( 'NONE', ( #12988, #10217, #12765, #22914 ) ) ;
#23437 = CARTESIAN_POINT ( 'NONE',  ( -55.24271866751342941, -0.006671293903667674559, -0.006757859501010194010 ) ) ;
#23438 = CARTESIAN_POINT ( 'NONE',  ( 13.84597867724998999, 82.31427113894766023, 121.4327876424614772 ) ) ;
#23440 = CARTESIAN_POINT ( 'NONE',  ( 25.70243777736189017, -98.18050844655108733, 55.83795591307098505 ) ) ;
#23439 = CARTESIAN_POINT ( 'NONE',  ( 55.49584447822657296, -62.69727227546427173, 36.50733923851176144 ) ) ;
#23441 = CARTESIAN_POINT ( 'NONE',  ( -1.019300379054419725, -44.15350047934408195, -12.21833869579447729 ) ) ;
#23442 = LINE ( 'NONE', #9919, #5643 ) ;
#23443 = VERTEX_POINT ( 'NONE', #6065 ) ;
#23444 = CARTESIAN_POINT ( 'NONE',  ( -1.155001620486248992, 12.20337535396741124, 44.25209926692296136 ) ) ;
#23445 = CARTESIAN_POINT ( 'NONE',  ( -8.786685647604896232, -7.199674155858612146, 53.04920435127190359 ) ) ;
#23446 = ORIENTED_EDGE ( 'NONE', *, *, #14979, .F. ) ;
#23447 = CARTESIAN_POINT ( 'NONE',  ( 1.894214914920993698, -0.9536781033349790437, -145.1469726764543964 ) ) ;
#23448 = CARTESIAN_POINT ( 'NONE',  ( 25.64704443564080094, -112.3065506427462168, 11.66968230815876950 ) ) ;
#23449 = CARTESIAN_POINT ( 'NONE',  ( 109.1778270068192853, 0.003210287141656879405, -0.008743876326153473405 ) ) ;
#23450 = EDGE_CURVE ( 'NONE', #7920, #20945, #23904, .T. ) ;
#23451 = CARTESIAN_POINT ( 'NONE',  ( 13.36082413113063083, 97.52406103376918622, -117.7941133658628559 ) ) ;
#23452 = CARTESIAN_POINT ( 'NONE',  ( -7.078251931573400491, 38.93060825814280435, 34.59014398252872269 ) ) ;
#23453 = CARTESIAN_POINT ( 'NONE',  ( 25.65782528836479770, -110.5695798068304896, 22.91156770660766284 ) ) ;
#23454 = B_SPLINE_CURVE_WITH_KNOTS ( 'NONE', 3,
 ( #4458, #4599, #19716, #17416, #11230, #24338, #4326, #21890 ),
 .UNSPECIFIED., .F., .F.,
 ( 4, 2, 2, 4 ),
 ( 2.194186273941487449E-16, 0.002761568181852863766, 0.005523136363705508090, 0.01104627272741078893 ),
 .UNSPECIFIED. ) ;
#23455 = CARTESIAN_POINT ( 'NONE',  ( -8.786685647604894456, 37.00619870957989832, 38.68584556812258768 ) ) ;
#23456 = ORIENTED_EDGE ( 'NONE', *, *, #2831, .F. ) ;
#23457 = CARTESIAN_POINT ( 'NONE',  ( 6.224689322667647851, 12.92299475787155316, -147.4941644018826992 ) ) ;
#23458 = EDGE_CURVE ( 'NONE', #1490, #22412, #28054, .T. ) ;
#23459 = EDGE_CURVE ( 'NONE', #21625, #13254, #7309, .T. ) ;
#23460 = FACE_OUTER_BOUND ( 'NONE', #5965, .T. ) ;
#23461 = B_SPLINE_CURVE_WITH_KNOTS ( 'NONE', 3,
 ( #2132, #28337, #15095, #8774, #6074, #11075, #28202, #8503, #4168, #26325 ),
 .UNSPECIFIED., .F., .F.,
 ( 4, 3, 3, 4 ),
 ( 6.938893903907228378E-18, 0.0002669560319015663462, 0.0005492286108966397190, 0.0008315040496093490177 ),
 .UNSPECIFIED. ) ;
#23462 = EDGE_LOOP ( 'NONE', ( #22221, #21651, #22197, #23417 ) ) ;
#23463 = CARTESIAN_POINT ( 'NONE',  ( 1.833485406944043827, 117.0814567582544612, 85.72460230293732764 ) ) ;
#23464 = ORIENTED_EDGE ( 'NONE', *, *, #19363, .T. ) ;
#23465 = ORIENTED_EDGE ( 'NONE', *, *, #3537, .F. ) ;
#23466 = CARTESIAN_POINT ( 'NONE',  ( -20.57838717382308147, -18.89542499756482741, 23.26537097894125594 ) ) ;
#23467 = CARTESIAN_POINT ( 'NONE',  ( 1.832998868059858122, -73.01698022778271024, -125.4013017422238363 ) ) ;
#23468 = CARTESIAN_POINT ( 'NONE',  ( -1.049819825607573254, -13.66706894614408618, 43.71263398674766876 ) ) ;
#23469 = DIRECTION ( 'NONE',  ( -0.7563875759206388771, 0.3556158456312860094, -0.5490129373055293582 ) ) ;
#23470 = CARTESIAN_POINT ( 'NONE',  ( 32.73300124599739291, 55.46353551262154014, -103.7392577722169875 ) ) ;
#23471 = CARTESIAN_POINT ( 'NONE',  ( 30.59138290137882521, -55.75105126023986912, 101.9665464510085400 ) ) ;
#23472 = CARTESIAN_POINT ( 'NONE',  ( -25.21435515916043713, 15.02493970636190745, 31.17620025257570759 ) ) ;
#23473 =( BOUNDED_SURFACE ( )  B_SPLINE_SURFACE ( 3, 1, ( 
 ( #2394, #11192 ),
 ( #13626, #19966 ),
 ( #24445, #4711 ),
 ( #12191, #1244 ) ),
 .UNSPECIFIED., .F., .F., .F. ) 
 B_SPLINE_SURFACE_WITH_KNOTS ( ( 4, 4 ),
 ( 2, 2 ),
 ( 0.000000000000000000, 1.000000000000000000 ),
 ( 0.000000000000000000, 1.000000000000000000 ),
 .UNSPECIFIED. ) 
 GEOMETRIC_REPRESENTATION_ITEM ( )  RATIONAL_B_SPLINE_SURFACE ( (
 ( 1.000000000000000000, 1.000000000000000000),
 ( 0.7789835883360578528, 0.9689951854195403280),
 ( 0.7789835883360578528, 0.9689951854195403280),
 ( 1.000000000000000000, 1.000000000000000000) ) ) 
 REPRESENTATION_ITEM ( '' )  SURFACE ( )  );
#23474 = CARTESIAN_POINT ( 'NONE',  ( 25.69398547355838858, -75.02007992711763507, 84.42756928260550353 ) ) ;
#23475 = CARTESIAN_POINT ( 'NONE',  ( 25.64692872815576052, 35.19724814978057026, -107.2850779876530822 ) ) ;
#23476 = ORIENTED_EDGE ( 'NONE', *, *, #9535, .F. ) ;
#23477 = VERTEX_POINT ( 'NONE', #17533 ) ;
#23478 = CARTESIAN_POINT ( 'NONE',  ( 13.36082413113063083, 56.35051087435157058, -142.1654513177082606 ) ) ;
#23479 = CARTESIAN_POINT ( 'NONE',  ( -1.045287976400351981, 43.05558670614237116, -15.59869763335110449 ) ) ;
#23480 = CARTESIAN_POINT ( 'NONE',  ( 1.834118845439484335, 132.6369225636082376, -58.85894970554785743 ) ) ;
#23481 = CONICAL_SURFACE ( 'NONE', #23034, 117.6351876552689504, 0.9945805576725580410 ) ;
#23482 = CARTESIAN_POINT ( 'NONE',  ( 1.893872463202030731, 144.2520230501565948, 16.11957794552817802 ) ) ;
#23483 = CARTESIAN_POINT ( 'NONE',  ( -1.044557008772713402, 43.01636061109007159, 15.70482370518772086 ) ) ;
#23484 = LINE ( 'NONE', #10800, #22230 ) ;
#23485 = CARTESIAN_POINT ( 'NONE',  ( -55.24271866751342941, 0.008433070970614256479, -0.004365563123935527895 ) ) ;
#23486 = ORIENTED_EDGE ( 'NONE', *, *, #23914, .F. ) ;
#23487 = CARTESIAN_POINT ( 'NONE',  ( 1.832998868059858122, 107.4798986104872967, -97.49378069860692619 ) ) ;
#23488 = CARTESIAN_POINT ( 'NONE',  ( -1.048172774974297949, -37.64158596421231096, -26.08722459372772562 ) ) ;
#23489 = EDGE_CURVE ( 'NONE', #21261, #7427, #19281, .T. ) ;
#23490 = B_SPLINE_CURVE_WITH_KNOTS ( 'NONE', 3,
 ( #27074, #14671, #26939, #27784, #7384, #23474, #22800, #10381 ),
 .UNSPECIFIED., .F., .F.,
 ( 4, 2, 2, 4 ),
 ( 0.000000000000000000, 0.0002429592666046789557, 0.0004859185332093579114, 0.0009718370664186629137 ),
 .UNSPECIFIED. ) ;
#23491 = EDGE_CURVE ( 'NONE', #5899, #17261, #13822, .T. ) ;
#23492 = CARTESIAN_POINT ( 'NONE',  ( 25.69398547355840634, 0.7422864227365167933, 112.9401428107247511 ) ) ;
#23493 = CARTESIAN_POINT ( 'NONE',  ( 25.64707127832795663, 0.04449220797125042620, -112.9112343549835487 ) ) ;
#23494 = ORIENTED_EDGE ( 'NONE', *, *, #19775, .T. ) ;
#23496 = EDGE_CURVE ( 'NONE', #18704, #25954, #6335, .T. ) ;
#23495 = CARTESIAN_POINT ( 'NONE',  ( 25.64700659047694131, -46.13293552475862214, 103.0567718204600709 ) ) ;
#23497 = CARTESIAN_POINT ( 'NONE',  ( -1.050230347360791017, 0.0004630652117437840452, -45.79907861464602092 ) ) ;
#23498 = VERTEX_POINT ( 'NONE', #10513 ) ;
#23499 = EDGE_CURVE ( 'NONE', #1086, #12213, #1147, .T. ) ;
#23500 = ORIENTED_EDGE ( 'NONE', *, *, #7445, .F. ) ;
#23501 = ORIENTED_EDGE ( 'NONE', *, *, #14422, .F. ) ;
#23502 = CIRCLE ( 'NONE', #4601, 34.60786435723138510 ) ;
#23503 = AXIS2_PLACEMENT_3D ( 'NONE', #349, #19544, #12776 ) ;
#23504 = CARTESIAN_POINT ( 'NONE',  ( 2.108393763691202238, 28.95405853987516664, 142.3786741588520499 ) ) ;
#23505 = CARTESIAN_POINT ( 'NONE',  ( -4.473127245936431073, -18.25038884639838699, 45.82513704981563052 ) ) ;
#23506 = AXIS2_PLACEMENT_3D ( 'NONE', #27372, #16999, #25224 ) ;
#23507 = B_SPLINE_CURVE_WITH_KNOTS ( 'NONE', 3,
 ( #15349, #19813, #10910, #1831 ),
 .UNSPECIFIED., .F., .F.,
 ( 4, 4 ),
 ( 4.443059973708341306E-17, 0.008383748772659519594 ),
 .UNSPECIFIED. ) ;
#23508 = DIRECTION ( 'NONE',  ( -1.000000000000000000, -0.000000000000000000, -0.000000000000000000 ) ) ;
#23509 =( BOUNDED_SURFACE ( )  B_SPLINE_SURFACE ( 3, 1, ( 
 ( #7061, #25184 ),
 ( #7486, #9788 ),
 ( #22453, #24768 ),
 ( #13794, #7337 ) ),
 .UNSPECIFIED., .F., .F., .F. ) 
 B_SPLINE_SURFACE_WITH_KNOTS ( ( 4, 4 ),
 ( 2, 2 ),
 ( 0.000000000000000000, 1.000000000000000000 ),
 ( 0.000000000000000000, 1.000000000000000000 ),
 .UNSPECIFIED. ) 
 GEOMETRIC_REPRESENTATION_ITEM ( )  RATIONAL_B_SPLINE_SURFACE ( (
 ( 1.000000000000000000, 1.000000000000000000),
 ( 0.9960225298536222738, 0.9999952330161893110),
 ( 0.9960225298536222738, 0.9999952330161893110),
 ( 1.000000000000000000, 1.000000000000000000) ) ) 
 REPRESENTATION_ITEM ( '' )  SURFACE ( )  );
#23510 = VERTEX_POINT ( 'NONE', #17118 ) ;
#23511 = CARTESIAN_POINT ( 'NONE',  ( 109.1721716018069515, 0.01695288006056418911, 0.001984900887706716240 ) ) ;
#23512 = CARTESIAN_POINT ( 'NONE',  ( 26.11404676487257603, -24.64483677384923865, 110.5078194225160360 ) ) ;
#23513 = CARTESIAN_POINT ( 'NONE',  ( -8.786685647604896232, -7.199674155858612146, 53.04920435127190359 ) ) ;
#23514 = CARTESIAN_POINT ( 'NONE',  ( 109.1586059443104944, -0.006971743774739767863, -0.001198897580738971869 ) ) ;
#23515 = CARTESIAN_POINT ( 'NONE',  ( 9.884929003653626367, 50.49804566712126075, 141.8132360130359757 ) ) ;
#23516 = AXIS2_PLACEMENT_3D ( 'NONE', #13248, #19729, #21905 ) ;
#23517 = B_SPLINE_CURVE_WITH_KNOTS ( 'NONE', 3,
 ( #17955, #7055, #15814, #12486 ),
 .UNSPECIFIED., .F., .F.,
 ( 4, 4 ),
 ( 3.428463280104494194E-16, 0.01077107486149824628 ),
 .UNSPECIFIED. ) ;
#23518 = CARTESIAN_POINT ( 'NONE',  ( 109.1589550718175161, -0.0005685167901217975548, 0.007553890059316982486 ) ) ;
#23519 = ADVANCED_FACE ( 'NONE', ( #10796 ), #23258, .F. ) ;
#23520 = VECTOR ( 'NONE', #23827, 1000.000000000000000 ) ;
#23521 = CARTESIAN_POINT ( 'NONE',  ( -9.156249394959706578, -8.027840202793560920, 53.90509764945136340 ) ) ;
#23522 = CARTESIAN_POINT ( 'NONE',  ( 8.186469777910977186, 127.5731248346298514, -77.65916160569786086 ) ) ;
#23523 = CARTESIAN_POINT ( 'NONE',  ( -20.20700224038492365, 23.35150625415685255, 18.19058640100197977 ) ) ;
#23524 = CARTESIAN_POINT ( 'NONE',  ( 1.832998868059858122, 73.01698022778357711, 125.4013017422233247 ) ) ;
#23525 = CARTESIAN_POINT ( 'NONE',  ( 10.93730112725990189, -148.8212007290660495, -26.59437931460901439 ) ) ;
#23526 = ORIENTED_EDGE ( 'NONE', *, *, #24837, .T. ) ;
#23527 = VECTOR ( 'NONE', #26410, 1000.000000000000000 ) ;
#23528 = ORIENTED_EDGE ( 'NONE', *, *, #25442, .T. ) ;
#23530 = EDGE_CURVE ( 'NONE', #26730, #20281, #2498, .T. ) ;
#23529 = CARTESIAN_POINT ( 'NONE',  ( 10.93730112725969938, 79.81734490845904872, 128.3908183996593948 ) ) ;
#23531 = CARTESIAN_POINT ( 'NONE',  ( 32.73300124599732186, 0.000000000000000000, 0.000000000000000000 ) ) ;
#23532 = ORIENTED_EDGE ( 'NONE', *, *, #14319, .T. ) ;
#23533 = ORIENTED_EDGE ( 'NONE', *, *, #1473, .T. ) ;
#23534 = ORIENTED_EDGE ( 'NONE', *, *, #23416, .F. ) ;
#23535 = CARTESIAN_POINT ( 'NONE',  ( -1.046936909428682672, 43.93225665392633061, 12.93351869073227611 ) ) ;
#23536 = AXIS2_PLACEMENT_3D ( 'NONE', #10780, #4283, #13484 ) ;
#23537 = CARTESIAN_POINT ( 'NONE',  ( -22.34422965417124018, -26.20925041532873223, -27.39717383755272451 ) ) ;
#23538 = AXIS2_PLACEMENT_3D ( 'NONE', #4441, #17956, #15815 ) ;
#23539 = CARTESIAN_POINT ( 'NONE',  ( -20.24419206586954090, 27.76448493191444200, -10.37009329716774708 ) ) ;
#23540 = CARTESIAN_POINT ( 'NONE',  ( 55.79472521941428198, -63.36760613016198818, -35.74479459808913617 ) ) ;
#23541 = DIRECTION ( 'NONE',  ( 0.7071067811865485719, 0.000000000000000000, 0.7071067811865465735 ) ) ;
#23542 = CARTESIAN_POINT ( 'NONE',  ( 1.833485406944057594, -117.7091014914944225, -84.86072343962690923 ) ) ;
#23543 = ORIENTED_EDGE ( 'NONE', *, *, #9975, .F. ) ;
#23544 =( BOUNDED_SURFACE ( )  B_SPLINE_SURFACE ( 3, 1, ( 
 ( #22056, #26652 ),
 ( #2179, #466 ),
 ( #26231, #10989 ),
 ( #9256, #11549 ) ),
 .UNSPECIFIED., .F., .F., .F. ) 
 B_SPLINE_SURFACE_WITH_KNOTS ( ( 4, 4 ),
 ( 2, 2 ),
 ( 0.000000000000000000, 1.000000000000000000 ),
 ( 0.000000000000000000, 1.000000000000000000 ),
 .UNSPECIFIED. ) 
 GEOMETRIC_REPRESENTATION_ITEM ( )  RATIONAL_B_SPLINE_SURFACE ( (
 ( 1.000000000000000000, 1.000000000000000000),
 ( 0.7789835883360578528, 0.9689951854195403280),
 ( 0.7789835883360578528, 0.9689951854195403280),
 ( 1.000000000000000000, 1.000000000000000000) ) ) 
 REPRESENTATION_ITEM ( '' )  SURFACE ( )  );
#23545 = VERTEX_POINT ( 'NONE', #8917 ) ;
#23546 = CARTESIAN_POINT ( 'NONE',  ( -1.048996300304503082, -26.29666317565274980, 37.49570739463913327 ) ) ;
#23548 = PLANE ( 'NONE',  #5044 ) ;
#23547 = CARTESIAN_POINT ( 'NONE',  ( 1.832998868059890096, -30.69214149073911457, -141.8272129421612249 ) ) ;
#23549 = EDGE_CURVE ( 'NONE', #457, #12820, #9702, .T. ) ;
#23550 = CARTESIAN_POINT ( 'NONE',  ( 25.64704443564079384, -103.0951670221011511, -46.04703398841390793 ) ) ;
#23551 = CARTESIAN_POINT ( 'NONE',  ( 55.49584447822657296, -7.849835876628820763, 72.12568090333340365 ) ) ;
#23552 = CARTESIAN_POINT ( 'NONE',  ( 25.65782528836480125, 91.69136324939191240, -65.90345832277380111 ) ) ;
#23553 = ORIENTED_EDGE ( 'NONE', *, *, #9861, .F. ) ;
#23554 = CARTESIAN_POINT ( 'NONE',  ( 2.263178607246734142, 137.8402782326817260, -46.26071628252303469 ) ) ;
#23556 = EDGE_CURVE ( 'NONE', #2493, #8511, #5003, .T. ) ;
#23555 = CARTESIAN_POINT ( 'NONE',  ( 2.263178113027036975, -144.4462808674009295, -16.59120315151724867 ) ) ;
#23557 = CARTESIAN_POINT ( 'NONE',  ( 1.833750490713699444, -15.43355859895757298, 144.2866297127913242 ) ) ;
#23558 = ORIENTED_EDGE ( 'NONE', *, *, #22711, .T. ) ;
#23559 = B_SPLINE_CURVE_WITH_KNOTS ( 'NONE', 3,
 ( #20537, #17935, #9605, #25028, #20828, #27738, #7899 ),
 .UNSPECIFIED., .F., .F.,
 ( 4, 3, 4 ),
 ( 0.000000000000000000, 0.02398743853561352210, 0.04000277880656211149 ),
 .UNSPECIFIED. ) ;
#23560 = ORIENTED_EDGE ( 'NONE', *, *, #2222, .T. ) ;
#23561 = EDGE_CURVE ( 'NONE', #25702, #607, #17807, .T. ) ;
#23562 = CARTESIAN_POINT ( 'NONE',  ( 14.74894986621300319, -1.023413983156987147E-16, 2.558534957892467869E-17 ) ) ;
#23564 =( BOUNDED_SURFACE ( )  B_SPLINE_SURFACE ( 3, 1, ( 
 ( #18735, #27507 ),
 ( #3472, #1312 ),
 ( #10112, #18877 ),
 ( #27651, #16732 ) ),
 .UNSPECIFIED., .F., .F., .F. ) 
 B_SPLINE_SURFACE_WITH_KNOTS ( ( 4, 4 ),
 ( 2, 2 ),
 ( 0.000000000000000000, 1.000000000000000000 ),
 ( 0.000000000000000000, 1.000000000000000000 ),
 .UNSPECIFIED. ) 
 GEOMETRIC_REPRESENTATION_ITEM ( )  RATIONAL_B_SPLINE_SURFACE ( (
 ( 1.000000000000000000, 1.000000000000000000),
 ( 0.9956975270656954757, 0.8568959468854893125),
 ( 0.9956975270656954757, 0.8568959468854893125),
 ( 1.000000000000000000, 1.000000000000000000) ) ) 
 REPRESENTATION_ITEM ( '' )  SURFACE ( )  );
#23563 = AXIS2_PLACEMENT_3D ( 'NONE', #20479, #24684, #2330 ) ;
#23565 = ORIENTED_EDGE ( 'NONE', *, *, #13369, .T. ) ;
#23566 = AXIS2_PLACEMENT_3D ( 'NONE', #25530, #27666, #12685 ) ;
#23567 = EDGE_LOOP ( 'NONE', ( #1123, #15271, #19934, #3407 ) ) ;
#23568 = ADVANCED_FACE ( 'NONE', ( #19980 ), #12560, .F. ) ;
#23569 = EDGE_CURVE ( 'NONE', #9601, #8709, #16085, .T. ) ;
#23570 = CARTESIAN_POINT ( 'NONE',  ( 26.28373643307403640, 100.6987277884695260, -78.30371666786294327 ) ) ;
#23571 = VERTEX_POINT ( 'NONE', #15641 ) ;
#23572 = CARTESIAN_POINT ( 'NONE',  ( 28.43349137099828994, -58.58376153369790984, 109.5743306972606064 ) ) ;
#23573 = CARTESIAN_POINT ( 'NONE',  ( 1.894214914920948845, -73.39939580274850073, -125.2241265685477885 ) ) ;
#23574 = EDGE_CURVE ( 'NONE', #1087, #16492, #403, .T. ) ;
#23575 = CARTESIAN_POINT ( 'NONE',  ( 109.1592201516379674, -0.003476928926134757649, -0.007051465909552751508 ) ) ;
#23576 = CARTESIAN_POINT ( 'NONE',  ( -1.583189561560252701, 29.24830400313166123, -36.01941156322796900 ) ) ;
#23577 = CARTESIAN_POINT ( 'NONE',  ( 26.28373643307435614, 112.4918671811455511, 60.14387450369848409 ) ) ;
#23578 = DIRECTION ( 'NONE',  ( 0.5946245182733608248, -0.4045541647807529007, 0.6948076064830616128 ) ) ;
#23579 = CARTESIAN_POINT ( 'NONE',  ( 1.833691583653525026, -107.5990239011820364, -97.36155720551585091 ) ) ;
#23580 = B_SPLINE_CURVE_WITH_KNOTS ( 'NONE', 3,
 ( #21653, #2062, #8284, #8852, #10731, #1924, #23838, #10451 ),
 .UNSPECIFIED., .F., .F.,
 ( 4, 2, 2, 4 ),
 ( 0.000000000000000000, 0.002761524886576656283, 0.005523049773153312567, 0.01104609954630661126 ),
 .UNSPECIFIED. ) ;
#23581 = CONICAL_SURFACE ( 'NONE', #23563, 117.6351876552689504, 0.9945805576725580410 ) ;
#23582 = EDGE_CURVE ( 'NONE', #1068, #19971, #27221, .T. ) ;
#23583 = CARTESIAN_POINT ( 'NONE',  ( -1.045287976400365970, -43.05558670614224326, 15.59869763335140469 ) ) ;
#23585 = CARTESIAN_POINT ( 'NONE',  ( 2.063896406836605024, -31.51663808384653720, 141.8093313989359956 ) ) ;
#23584 = CARTESIAN_POINT ( 'NONE',  ( 25.64704443564077252, -97.71717520928642386, -56.57116289738710435 ) ) ;
#23586 = CARTESIAN_POINT ( 'NONE',  ( 32.73300124599740002, 62.10906484417377271, -99.90245962373766986 ) ) ;
#23587 = CIRCLE ( 'NONE', #8860, 117.6351876552689504 ) ;
#23588 = VERTEX_POINT ( 'NONE', #13499 ) ;
#23589 = ORIENTED_EDGE ( 'NONE', *, *, #10514, .T. ) ;
#23590 = CARTESIAN_POINT ( 'NONE',  ( -19.53423201713129842, 1.355459634611817431E-16, -3.388649086529543578E-17 ) ) ;
#23591 = CARTESIAN_POINT ( 'NONE',  ( 55.49584447822657296, -7.849835876627842879, -72.12568090333350312 ) ) ;
#23592 = LINE ( 'NONE', #6298, #23135 ) ;
#23593 = ADVANCED_FACE ( 'NONE', ( #9480 ), #21384, .F. ) ;
#23594 = CARTESIAN_POINT ( 'NONE',  ( 2.433796855181233454, 125.2830755159764777, -74.00833731765430912 ) ) ;
#23595 = CARTESIAN_POINT ( 'NONE',  ( -1.619063947482201282, -11.94059994246191359, -44.80407745103779860 ) ) ;
#23596 = VERTEX_POINT ( 'NONE', #22439 ) ;
#23597 = CARTESIAN_POINT ( 'NONE',  ( -25.21435515916043713, -25.00736669481004526, 23.92354251275963861 ) ) ;
#23598 = CARTESIAN_POINT ( 'NONE',  ( -1.058197053496177764, -44.07533330186778642, 12.47644286888561105 ) ) ;
#23599 = EDGE_LOOP ( 'NONE', ( #24707, #26597, #8925, #7657 ) ) ;
#23600 = CARTESIAN_POINT ( 'NONE',  ( 109.1586900883932856, -0.006561743627145281976, -0.002810909342002382467 ) ) ;
#23601 = FACE_OUTER_BOUND ( 'NONE', #18965, .T. ) ;
#23602 = CARTESIAN_POINT ( 'NONE',  ( 25.98107933586721430, 74.88680433646234746, 84.80123094405227846 ) ) ;
#23603 = CARTESIAN_POINT ( 'NONE',  ( 2.063896406836605024, -126.4736179849652871, 71.46753739785971504 ) ) ;
#23604 = CARTESIAN_POINT ( 'NONE',  ( 25.64699802086726166, 75.37548011155837457, -84.06830990999249309 ) ) ;
#23605 = ORIENTED_EDGE ( 'NONE', *, *, #20535, .F. ) ;
#23606 = CARTESIAN_POINT ( 'NONE',  ( 24.01988960052063504, 57.17607523395366798, -117.9135177031530759 ) ) ;
#23607 =( BOUNDED_SURFACE ( )  B_SPLINE_SURFACE ( 3, 1, ( 
 ( #19429, #16722 ),
 ( #25514, #21164 ),
 ( #8224, #14547 ),
 ( #23352, #19017 ) ),
 .UNSPECIFIED., .F., .F., .F. ) 
 B_SPLINE_SURFACE_WITH_KNOTS ( ( 4, 4 ),
 ( 2, 2 ),
 ( 0.000000000000000000, 1.000000000000000000 ),
 ( 0.000000000000000000, 1.000000000000000000 ),
 .UNSPECIFIED. ) 
 GEOMETRIC_REPRESENTATION_ITEM ( )  RATIONAL_B_SPLINE_SURFACE ( (
 ( 1.000000000000000000, 1.000000000000000000),
 ( 0.6386103224230316178, 0.9954351624131538845),
 ( 0.6386103224230316178, 0.9954351624131538845),
 ( 1.000000000000000000, 1.000000000000000000) ) ) 
 REPRESENTATION_ITEM ( '' )  SURFACE ( )  );
#23608 = DIRECTION ( 'NONE',  ( -0.7563875759206388771, -0.6104009704506927481, 0.2351350468682887607 ) ) ;
#23609 = CIRCLE ( 'NONE', #12089, 117.6351876552689504 ) ;
#23610 = VERTEX_POINT ( 'NONE', #2706 ) ;
#23611 = CARTESIAN_POINT ( 'NONE',  ( 109.1778270068192853, -0.008360410075196044247, 0.004106684808170100488 ) ) ;
#23612 = B_SPLINE_CURVE_WITH_KNOTS ( 'NONE', 3,
 ( #17081, #88, #8315, #8882, #6026, #23594 ),
 .UNSPECIFIED., .F., .F.,
 ( 4, 2, 4 ),
 ( 2.778605206969998010E-17, 0.0006311571484586209679, 0.001262314296917214397 ),
 .UNSPECIFIED. ) ;
#23613 = VERTEX_POINT ( 'NONE', #549 ) ;
#23614 = AXIS2_PLACEMENT_3D ( 'NONE', #12104, #10096, #18863 ) ;
#23615 = CARTESIAN_POINT ( 'NONE',  ( -20.24399999263415140, -7.930419334766389383, -28.55700515887716762 ) ) ;
#23616 = CARTESIAN_POINT ( 'NONE',  ( -18.41936578851709783, -20.09935324538221479, -37.37524689996187277 ) ) ;
#23617 = SURFACE_STYLE_USAGE ( .BOTH. , #27479 ) ;
#23618 = CARTESIAN_POINT ( 'NONE',  ( -20.20700224038492010, 18.19058640100223556, -23.35150625415664649 ) ) ;
#23619 = B_SPLINE_CURVE_WITH_KNOTS ( 'NONE', 3,
 ( #346, #13587, #2208, #26122, #9137, #26681 ),
 .UNSPECIFIED., .F., .F.,
 ( 4, 2, 4 ),
 ( 1.528920360908313465E-16, 0.003570751334075640462, 0.007141502668151127400 ),
 .UNSPECIFIED. ) ;
#23620 = CARTESIAN_POINT ( 'NONE',  ( -28.41354790283022069, 23.16239616762931064, 1.249099604787156981 ) ) ;
#23621 = CARTESIAN_POINT ( 'NONE',  ( 1.831572820252008738, 145.1082523917587253, 0.9871191512919631483 ) ) ;
#23622 = B_SPLINE_CURVE_WITH_KNOTS ( 'NONE', 3,
 ( #14501, #5743, #22883, #21112, #25311, #12069 ),
 .UNSPECIFIED., .F., .F.,
 ( 4, 2, 4 ),
 ( 3.467809420226820728E-16, 0.003576372551511154425, 0.007152745103021954098 ),
 .UNSPECIFIED. ) ;
#23623 = CARTESIAN_POINT ( 'NONE',  ( -1.323830074806765289, -28.92190886481839129, 35.86387698262947055 ) ) ;
#23624 = ADVANCED_FACE ( 'NONE', ( #26880 ), #10404, .F. ) ;
#23625 = DIRECTION ( 'NONE',  ( -0.7563875759206388771, 0.6320336713238511317, 0.1685564395263317583 ) ) ;
#23626 = CARTESIAN_POINT ( 'NONE',  ( 8.186469829614329896, -148.8557359502362942, 12.15801983495572003 ) ) ;
#23627 = ORIENTED_EDGE ( 'NONE', *, *, #25516, .T. ) ;
#23628 = ADVANCED_FACE ( 'NONE', ( #831 ), #4258, .T. ) ;
#23629 = ORIENTED_EDGE ( 'NONE', *, *, #14621, .F. ) ;
#23630 = CARTESIAN_POINT ( 'NONE',  ( 25.70243777736188306, -97.44734253939043356, -57.10783651465066413 ) ) ;
#23631 = CARTESIAN_POINT ( 'NONE',  ( -20.24399999263414784, 1.282322917263463813, -29.60996018918694617 ) ) ;
#23632 = FACE_OUTER_BOUND ( 'NONE', #178, .T. ) ;
#23633 = DIRECTION ( 'NONE',  ( 0.000000000000000000, 5.223019709707975211E-21, -1.000000000000000000 ) ) ;
#23634 = CARTESIAN_POINT ( 'NONE',  ( 28.43349137099837876, 123.0821667346709489, -17.01091693849615183 ) ) ;
#23635 = CIRCLE ( 'NONE', #2440, 117.6351876552689504 ) ;
#23636 = CARTESIAN_POINT ( 'NONE',  ( 2.430230287190581429, 133.5180086894999363, -57.85706160874013904 ) ) ;
#23637 = CARTESIAN_POINT ( 'NONE',  ( -1.048996300304493978, 26.29666317565303046, -37.49570739463894142 ) ) ;
#23638 = ORIENTED_EDGE ( 'NONE', *, *, #18153, .F. ) ;
#23639 = CARTESIAN_POINT ( 'NONE',  ( 1.833485406944043827, -144.2578170162064168, 15.69895494453337648 ) ) ;
#23640 = DIRECTION ( 'NONE',  ( -1.000000000000000000, 6.938893903907226837E-18, -1.734723475976806709E-18 ) ) ;
#23641 = CIRCLE ( 'NONE', #6156, 37.50000000000002132 ) ;
#23642 = CARTESIAN_POINT ( 'NONE',  ( 1.833838848569428359, 117.2916552720330543, -85.43736077718747879 ) ) ;
#23643 = VECTOR ( 'NONE', #11371, 1000.000000000000000 ) ;
#23644 = CARTESIAN_POINT ( 'NONE',  ( 1.832998868059890096, 14.63705790014011932, 144.3700883710217795 ) ) ;
#23645 = DIRECTION ( 'NONE',  ( 0.7563875759206388771, -0.6531865459554681008, -0.03500244528122332249 ) ) ;
#23646 = ORIENTED_EDGE ( 'NONE', *, *, #26351, .T. ) ;
#23647 = CARTESIAN_POINT ( 'NONE',  ( -8.786685647604890903, 37.00619870957935120, -38.68584556812312059 ) ) ;
#23648 = CARTESIAN_POINT ( 'NONE',  ( 25.87036335909426654, -97.41424496619563911, 57.38512068812975286 ) ) ;
#23649 = ORIENTED_EDGE ( 'NONE', *, *, #21221, .F. ) ;
#23650 = ORIENTED_EDGE ( 'NONE', *, *, #4879, .T. ) ;
#23651 = ORIENTED_EDGE ( 'NONE', *, *, #16880, .F. ) ;
#23652 =( BOUNDED_SURFACE ( )  B_SPLINE_SURFACE ( 3, 1, ( 
 ( #25571, #18650 ),
 ( #5990, #5849 ),
 ( #3111, #20655 ),
 ( #26397, #24115 ) ),
 .UNSPECIFIED., .F., .F., .F. ) 
 B_SPLINE_SURFACE_WITH_KNOTS ( ( 4, 4 ),
 ( 2, 2 ),
 ( 0.000000000000000000, 1.000000000000000000 ),
 ( 0.000000000000000000, 1.000000000000000000 ),
 .UNSPECIFIED. ) 
 GEOMETRIC_REPRESENTATION_ITEM ( )  RATIONAL_B_SPLINE_SURFACE ( (
 ( 1.000000000000000000, 1.000000000000000000),
 ( 0.9934239774497838349, 0.8357310067453913582),
 ( 0.9934239774497838349, 0.8357310067453913582),
 ( 1.000000000000000000, 1.000000000000000000) ) ) 
 REPRESENTATION_ITEM ( '' )  SURFACE ( )  );
#23653 = CARTESIAN_POINT ( 'NONE',  ( 25.70243777736189372, -107.6443926015132604, 34.20488708978063386 ) ) ;
#23654 = CARTESIAN_POINT ( 'NONE',  ( 1.831572820252009626, -132.1614873090352944, 59.92262167723391286 ) ) ;
#23655 = EDGE_CURVE ( 'NONE', #6108, #28186, #14351, .T. ) ;
#23656 = EDGE_CURVE ( 'NONE', #28480, #24250, #27749, .T. ) ;
#23657 = CARTESIAN_POINT ( 'NONE',  ( 2.263178113027036531, -133.3897502891098839, 57.85473702513823469 ) ) ;
#23658 = B_SPLINE_CURVE_WITH_KNOTS ( 'NONE', 3,
 ( #17884, #2495, #17755, #4665, #20056, #337 ),
 .UNSPECIFIED., .F., .F.,
 ( 4, 2, 4 ),
 ( 1.215080616515954935E-17, 0.0006311636237756828140, 0.001262327247551361942 ),
 .UNSPECIFIED. ) ;
#23659 = CARTESIAN_POINT ( 'NONE',  ( 13.36082413113061307, 119.8836995922726629, 94.94363694444093937 ) ) ;
#23660 = ORIENTED_EDGE ( 'NONE', *, *, #23955, .T. ) ;
#23661 = PLANE ( 'NONE',  #11044 ) ;
#23662 = EDGE_CURVE ( 'NONE', #26589, #8900, #22080, .T. ) ;
#23663 = CARTESIAN_POINT ( 'NONE',  ( -19.53423201713129842, 1.353948732986041533E-16, 28.92774122539760384 ) ) ;
#23664 = CARTESIAN_POINT ( 'NONE',  ( 1.834118845439484335, 132.6369225636073850, 58.85894970554959826 ) ) ;
#23665 = EDGE_CURVE ( 'NONE', #6278, #1423, #21739, .T. ) ;
#23666 = CARTESIAN_POINT ( 'NONE',  ( -25.21435515916043713, 15.02493970636190745, 31.17620025257570759 ) ) ;
#23667 = AXIS2_PLACEMENT_3D ( 'NONE', #4846, #9743, #18353 ) ;
#23668 = CARTESIAN_POINT ( 'NONE',  ( -55.24300891470648622, -0.0003472257464243277253, 0.009812809446890398413 ) ) ;
#23669 = CARTESIAN_POINT ( 'NONE',  ( 109.1778270068192853, -0.002542344697958529715, -0.008960903982061008133 ) ) ;
#23670 = CARTESIAN_POINT ( 'NONE',  ( -1.583189561560252701, -2.490696082059551397, 46.33203782964464068 ) ) ;
#23671 = CARTESIAN_POINT ( 'NONE',  ( -1.619063947482197729, 29.22875152547757338, -35.99532424477389725 ) ) ;
#23672 = CARTESIAN_POINT ( 'NONE',  ( 6.224689322667647851, 71.79702446228485258, -129.4863684118279821 ) ) ;
#23673 = CARTESIAN_POINT ( 'NONE',  ( 1.833809397011862519, -0.1779683723488788560, 145.1096615925545734 ) ) ;
#23674 = ORIENTED_EDGE ( 'NONE', *, *, #3907, .T. ) ;
#23675 = ORIENTED_EDGE ( 'NONE', *, *, #15865, .T. ) ;
#23676 = CARTESIAN_POINT ( 'NONE',  ( 1.833485406944057594, -108.1939177044919376, -96.69979900902278303 ) ) ;
#23677 = CARTESIAN_POINT ( 'NONE',  ( 19.66333377628721735, -38.27269871460961070, -132.3257119126252519 ) ) ;
#23678 = VERTEX_POINT ( 'NONE', #979 ) ;
#23679 = EDGE_CURVE ( 'NONE', #17615, #4550, #21058, .T. ) ;
#23680 = VERTEX_POINT ( 'NONE', #5437 ) ;
#23681 = ORIENTED_EDGE ( 'NONE', *, *, #26475, .T. ) ;
#23682 = CARTESIAN_POINT ( 'NONE',  ( -1.045287976400365970, 44.00138577190666922, 12.68782741917247670 ) ) ;
#23683 = CARTESIAN_POINT ( 'NONE',  ( 1.833485406944043827, -96.69979900902241354, 108.1939177044922786 ) ) ;
#23684 = CARTESIAN_POINT ( 'NONE',  ( 25.86096068574582674, -83.34468010038236230, -76.38617895399430324 ) ) ;
#23685 = B_SPLINE_CURVE_WITH_KNOTS ( 'NONE', 3,
 ( #21595, #8372, #10264, #15240, #1866, #17135, #12530, #6080 ),
 .UNSPECIFIED., .F., .F.,
 ( 4, 2, 2, 4 ),
 ( 2.189053321159284187E-16, 0.002761568181852863766, 0.005523136363705508090, 0.01104627272741077852 ),
 .UNSPECIFIED. ) ;
#23686 = EDGE_CURVE ( 'NONE', #16228, #27632, #15276, .T. ) ;
#23687 = CARTESIAN_POINT ( 'NONE',  ( 1.833838850855463054, -141.9572669680997592, 30.08297881069633561 ) ) ;
#23688 = CARTESIAN_POINT ( 'NONE',  ( -28.41354790283022069, 5.969609727608021998, -22.41474081378002836 ) ) ;
#23689 = ADVANCED_FACE ( 'NONE', ( #5294 ), #26331, .T. ) ;
#23690 = CARTESIAN_POINT ( 'NONE',  ( -20.20997486282892552, 0.3303599360442536770, 29.60348406988233450 ) ) ;
#23691 = LINE ( 'NONE', #28382, #10674 ) ;
#23692 = B_SPLINE_CURVE_WITH_KNOTS ( 'NONE', 3,
 ( #24460, #19836, #10795, #11344, #6334, #15640, #10928, #21725, #24043, #17255, #4726, #28459, #1995 ),
 .UNSPECIFIED., .F., .F.,
 ( 4, 3, 3, 3, 4 ),
 ( 1.250926888277100303E-17, 0.0007657099931970524301, 0.001531419946797917637, 0.002296279302920158170, 0.003061450627205759400 ),
 .UNSPECIFIED. ) ;
#23693 = CARTESIAN_POINT ( 'NONE',  ( 109.1592201516379674, 0.007620268632971107306, -0.001934867487021749589 ) ) ;
#23694 = CARTESIAN_POINT ( 'NONE',  ( 109.1721716018069515, 0.005082060336465269064, 0.01629455849719225330 ) ) ;
#23695 = CARTESIAN_POINT ( 'NONE',  ( -8.786685647604885574, 6.096987947571466530E-17, -1.524246986892866633E-17 ) ) ;
#23696 = ORIENTED_EDGE ( 'NONE', *, *, #20949, .T. ) ;
#23697 = VERTEX_POINT ( 'NONE', #8052 ) ;
#23699 = CARTESIAN_POINT ( 'NONE',  ( 109.1624594426973260, 0.01154818537150960160, 0.01102230012606007781 ) ) ;
#23698 = CARTESIAN_POINT ( 'NONE',  ( 25.64692232868534560, 112.9106972861223426, -0.3267662677155435680 ) ) ;
#23700 = CARTESIAN_POINT ( 'NONE',  ( 8.186469777910970080, 97.33125097303862105, -113.2805152945346805 ) ) ;
#23701 = CARTESIAN_POINT ( 'NONE',  ( 8.186469777910879486, -113.2805152945350073, -97.33125097303823736 ) ) ;
#23702 = CARTESIAN_POINT ( 'NONE',  ( 25.98107933586724627, 92.16448350435805992, -65.61242423298341464 ) ) ;
#23703 = ORIENTED_EDGE ( 'NONE', *, *, #24882, .F. ) ;
#23704 = CARTESIAN_POINT ( 'NONE',  ( 1.833485406944043827, -73.01664920993054864, 125.4007332306543105 ) ) ;
#23705 = CARTESIAN_POINT ( 'NONE',  ( 55.49584447822657296, 71.02133150427255259, 14.82242356767960345 ) ) ;
#23706 = CARTESIAN_POINT ( 'NONE',  ( -55.24390624410018802, -0.001811362924362171613, 0.01027195578988007209 ) ) ;
#23707 = VERTEX_POINT ( 'NONE', #16819 ) ;
#23708 = VERTEX_POINT ( 'NONE', #14199 ) ;
#23710 = CARTESIAN_POINT ( 'NONE',  ( -8.786685647604890903, -52.67761315067293282, -9.545808661480407409 ) ) ;
#23709 = B_SPLINE_CURVE_WITH_KNOTS ( 'NONE', 3,
 ( #17117, #21154, #19146, #25913, #1441, #8212, #10512 ),
 .UNSPECIFIED., .F., .F.,
 ( 4, 3, 4 ),
 ( 0.000000000000000000, 0.006568092053401790135, 0.02506242213020847681 ),
 .UNSPECIFIED. ) ;
#23711 = ORIENTED_EDGE ( 'NONE', *, *, #6651, .T. ) ;
#23712 = ORIENTED_EDGE ( 'NONE', *, *, #5648, .F. ) ;
#23713 = CARTESIAN_POINT ( 'NONE',  ( 109.1778270068192853, -0.007885345421907767605, -0.004958088776550184651 ) ) ;
#23714 = ORIENTED_EDGE ( 'NONE', *, *, #23665, .F. ) ;
#23715 = CARTESIAN_POINT ( 'NONE',  ( -1.058197053496163109, 1.754224732379551011, -45.77356582045591438 ) ) ;
#23716 = ADVANCED_FACE ( 'NONE', ( #25601 ), #28022, .F. ) ;
#23717 = ITEM_DEFINED_TRANSFORMATION ( 'NONE', 'NONE', #24522,  #27263 ) ;
#23718 = LINE ( 'NONE', #25722, #24305 ) ;
#23719 = CARTESIAN_POINT ( 'NONE',  ( 8.186469777910783563, -127.5731248346292688, 77.65916160569861404 ) ) ;
#23720 = EDGE_CURVE ( 'NONE', #9703, #12630, #13915, .T. ) ;
#23721 = CARTESIAN_POINT ( 'NONE',  ( 9.884929003653608603, 71.59798461011331483, 132.4189379373572990 ) ) ;
#23722 = B_SPLINE_CURVE_WITH_KNOTS ( 'NONE', 3,
 ( #13811, #5181, #15676, #9803, #20438, #3033, #27039 ),
 .UNSPECIFIED., .F., .F.,
 ( 4, 3, 4 ),
 ( 3.469446951953614189E-18, 0.009512539173626420944, 0.02506242213020843865 ),
 .UNSPECIFIED. ) ;
#23723 = CARTESIAN_POINT ( 'NONE',  ( 32.73300124599733607, 103.7392577722176270, 55.46353551262048853 ) ) ;
#23724 = FACE_OUTER_BOUND ( 'NONE', #13435, .T. ) ;
#23725 = CARTESIAN_POINT ( 'NONE',  ( 55.79472521941426777, 35.74479459808846826, 63.36760613016235766 ) ) ;
#23726 = EDGE_CURVE ( 'NONE', #13256, #9946, #18820, .T. ) ;
#23727 = ORIENTED_EDGE ( 'NONE', *, *, #15856, .F. ) ;
#23728 = B_SPLINE_CURVE_WITH_KNOTS ( 'NONE', 3,
 ( #3818, #18791, #20943, #12585, #1647, #19212, #27423, #27987, #17047, #25844 ),
 .UNSPECIFIED., .F., .F.,
 ( 4, 3, 3, 4 ),
 ( 1.962615573354718958E-17, 0.0002669560319015795735, 0.0005492286108966419958, 0.0008315040496093461988 ),
 .UNSPECIFIED. ) ;
#23729 = CARTESIAN_POINT ( 'NONE',  ( -55.24300891470650754, -0.007734635432136225362, 0.006048736206179294861 ) ) ;
#23731 = CARTESIAN_POINT ( 'NONE',  ( -20.57838717382308147, 1.611677988432778319, 29.92853265176829325 ) ) ;
#23730 = CARTESIAN_POINT ( 'NONE',  ( 2.430230287190589422, -144.5585181921887283, 16.65331920325691684 ) ) ;
#23732 = DIRECTION ( 'NONE',  ( -0.7563875759206388771, -0.1685564395263341175, 0.6320336713238504656 ) ) ;
#23733 = ORIENTED_EDGE ( 'NONE', *, *, #14563, .T. ) ;
#23734 = ORIENTED_EDGE ( 'NONE', *, *, #10156, .F. ) ;
#23735 = CARTESIAN_POINT ( 'NONE',  ( -8.259864102781673267, -52.60025989855198247, 6.590267880897466846 ) ) ;
#23736 = CARTESIAN_POINT ( 'NONE',  ( -1.619063947482197729, 25.20140673341430571, 38.92136151114879539 ) ) ;
#23737 = DIRECTION ( 'NONE',  ( -0.5946245182733607137, -0.6948076064830687182, 0.4045541647807407992 ) ) ;
#23738 = CARTESIAN_POINT ( 'NONE',  ( -8.786685647604885574, 6.096987947571466530E-17, -1.524246986892866633E-17 ) ) ;
#23739 = CARTESIAN_POINT ( 'NONE',  ( 10.93730112725945602, 104.7670965581007607, 108.9902118373744742 ) ) ;
#23740 = VERTEX_POINT ( 'NONE', #7763 ) ;
#23741 = CARTESIAN_POINT ( 'NONE',  ( 1.832998868059890096, 125.4013017422231115, 73.01698022778396080 ) ) ;
#23742 = ORIENTED_EDGE ( 'NONE', *, *, #1208, .T. ) ;
#23743 = CARTESIAN_POINT ( 'NONE',  ( -1.019300379054419947, 2.023851374322675589, -45.76814864815091255 ) ) ;
#23744 = CARTESIAN_POINT ( 'NONE',  ( 30.59138290137869021, 116.1811451928592334, -2.701446546448577735 ) ) ;
#23745 = CARTESIAN_POINT ( 'NONE',  ( 25.98107933586716101, -92.16448350435771886, 65.61242423298415360 ) ) ;
#23746 = B_SPLINE_CURVE_WITH_KNOTS ( 'NONE', 3,
 ( #8400, #27961, #28368, #23529 ),
 .UNSPECIFIED., .F., .F.,
 ( 4, 4 ),
 ( 3.386856006650903455E-16, 0.01077107486149799648 ),
 .UNSPECIFIED. ) ;
#23747 = CARTESIAN_POINT ( 'NONE',  ( 25.98552792386800192, -55.63155129533001997, 98.51438617140721021 ) ) ;
#23748 = ORIENTED_EDGE ( 'NONE', *, *, #21057, .F. ) ;
#23749 = CARTESIAN_POINT ( 'NONE',  ( -7.078251931573406708, -51.82710018979472721, 5.101176922831208493 ) ) ;
#23750 = CARTESIAN_POINT ( 'NONE',  ( 2.430230287190589422, -13.76600171652741800, 144.8619874886005903 ) ) ;
#23751 = VERTEX_POINT ( 'NONE', #16521 ) ;
#23752 = EDGE_CURVE ( 'NONE', #19603, #26070, #18290, .T. ) ;
#23753 = CARTESIAN_POINT ( 'NONE',  ( -1.539763995773674177, 38.84665165401067810, -25.17088606276561080 ) ) ;
#23754 = B_SPLINE_CURVE_WITH_KNOTS ( 'NONE', 3,
 ( #16339, #20652, #25136, #6267, #3815, #23408 ),
 .UNSPECIFIED., .F., .F.,
 ( 4, 2, 4 ),
 ( 4.770489558936219510E-18, 0.0006311636237756704541, 0.001262327247551336138 ),
 .UNSPECIFIED. ) ;
#23755 = CARTESIAN_POINT ( 'NONE',  ( 2.433796855181219243, -132.3327394885235435, 60.50726454507858421 ) ) ;
#23756 = ADVANCED_FACE ( 'NONE', ( #10892 ), #6517, .F. ) ;
#23757 = CARTESIAN_POINT ( 'NONE',  ( 25.64703792032473828, 103.0889146124071374, -46.06101937225500365 ) ) ;
#23758 = CARTESIAN_POINT ( 'NONE',  ( -12.94347594948482971, 47.96504705787755540, -8.691477019903484091 ) ) ;
#23759 = CARTESIAN_POINT ( 'NONE',  ( 25.98552792386799482, 55.63155129533072341, -98.51438617140682652 ) ) ;
#23760 = CARTESIAN_POINT ( 'NONE',  ( -25.21435515916025594, 1.749597353048488237E-16, -4.373993382621220594E-17 ) ) ;
#23761 = CARTESIAN_POINT ( 'NONE',  ( 109.1586900883932856, -0.002810909342011644156, -0.006561743627143320871 ) ) ;
#23762 = FACE_BOUND ( 'NONE', #3705, .T. ) ;
#23763 = CARTESIAN_POINT ( 'NONE',  ( 25.64708010899964918, 110.4552579818685274, 23.42206246795045033 ) ) ;
#23764 = CARTESIAN_POINT ( 'NONE',  ( 1.833485406944043827, -44.33323125129830089, -138.1714136985312962 ) ) ;
#23765 = CARTESIAN_POINT ( 'NONE',  ( 109.1778270068192853, -0.001591747944966589697, 0.009177562596833062358 ) ) ;
#23766 = CARTESIAN_POINT ( 'NONE',  ( 119.2224693531408803, -90.00000000000005684, -40.00000000000002842 ) ) ;
#23767 = CARTESIAN_POINT ( 'NONE',  ( 1.833485406944057594, -58.53321471326971448, 132.7804117027886548 ) ) ;
#23768 = ORIENTED_EDGE ( 'NONE', *, *, #9070, .T. ) ;
#23769 = ORIENTED_EDGE ( 'NONE', *, *, #26257, .F. ) ;
#23770 = EDGE_LOOP ( 'NONE', ( #28100, #8490, #9555, #26335 ) ) ;
#23771 = CARTESIAN_POINT ( 'NONE',  ( 30.59141879584289470, -114.2039975081482481, 21.51299111590015301 ) ) ;
#23772 = B_SPLINE_CURVE_WITH_KNOTS ( 'NONE', 3,
 ( #21495, #1909, #19478, #2047, #28379, #319, #11404, #11269, #20036, #2475, #26513, #15713, #9255 ),
 .UNSPECIFIED., .F., .F.,
 ( 4, 3, 3, 3, 4 ),
 ( 1.040834085586084257E-17, 0.0007657099931970558996, 0.001531419946797916336, 0.002296279302920154267, 0.003061450627205756364 ),
 .UNSPECIFIED. ) ;
#23773 = CARTESIAN_POINT ( 'NONE',  ( -20.24399999263414784, -28.55700515887714275, 7.930419334766489747 ) ) ;
#23774 = CARTESIAN_POINT ( 'NONE',  ( 2.430230287190589422, 144.8619874886006471, 13.76600171652692062 ) ) ;
#23775 = CARTESIAN_POINT ( 'NONE',  ( 1.833206308920068750, -141.7818018507500426, -30.89799439741769760 ) ) ;
#23776 = CARTESIAN_POINT ( 'NONE',  ( -25.21435515916025594, 1.749597353048488237E-16, -4.373993382621220594E-17 ) ) ;
#23777 = CARTESIAN_POINT ( 'NONE',  ( 25.64681081121879203, 35.28660243342691416, -107.2555980796237804 ) ) ;
#23778 = CARTESIAN_POINT ( 'NONE',  ( 109.1587776205901577, -0.002343968083389405717, 0.006944419901758085156 ) ) ;
#23779 = ORIENTED_EDGE ( 'NONE', *, *, #1109, .T. ) ;
#23780 = DIRECTION ( 'NONE',  ( 0.000000000000000000, 0.000000000000000000, 1.000000000000000000 ) ) ;
#23781 = CARTESIAN_POINT ( 'NONE',  ( -1.031422197589711764, -45.78027046666444733, -1.530725436377303073 ) ) ;
#23782 =( BOUNDED_SURFACE ( )  B_SPLINE_SURFACE ( 3, 1, ( 
 ( #25130, #13461 ),
 ( #15764, #11308 ),
 ( #11590, #2966 ),
 ( #9148, #17906 ) ),
 .UNSPECIFIED., .F., .F., .F. ) 
 B_SPLINE_SURFACE_WITH_KNOTS ( ( 4, 4 ),
 ( 2, 2 ),
 ( 0.000000000000000000, 1.000000000000000000 ),
 ( 0.000000000000000000, 1.000000000000000000 ),
 .UNSPECIFIED. ) 
 GEOMETRIC_REPRESENTATION_ITEM ( )  RATIONAL_B_SPLINE_SURFACE ( (
 ( 1.000000000000000000, 1.000000000000000000),
 ( 0.9960225298536222738, 0.9999952330161893110),
 ( 0.9960225298536222738, 0.9999952330161893110),
 ( 1.000000000000000000, 1.000000000000000000) ) ) 
 REPRESENTATION_ITEM ( '' )  SURFACE ( )  );
#23783 = CARTESIAN_POINT ( 'NONE',  ( 1.833838850855475044, 117.4485666028830053, -85.22139087168962135 ) ) ;
#23784 = DIRECTION ( 'NONE',  ( -0.7637818620346801257, 0.5092696688508612235, -0.3965875333584896190 ) ) ;
#23785 = ORIENTED_EDGE ( 'NONE', *, *, #1632, .T. ) ;
#23786 = CARTESIAN_POINT ( 'NONE',  ( 25.64704443564076541, -46.04703398841358819, 103.0951670221013217 ) ) ;
#23787 = DIRECTION ( 'NONE',  ( -0.7071067818211357325, 9.150583771627653840E-17, -0.7071067805519594129 ) ) ;
#23788 = ORIENTED_EDGE ( 'NONE', *, *, #17702, .F. ) ;
#23789 = ORIENTED_EDGE ( 'NONE', *, *, #22307, .F. ) ;
#23790 = EDGE_CURVE ( 'NONE', #25020, #16841, #10760, .T. ) ;
#23791 = B_SPLINE_CURVE_WITH_KNOTS ( 'NONE', 3,
 ( #12760, #8464, #1407, #17228 ),
 .UNSPECIFIED., .F., .F.,
 ( 4, 4 ),
 ( 0.000000000000000000, 0.008383560773332694727 ),
 .UNSPECIFIED. ) ;
#23792 = ORIENTED_EDGE ( 'NONE', *, *, #24088, .T. ) ;
#23793 = EDGE_CURVE ( 'NONE', #24227, #12813, #26206, .T. ) ;
#23794 = EDGE_CURVE ( 'NONE', #27510, #27064, #17930, .T. ) ;
#23795 = CARTESIAN_POINT ( 'NONE',  ( -55.24728320129491266, -0.01402509393918105647, -0.003868537197316873795 ) ) ;
#23796 = FACE_OUTER_BOUND ( 'NONE', #11150, .T. ) ;
#23797 = CARTESIAN_POINT ( 'NONE',  ( 2.433796855181233454, -125.2830755159759519, 74.00833731765517598 ) ) ;
#23798 = CARTESIAN_POINT ( 'NONE',  ( 9.884929003653608603, 119.2676479132373828, 91.84919534721981904 ) ) ;
#23799 = ORIENTED_EDGE ( 'NONE', *, *, #22325, .T. ) ;
#23800 = CARTESIAN_POINT ( 'NONE',  ( 109.1592201516379674, 0.004194960840980690650, -0.006649399203953405661 ) ) ;
#23801 = CARTESIAN_POINT ( 'NONE',  ( 8.186469829614358318, -97.33125097511801016, -113.2805153378648839 ) ) ;
#23802 = CARTESIAN_POINT ( 'NONE',  ( -16.86833981943423666, 43.51541671545732726, 7.884812276281646604 ) ) ;
#23803 = CARTESIAN_POINT ( 'NONE',  ( -1.031422197589716205, 37.93675465142509751, 25.67058493451402157 ) ) ;
#23804 = CARTESIAN_POINT ( 'NONE',  ( 2.430230287190592531, 46.34481016236826179, 137.9371479820464117 ) ) ;
#23805 = CARTESIAN_POINT ( 'NONE',  ( -1.323830074806776391, -44.47857376182260936, 12.01461446423248169 ) ) ;
#23806 = CARTESIAN_POINT ( 'NONE',  ( 9.884929003653626367, -114.6392083957111083, -97.56484214660738985 ) ) ;
#23807 = CARTESIAN_POINT ( 'NONE',  ( 19.66333377628702905, 137.3914191246406062, -9.924285918885045632 ) ) ;
#23808 = ORIENTED_EDGE ( 'NONE', *, *, #26929, .T. ) ;
#23809 = ADVANCED_FACE ( 'NONE', ( #8455 ), #3741, .F. ) ;
#23810 = ORIENTED_EDGE ( 'NONE', *, *, #6443, .F. ) ;
#23811 = CARTESIAN_POINT ( 'NONE',  ( -25.21435515916025594, 1.749597353048488237E-16, -4.373993382621220594E-17 ) ) ;
#23812 = DIRECTION ( 'NONE',  ( -0.000000000000000000, 1.000000000000000000, -0.000000000000000000 ) ) ;
#23813 = ORIENTED_EDGE ( 'NONE', *, *, #14620, .F. ) ;
#23814 =( BOUNDED_SURFACE ( )  B_SPLINE_SURFACE ( 3, 1, ( 
 ( #14148, #18047 ),
 ( #18630, #20781 ),
 ( #12010, #20494 ),
 ( #7140, #1073 ) ),
 .UNSPECIFIED., .F., .F., .F. ) 
 B_SPLINE_SURFACE_WITH_KNOTS ( ( 4, 4 ),
 ( 2, 2 ),
 ( 0.000000000000000000, 1.000000000000000000 ),
 ( 0.000000000000000000, 1.000000000000000000 ),
 .UNSPECIFIED. ) 
 GEOMETRIC_REPRESENTATION_ITEM ( )  RATIONAL_B_SPLINE_SURFACE ( (
 ( 1.000000000000000000, 1.000000000000000000),
 ( 0.6386103224230316178, 0.9954351624131538845),
 ( 0.6386103224230316178, 0.9954351624131538845),
 ( 1.000000000000000000, 1.000000000000000000) ) ) 
 REPRESENTATION_ITEM ( '' )  SURFACE ( )  );
#23815 = ORIENTED_EDGE ( 'NONE', *, *, #10307, .F. ) ;
#23816 = ORIENTED_EDGE ( 'NONE', *, *, #11182, .T. ) ;
#23817 = EDGE_CURVE ( 'NONE', #7509, #17315, #16215, .T. ) ;
#23818 = EDGE_CURVE ( 'NONE', #9740, #17967, #6024, .T. ) ;
#23819 = CARTESIAN_POINT ( 'NONE',  ( 13.84597867724993314, 94.55652763153807427, 112.1633818588827438 ) ) ;
#23820 = CARTESIAN_POINT ( 'NONE',  ( 1.834118845439484335, -59.18411796426966731, -132.4921483272733838 ) ) ;
#23821 = CARTESIAN_POINT ( 'NONE',  ( 14.74894986621300319, 4.490279961725991446E-15, -37.50000000000001421 ) ) ;
#23822 = CARTESIAN_POINT ( 'NONE',  ( 26.11404676487257603, -83.38016054979729574, -76.59696442953277540 ) ) ;
#23823 = CARTESIAN_POINT ( 'NONE',  ( 26.11404676487259024, 83.38016054979885894, -76.59696442953111273 ) ) ;
#23824 = CARTESIAN_POINT ( 'NONE',  ( 25.98107933586736706, 24.58827779736931163, -110.4296102877911494 ) ) ;
#23825 = CARTESIAN_POINT ( 'NONE',  ( -1.583189561560255143, 44.83405390829672399, -11.94859433442917762 ) ) ;
#23826 = CARTESIAN_POINT ( 'NONE',  ( 1.831572820252009626, -59.92262167723350785, -132.1614873090354934 ) ) ;
#23827 = DIRECTION ( 'NONE',  ( 0.7637818620346801257, -0.02150485345383945993, 0.6451161201712183324 ) ) ;
#23828 = ORIENTED_EDGE ( 'NONE', *, *, #22936, .F. ) ;
#23829 = ORIENTED_EDGE ( 'NONE', *, *, #4608, .T. ) ;
#23831 = CARTESIAN_POINT ( 'NONE',  ( -55.24271866751342941, -0.001545935011626541761, -0.009369360294294543784 ) ) ;
#23830 = CARTESIAN_POINT ( 'NONE',  ( 25.64681081121879203, 112.9102952884414464, 0.4157506337731812773 ) ) ;
#23832 = CARTESIAN_POINT ( 'NONE',  ( 25.81918753295379432, 22.58534689649824756, -110.7464580477335687 ) ) ;
#23833 = CARTESIAN_POINT ( 'NONE',  ( 25.86096068574580897, 110.3716997142158220, 24.48003142199124582 ) ) ;
#23834 = CARTESIAN_POINT ( 'NONE',  ( -55.24390624410018802, 0.001811362924362862900, -0.01027195578988028025 ) ) ;
#23835 = ORIENTED_EDGE ( 'NONE', *, *, #7103, .F. ) ;
#23836 = CARTESIAN_POINT ( 'NONE',  ( -6.574463467970643293, 11.01561683920051848, -50.12924290857540655 ) ) ;
#23837 = EDGE_CURVE ( 'NONE', #21665, #17077, #8312, .T. ) ;
#23838 = CARTESIAN_POINT ( 'NONE',  ( -2.911734481061404534, -30.23325065583388138, -36.84482841982639911 ) ) ;
#23839 = B_SPLINE_CURVE_WITH_KNOTS ( 'NONE', 3,
 ( #19200, #4642, #24237, #13269, #24679, #18014, #26375, #24532, #6529, #6965 ),
 .UNSPECIFIED., .F., .F.,
 ( 4, 3, 3, 4 ),
 ( 0.000000000000000000, 0.0002669560319015763209, 0.0005492286108966422126, 0.0008315040496093427293 ),
 .UNSPECIFIED. ) ;
#23840 = CARTESIAN_POINT ( 'NONE',  ( 26.11404676487257603, 112.4785329405483765, -12.95861723607337979 ) ) ;
#23841 = ORIENTED_EDGE ( 'NONE', *, *, #4084, .F. ) ;
#23842 = ORIENTED_EDGE ( 'NONE', *, *, #14009, .F. ) ;
#23843 = EDGE_CURVE ( 'NONE', #9585, #18375, #10609, .T. ) ;
#23844 = CARTESIAN_POINT ( 'NONE',  ( 32.73300124599735739, 3.836798148478847370, 117.5726003567930178 ) ) ;
#23845 = ORIENTED_EDGE ( 'NONE', *, *, #12234, .T. ) ;
#23846 = CARTESIAN_POINT ( 'NONE',  ( -20.20700224038492010, -10.08426345511570332, 27.82980252387829623 ) ) ;
#23847 =( BOUNDED_SURFACE ( )  B_SPLINE_SURFACE ( 3, 1, ( 
 ( #9551, #5228 ),
 ( #16019, #3213 ),
 ( #14281, #18172 ),
 ( #18309, #20768 ) ),
 .UNSPECIFIED., .F., .F., .F. ) 
 B_SPLINE_SURFACE_WITH_KNOTS ( ( 4, 4 ),
 ( 2, 2 ),
 ( 0.000000000000000000, 1.000000000000000000 ),
 ( 0.000000000000000000, 1.000000000000000000 ),
 .UNSPECIFIED. ) 
 GEOMETRIC_REPRESENTATION_ITEM ( )  RATIONAL_B_SPLINE_SURFACE ( (
 ( 1.000000000000000000, 1.000000000000000000),
 ( 0.6386103224230316178, 0.9954351624131538845),
 ( 0.6386103224230316178, 0.9954351624131538845),
 ( 1.000000000000000000, 1.000000000000000000) ) ) 
 REPRESENTATION_ITEM ( '' )  SURFACE ( )  );
#23848 = ORIENTED_EDGE ( 'NONE', *, *, #10741, .F. ) ;
#23849 = EDGE_CURVE ( 'NONE', #12008, #1309, #4235, .T. ) ;
#23850 = VECTOR ( 'NONE', #11228, 1000.000000000000114 ) ;
#23851 = DIRECTION ( 'NONE',  ( 0.5946245182733608248, 0.4749651461092296856, -0.6487139525627699799 ) ) ;
#23852 = EDGE_CURVE ( 'NONE', #5490, #16899, #13014, .T. ) ;
#23853 = ORIENTED_EDGE ( 'NONE', *, *, #3071, .T. ) ;
#23854 = CARTESIAN_POINT ( 'NONE',  ( 109.1592201516379674, -0.001331853079208366458, -0.007748443302128551168 ) ) ;
#23855 = CARTESIAN_POINT ( 'NONE',  ( -24.53239521893651442, -14.09666242510773948, 30.86654523348680002 ) ) ;
#23856 = CARTESIAN_POINT ( 'NONE',  ( -1.113427685307002424, -38.22586258295212502, -25.34053733836516642 ) ) ;
#23857 = CARTESIAN_POINT ( 'NONE',  ( -55.24198130335446422, 0.004163123460806185221, -0.008310594958150844397 ) ) ;
#23858 = B_SPLINE_CURVE_WITH_KNOTS ( 'NONE', 3,
 ( #4250, #26131, #11024, #10599, #10466, #25996, #8445, #6288, #15038, #23860, #4109, #17342, #2960 ),
 .UNSPECIFIED., .F., .F.,
 ( 4, 3, 3, 3, 4 ),
 ( 8.673617379884035472E-18, 0.0007657099931970526470, 0.001531419946797914385, 0.002296279302920149496, 0.003061450627205760701 ),
 .UNSPECIFIED. ) ;
#23859 = FACE_OUTER_BOUND ( 'NONE', #25035, .T. ) ;
#23860 = CARTESIAN_POINT ( 'NONE',  ( -1.048994561756806831, 14.87838255483256233, -43.31369460697981566 ) ) ;
#23861 = DIRECTION ( 'NONE',  ( 0.5914120900931444380, -0.3962188444547240507, -0.7023121577978139740 ) ) ;
#23862 = CARTESIAN_POINT ( 'NONE',  ( -1.019300379054419725, 12.21833869579464604, -44.15350047934403221 ) ) ;
#23864 = CARTESIAN_POINT ( 'NONE',  ( -1.323439229708139875, 46.01398008004444762, -2.317790194799894010 ) ) ;
#23863 = CARTESIAN_POINT ( 'NONE',  ( 1.833485406944057594, 0.5339064996884692604, 145.1085452359073429 ) ) ;
#23865 = CARTESIAN_POINT ( 'NONE',  ( 10.93730112726003156, 97.44200844886434254, -115.5857507957695276 ) ) ;
#23866 = ORIENTED_EDGE ( 'NONE', *, *, #16505, .F. ) ;
#23867 = ORIENTED_EDGE ( 'NONE', *, *, #5562, .F. ) ;
#23868 = DIRECTION ( 'NONE',  ( -1.000000000000000000, -0.000000000000000000, -0.000000000000000000 ) ) ;
#23869 = DIRECTION ( 'NONE',  ( 0.5946245182733607137, 0.7356888587241657840, -0.3243201896541563212 ) ) ;
#23871 = CARTESIAN_POINT ( 'NONE',  ( 25.64681081121879203, -97.99105938547964456, 56.09509703373309719 ) ) ;
#23870 = CARTESIAN_POINT ( 'NONE',  ( -12.94347594948482438, 42.93165645342861581, -23.08810053288705078 ) ) ;
#23872 = CARTESIAN_POINT ( 'NONE',  ( 1.833485406944043827, -144.2578170162064168, 15.69895494453337648 ) ) ;
#23873 = CARTESIAN_POINT ( 'NONE',  ( 2.263178113027037419, 84.32376073259221982, 118.4461880110606131 ) ) ;
#23874 = CARTESIAN_POINT ( 'NONE',  ( -20.57838717382308147, -25.16001208503093522, 16.28767523336148315 ) ) ;
#23875 = VECTOR ( 'NONE', #7256, 1000.000000000000114 ) ;
#23876 = ORIENTED_EDGE ( 'NONE', *, *, #22939, .F. ) ;
#23877 = CARTESIAN_POINT ( 'NONE',  ( -1.031422197589711764, -37.93675465142452907, 25.67058493451483514 ) ) ;
#23878 = CARTESIAN_POINT ( 'NONE',  ( -55.25719721206881729, 0.002847566758684554142, 0.01079965405819473083 ) ) ;
#23879 = CARTESIAN_POINT ( 'NONE',  ( 2.108393763691186695, -46.11438684123258724, 137.7805780486504545 ) ) ;
#23880 = EDGE_CURVE ( 'NONE', #5961, #11177, #6652, .T. ) ;
#23881 = ORIENTED_EDGE ( 'NONE', *, *, #28105, .F. ) ;
#23882 = FACE_OUTER_BOUND ( 'NONE', #8357, .T. ) ;
#23883 = EDGE_CURVE ( 'NONE', #18593, #7658, #13455, .T. ) ;
#23884 = CARTESIAN_POINT ( 'NONE',  ( 1.832998868059858122, -14.63705790014105546, 144.3700883710216658 ) ) ;
#23885 = EDGE_CURVE ( 'NONE', #17556, #13659, #6256, .T. ) ;
#23886 = ORIENTED_EDGE ( 'NONE', *, *, #28380, .F. ) ;
#23887 = CARTESIAN_POINT ( 'NONE',  ( 2.108393763691158274, 116.7869873529609919, 86.43392821214625599 ) ) ;
#23888 = FACE_OUTER_BOUND ( 'NONE', #10757, .T. ) ;
#23889 = CARTESIAN_POINT ( 'NONE',  ( 0.000000000000000000, 0.000000000000000000, 0.000000000000000000 ) ) ;
#23890 = CARTESIAN_POINT ( 'NONE',  ( 25.64708010899963497, 97.81137751680995507, 56.40825696968293812 ) ) ;
#23891 = CARTESIAN_POINT ( 'NONE',  ( -1.050231094221214079, 37.20185272688497236, 26.71409683968576942 ) ) ;
#23892 = CARTESIAN_POINT ( 'NONE',  ( 25.64660436782556729, 55.95243482911524069, -98.07256794792259313 ) ) ;
#23893 = CARTESIAN_POINT ( 'NONE',  ( -1.259972190295316485, -45.95417440459613090, 2.243354636026243742 ) ) ;
#23894 = CARTESIAN_POINT ( 'NONE',  ( -55.24340739397742794, 0.009386184976285603249, -0.003826481709800144074 ) ) ;
#23895 = CARTESIAN_POINT ( 'NONE',  ( 16.75465622695655910, -102.5353941815396439, -98.56308464785165313 ) ) ;
#23896 = CARTESIAN_POINT ( 'NONE',  ( 32.73300124599732186, 0.000000000000000000, 0.000000000000000000 ) ) ;
#23897 = CARTESIAN_POINT ( 'NONE',  ( 2.430230287190581429, 132.3371620660951180, 60.50928654924798167 ) ) ;
#23898 = CARTESIAN_POINT ( 'NONE',  ( 6.224689322667630975, -2.565137105444788901, 148.0369967195762797 ) ) ;
#23899 = CARTESIAN_POINT ( 'NONE',  ( -25.21435515916043713, 34.05351380035342146, 6.169479169075106739 ) ) ;
#23900 = EDGE_LOOP ( 'NONE', ( #14662, #19777, #25445, #19029 ) ) ;
#23901 = VERTEX_POINT ( 'NONE', #15008 ) ;
#23902 = ORIENTED_EDGE ( 'NONE', *, *, #9204, .T. ) ;
#23903 = CARTESIAN_POINT ( 'NONE',  ( 25.64704443564077607, 103.0951670221014496, 46.04703398841322581 ) ) ;
#23904 = LINE ( 'NONE', #6207, #3345 ) ;
#23905 = CARTESIAN_POINT ( 'NONE',  ( -6.574463467970653952, 38.37705091668375701, -34.08059230520056104 ) ) ;
#23906 = CARTESIAN_POINT ( 'NONE',  ( -12.94347594948487057, -47.96504705787739198, 8.691477019903814494 ) ) ;
#23907 = CARTESIAN_POINT ( 'NONE',  ( -1.031422197589711764, -25.67058493451469303, -37.93675465142463565 ) ) ;
#23908 = CARTESIAN_POINT ( 'NONE',  ( 10.93730112726002979, 79.81734490846109509, -128.3908183996583432 ) ) ;
#23909 = CARTESIAN_POINT ( 'NONE',  ( -1.050231094221210082, 26.71409683968617799, -37.20185272688468814 ) ) ;
#23910 = ORIENTED_EDGE ( 'NONE', *, *, #11989, .F. ) ;
#23911 = CARTESIAN_POINT ( 'NONE',  ( 26.11404676487259024, 36.06104232266452669, 107.3263591096431639 ) ) ;
#23912 = CARTESIAN_POINT ( 'NONE',  ( -55.24300891470648622, 0.008142823778062486390, -0.005486913146696510354 ) ) ;
#23913 = CARTESIAN_POINT ( 'NONE',  ( 109.1587776205901861, -0.002343968083398788402, -0.006944419901758122453 ) ) ;
#23914 = EDGE_CURVE ( 'NONE', #5234, #14104, #25152, .T. ) ;
#23915 = CARTESIAN_POINT ( 'NONE',  ( 1.833485406944043827, -73.01664920992880070, -125.4007332306553195 ) ) ;
#23916 = ORIENTED_EDGE ( 'NONE', *, *, #6903, .F. ) ;
#23917 = CARTESIAN_POINT ( 'NONE',  ( 25.64681081121879203, -112.2483031020012589, -12.21581276189922427 ) ) ;
#23918 = EDGE_CURVE ( 'NONE', #4343, #10772, #6821, .T. ) ;
#23919 = DIRECTION ( 'NONE',  ( -1.000000000000000000, -0.000000000000000000, -0.000000000000000000 ) ) ;
#23920 = ORIENTED_EDGE ( 'NONE', *, *, #11695, .T. ) ;
#23921 = EDGE_CURVE ( 'NONE', #22316, #14882, #15566, .T. ) ;
#23922 = ORIENTED_EDGE ( 'NONE', *, *, #24154, .F. ) ;
#23923 = ORIENTED_EDGE ( 'NONE', *, *, #17543, .F. ) ;
#23924 = CARTESIAN_POINT ( 'NONE',  ( 109.1592201516379674, -0.007566779963318568183, 0.002134489919774338555 ) ) ;
#23925 = CARTESIAN_POINT ( 'NONE',  ( -1.031422197589711764, -36.13727897780146492, -28.14735071801730726 ) ) ;
#23926 = LINE ( 'NONE', #4460, #14296 ) ;
#23927 = VECTOR ( 'NONE', #1566, 1000.000000000000000 ) ;
#23928 = CARTESIAN_POINT ( 'NONE',  ( 24.01988960052031530, 111.2910478358005122, 69.18817751538362870 ) ) ;
#23929 = ORIENTED_EDGE ( 'NONE', *, *, #19741, .T. ) ;
#23930 = CARTESIAN_POINT ( 'NONE',  ( 1.833603222531983379, 59.42758433816144503, -132.3826570575577364 ) ) ;
#23931 = B_SPLINE_CURVE_WITH_KNOTS ( 'NONE', 3,
 ( #20221, #17784, #17912, #26703, #7293, #26849, #24430 ),
 .UNSPECIFIED., .F., .F.,
 ( 4, 3, 4 ),
 ( 5.319721237705389368E-16, 0.02816610861753246486, 0.04000277880656274293 ),
 .UNSPECIFIED. ) ;
#23932 = CARTESIAN_POINT ( 'NONE',  ( -25.21435515916025594, 1.749597353048488237E-16, -4.373993382621220594E-17 ) ) ;
#23933 = CARTESIAN_POINT ( 'NONE',  ( 109.1587776205901577, 0.006661366261224497057, 0.003057017121591230555 ) ) ;
#23934 = EDGE_CURVE ( 'NONE', #1461, #2416, #8334, .T. ) ;
#23935 = FACE_OUTER_BOUND ( 'NONE', #25374, .T. ) ;
#23936 = CARTESIAN_POINT ( 'NONE',  ( 99.22246935314079508, 70.00000000000004263, 39.99999999999999289 ) ) ;
#23937 = ADVANCED_FACE ( 'NONE', ( #21791 ), #26016, .F. ) ;
#23938 = CARTESIAN_POINT ( 'NONE',  ( 109.1586059443104944, -0.004524147648833204242, -0.005438258427225600017 ) ) ;
#23939 = DIRECTION ( 'NONE',  ( -0.5914120900931443270, -0.1598001217819418063, 0.7903769105750340085 ) ) ;
#23940 = EDGE_CURVE ( 'NONE', #13567, #17941, #21555, .T. ) ;
#23941 = CARTESIAN_POINT ( 'NONE',  ( 6.224689322667630975, 121.2721959030549499, -84.93872395422852151 ) ) ;
#23942 = ORIENTED_EDGE ( 'NONE', *, *, #2568, .F. ) ;
#23943 = ORIENTED_EDGE ( 'NONE', *, *, #27194, .T. ) ;
#23944 = CARTESIAN_POINT ( 'NONE',  ( 109.1586059443104944, 0.006808232911144239917, -0.001921075557427576489 ) ) ;
#23945 = VECTOR ( 'NONE', #28057, 999.9999999999998863 ) ;
#23946 = CARTESIAN_POINT ( 'NONE',  ( -21.41427618760458884, -28.68857606049974862, -11.22988868156173581 ) ) ;
#23947 = ORIENTED_EDGE ( 'NONE', *, *, #22339, .T. ) ;
#23948 = ORIENTED_EDGE ( 'NONE', *, *, #21482, .F. ) ;
#23949 = EDGE_LOOP ( 'NONE', ( #6451, #10556, #13598, #15180 ) ) ;
#23950 = VECTOR ( 'NONE', #21981, 999.9999999999998863 ) ;
#23951 = FACE_OUTER_BOUND ( 'NONE', #18120, .T. ) ;
#23952 = B_SPLINE_CURVE_WITH_KNOTS ( 'NONE', 3,
 ( #18340, #7431, #25005, #5257, #20650, #1643, #28119 ),
 .UNSPECIFIED., .F., .F.,
 ( 4, 3, 4 ),
 ( 5.463690523629807176E-17, 0.009512539173626407066, 0.02506242213020838661 ),
 .UNSPECIFIED. ) ;
#23953 = CARTESIAN_POINT ( 'NONE',  ( 1.834118845439484335, 44.67218053242574882, -138.0627591860425412 ) ) ;
#23954 = CARTESIAN_POINT ( 'NONE',  ( -20.20700224038492721, 28.44216453106548315, 8.199606986804035103 ) ) ;
#23955 = EDGE_CURVE ( 'NONE', #8031, #18704, #9218, .T. ) ;
#23956 = CARTESIAN_POINT ( 'NONE',  ( 30.59138290137916627, 75.73279410806848944, -88.14703743378181855 ) ) ;
#23957 = AXIS2_PLACEMENT_3D ( 'NONE', #2789, #635, #7130 ) ;
#23958 = B_SPLINE_CURVE_WITH_KNOTS ( 'NONE', 3,
 ( #4241, #15748, #2070, #4822, #11015, #17621 ),
 .UNSPECIFIED., .F., .F.,
 ( 4, 2, 4 ),
 ( 6.938893903907228378E-18, 0.0006311636237756803203, 0.001262327247551353702 ),
 .UNSPECIFIED. ) ;
#23959 = CARTESIAN_POINT ( 'NONE',  ( -25.21435515916025594, 34.29329011225976132, 4.655591116594488099 ) ) ;
#23960 = CIRCLE ( 'NONE', #24893, 151.1787379149930359 ) ;
#23961 = CARTESIAN_POINT ( 'NONE',  ( -1.619063947482194177, 35.99532424477422410, 29.22875152547716482 ) ) ;
#23962 = B_SPLINE_CURVE_WITH_KNOTS ( 'NONE', 3,
 ( #20556, #23178, #16237, #5299, #18687, #27459, #23024 ),
 .UNSPECIFIED., .F., .F.,
 ( 4, 3, 4 ),
 ( 5.669813051359019560E-16, 0.02816610861753245793, 0.04000277880656276375 ),
 .UNSPECIFIED. ) ;
#23963 = ADVANCED_FACE ( 'NONE', ( #22803 ), #15133, .F. ) ;
#23964 = CARTESIAN_POINT ( 'NONE',  ( 109.1586900883932856, 0.004701023939953857290, 0.005371970278523981006 ) ) ;
#23965 = CARTESIAN_POINT ( 'NONE',  ( -1.048996300304505747, 27.53442103413745912, 36.59642367107714023 ) ) ;
#23966 = VECTOR ( 'NONE', #9051, 1000.000000000000114 ) ;
#23967 = ADVANCED_FACE ( 'NONE', ( #897 ), #24339, .F. ) ;
#23968 = ORIENTED_EDGE ( 'NONE', *, *, #6868, .F. ) ;
#23969 = ORIENTED_EDGE ( 'NONE', *, *, #626, .F. ) ;
#23970 = CARTESIAN_POINT ( 'NONE',  ( -18.41936578851709783, -29.33493038358050242, 30.66520733838684265 ) ) ;
#23971 = CARTESIAN_POINT ( 'NONE',  ( 25.98552792386802324, 22.46612985365126036, -110.8838436908324212 ) ) ;
#23972 = CARTESIAN_POINT ( 'NONE',  ( -2.904412668506660467, 11.97478724945576545, 46.12477647685262383 ) ) ;
#23973 = DIRECTION ( 'NONE',  ( 0.000000000000000000, 0.000000000000000000, 1.000000000000000000 ) ) ;
#23974 = CARTESIAN_POINT ( 'NONE',  ( 2.063896406836609909, -71.46753739786105086, 126.4736179849645481 ) ) ;
#23975 =( BOUNDED_SURFACE ( )  B_SPLINE_SURFACE ( 3, 1, ( 
 ( #18424, #18721 ),
 ( #27049, #23062 ),
 ( #3464, #22779 ),
 ( #23208, #22630 ) ),
 .UNSPECIFIED., .F., .F., .F. ) 
 B_SPLINE_SURFACE_WITH_KNOTS ( ( 4, 4 ),
 ( 2, 2 ),
 ( 0.000000000000000000, 1.000000000000000000 ),
 ( 0.000000000000000000, 1.000000000000000000 ),
 .UNSPECIFIED. ) 
 GEOMETRIC_REPRESENTATION_ITEM ( )  RATIONAL_B_SPLINE_SURFACE ( (
 ( 1.000000000000000000, 1.000000000000000000),
 ( 0.9956975270656955868, 0.8568959468854907557),
 ( 0.9956975270656955868, 0.8568959468854907557),
 ( 1.000000000000000000, 1.000000000000000000) ) ) 
 REPRESENTATION_ITEM ( '' )  SURFACE ( )  );
#23976 = ORIENTED_EDGE ( 'NONE', *, *, #9136, .T. ) ;
#23977 = CARTESIAN_POINT ( 'NONE',  ( -8.259864102781671491, 9.986657004933631399, -52.06232470801713674 ) ) ;
#23978 = CARTESIAN_POINT ( 'NONE',  ( 2.108393763691197353, 118.2927144690670787, -84.36147263237450034 ) ) ;
#23979 = CARTESIAN_POINT ( 'NONE',  ( -1.048171036023496594, -36.44209502233728415, -27.73816396939552931 ) ) ;
#23980 = ORIENTED_EDGE ( 'NONE', *, *, #27151, .F. ) ;
#23981 = ORIENTED_EDGE ( 'NONE', *, *, #21482, .T. ) ;
#23982 = CARTESIAN_POINT ( 'NONE',  ( -1.113548883309551929, -16.03115934825500588, 42.96943836789122173 ) ) ;
#23983 = EDGE_LOOP ( 'NONE', ( #2064, #2947, #11061, #27808 ) ) ;
#23984 = CARTESIAN_POINT ( 'NONE',  ( -28.13707043255157103, 14.07296284901332761, -18.06394523322457957 ) ) ;
#23985 = VERTEX_POINT ( 'NONE', #20180 ) ;
#23986 = CONICAL_SURFACE ( 'NONE', #17520, 28.92774122539760384, 0.7853981625000054922 ) ;
#23987 = VECTOR ( 'NONE', #19964, 1000.000000000000114 ) ;
#23988 = CARTESIAN_POINT ( 'NONE',  ( 2.063896406836605024, -138.5688025270881383, 43.61045647697645933 ) ) ;
#23989 = AXIS2_PLACEMENT_3D ( 'NONE', #14749, #14608, #3527 ) ;
#23990 = ORIENTED_EDGE ( 'NONE', *, *, #1051, .F. ) ;
#23991 = CARTESIAN_POINT ( 'NONE',  ( 2.263178113027032978, 126.6115605262348112, -71.48082833564930638 ) ) ;
#23992 = EDGE_CURVE ( 'NONE', #1180, #24611, #8515, .T. ) ;
#23993 = CARTESIAN_POINT ( 'NONE',  ( 1.832998868059858122, -117.0819875546701070, 85.72499093308064744 ) ) ;
#23994 = CARTESIAN_POINT ( 'NONE',  ( 25.98107933586730667, -112.3948402207511208, -12.91054317625230397 ) ) ;
#23995 = ADVANCED_FACE ( 'NONE', ( #20613 ), #4652, .F. ) ;
#23996 = ORIENTED_EDGE ( 'NONE', *, *, #1496, .T. ) ;
#23997 = CARTESIAN_POINT ( 'NONE',  ( 25.81918753295378721, -103.6306245682012701, -45.11728622333246363 ) ) ;
#23999 = CARTESIAN_POINT ( 'NONE',  ( 25.98552792386796995, -10.75254026142880548, 112.6247604222998433 ) ) ;
#23998 = CARTESIAN_POINT ( 'NONE',  ( 1.833721036429677875, 0.3559391723980712685, 145.1093571290645627 ) ) ;
#24000 = CARTESIAN_POINT ( 'NONE',  ( -1.539760825549688628, -2.469813586483410539, -46.22267384399379608 ) ) ;
#24001 = EDGE_CURVE ( 'NONE', #11755, #27686, #16410, .T. ) ;
#24002 = ORIENTED_EDGE ( 'NONE', *, *, #11273, .F. ) ;
#24003 = ORIENTED_EDGE ( 'NONE', *, *, #11580, .T. ) ;
#24004 = CARTESIAN_POINT ( 'NONE',  ( 8.186469777910868828, -140.9315935720373147, 49.43817851234016558 ) ) ;
#24005 = CARTESIAN_POINT ( 'NONE',  ( -1.323830074806759960, 25.17121255494532406, 38.58891736138504314 ) ) ;
#24007 = CARTESIAN_POINT ( 'NONE',  ( 25.65782528836481191, -98.07785559018917354, 55.95807498711450023 ) ) ;
#24006 = CARTESIAN_POINT ( 'NONE',  ( -25.21435515916043002, 30.48034229288640162, -16.39063784838753790 ) ) ;
#24008 = CARTESIAN_POINT ( 'NONE',  ( -18.41936578851713335, 20.09935324538248480, 37.37524689996173777 ) ) ;
#24009 = CARTESIAN_POINT ( 'NONE',  ( 10.93730112725932813, 150.7858122213658305, 10.89264110825069132 ) ) ;
#24010 = CARTESIAN_POINT ( 'NONE',  ( 25.64681081121879203, 91.10197563708035773, -66.70335573067774249 ) ) ;
#24011 = EDGE_CURVE ( 'NONE', #21239, #26564, #11259, .T. ) ;
#24012 = EDGE_LOOP ( 'NONE', ( #18697, #3120, #23526, #7151 ) ) ;
#24013 = CARTESIAN_POINT ( 'NONE',  ( 25.64707127832796019, 6.059145946834079367E-17, -112.9112343549835487 ) ) ;
#24014 = VECTOR ( 'NONE', #22138, 1000.000000000000341 ) ;
#24015 = CARTESIAN_POINT ( 'NONE',  ( 2.063896406836609909, 138.5688025270878541, 43.61045647697738303 ) ) ;
#24016 = CARTESIAN_POINT ( 'NONE',  ( 25.64670758986457599, -91.63870681572869614, 65.96397693491134362 ) ) ;
#24017 = CARTESIAN_POINT ( 'NONE',  ( -8.786685647604720373, -47.14957014837338534, -25.35688121747513435 ) ) ;
#24018 = ORIENTED_EDGE ( 'NONE', *, *, #18823, .T. ) ;
#24019 = DIRECTION ( 'NONE',  ( -0.5946245182733607137, -0.1642747008466245162, 0.7870422510449649467 ) ) ;
#24020 = CARTESIAN_POINT ( 'NONE',  ( 9.884929003653626367, -71.59798461011423854, 132.4189379373568443 ) ) ;
#24021 = CARTESIAN_POINT ( 'NONE',  ( -1.539763995773691940, 46.22267697748604576, 2.469814354917652999 ) ) ;
#24022 = VERTEX_POINT ( 'NONE', #1022 ) ;
#24023 = DIRECTION ( 'NONE',  ( -1.000000000000000000, -0.000000000000000000, -0.000000000000000000 ) ) ;
#24024 = B_SPLINE_CURVE_WITH_KNOTS ( 'NONE', 3,
 ( #16625, #16328, #7719, #27408, #3379, #3236, #25416, #5691, #23118, #14453 ),
 .UNSPECIFIED., .F., .F.,
 ( 4, 2, 2, 2, 4 ),
 ( 2.976962515321448001E-16, 0.0003346187017559152190, 0.0006692374035115327162, 0.001003856105267150267, 0.001338474807022767710 ),
 .UNSPECIFIED. ) ;
#24025 = CARTESIAN_POINT ( 'NONE',  ( 5.340103579038038895, 146.8647350263016165, 13.12023871299778932 ) ) ;
#24026 = CARTESIAN_POINT ( 'NONE',  ( 1.833206310202337486, -71.90885922990241852, 126.0392056382539892 ) ) ;
#24027 = VECTOR ( 'NONE', #6827, 1000.000000000000341 ) ;
#24028 = DIRECTION ( 'NONE',  ( 0.000000000000000000, 0.000000000000000000, 1.000000000000000000 ) ) ;
#24029 = FACE_OUTER_BOUND ( 'NONE', #1066, .T. ) ;
#24030 = VECTOR ( 'NONE', #12005, 1000.000000000000000 ) ;
#24031 = CARTESIAN_POINT ( 'NONE',  ( 2.433796855181219243, 132.3327394885239698, -60.50726454507772445 ) ) ;
#24032 = CARTESIAN_POINT ( 'NONE',  ( 55.49584447822657296, -58.53775398922284978, 42.86099773636522059 ) ) ;
#24033 = CARTESIAN_POINT ( 'NONE',  ( 30.59141879584282719, 21.51299111590054380, 114.2039975081481344 ) ) ;
#24034 = EDGE_CURVE ( 'NONE', #12261, #8723, #1319, .T. ) ;
#24035 = CARTESIAN_POINT ( 'NONE',  ( -12.82751273423880178, -23.15139349681279057, 43.04932478553559605 ) ) ;
#24036 = DIRECTION ( 'NONE',  ( 0.000000000000000000, 0.000000000000000000, 1.000000000000000000 ) ) ;
#24037 = CARTESIAN_POINT ( 'NONE',  ( -28.13707043255157103, -21.52861750560944998, -7.802116958608919184 ) ) ;
#24038 = CARTESIAN_POINT ( 'NONE',  ( 25.64681081121879203, 45.54494737132223747, 103.3177883989780952 ) ) ;
#24039 = ORIENTED_EDGE ( 'NONE', *, *, #13405, .T. ) ;
#24040 = ADVANCED_FACE ( 'NONE', ( #20884 ), #11822, .F. ) ;
#24041 = ORIENTED_EDGE ( 'NONE', *, *, #12230, .F. ) ;
#24042 = EDGE_LOOP ( 'NONE', ( #1625, #14535, #12831, #20859 ) ) ;
#24043 = CARTESIAN_POINT ( 'NONE',  ( -1.049817751779876129, -43.71287583013717182, 13.66628317065032583 ) ) ;
#24044 = CARTESIAN_POINT ( 'NONE',  ( -16.86833981943427574, 39.83928801320588775, -19.19877306373863490 ) ) ;
#24045 = CARTESIAN_POINT ( 'NONE',  ( -4.780792508754314163, -32.07473752860752825, 37.74278713234433269 ) ) ;
#24046 = DIRECTION ( 'NONE',  ( 0.000000000000000000, -0.000000000000000000, -1.000000000000000000 ) ) ;
#24047 = CARTESIAN_POINT ( 'NONE',  ( 8.186469829614525295, 131.0413692472670277, -71.65198613712843212 ) ) ;
#24048 = CARTESIAN_POINT ( 'NONE',  ( 30.59138290137909877, -14.83088430729485552, -115.2623146671593020 ) ) ;
#24049 = CARTESIAN_POINT ( 'NONE',  ( -1.046935749539993799, 27.93995161054695231, -36.28605774377773230 ) ) ;
#24050 = VERTEX_POINT ( 'NONE', #20590 ) ;
#24051 = CARTESIAN_POINT ( 'NONE',  ( 26.11404676487257603, 112.4785329405482059, 12.95861723607491456 ) ) ;
#24052 = CARTESIAN_POINT ( 'NONE',  ( -55.24390624410018802, 0.007245494385991918876, 0.007503127514281743120 ) ) ;
#24053 = DIRECTION ( 'NONE',  ( -0.7637818620346801257, 0.6451161201712179993, -0.02150485345385064542 ) ) ;
#24054 = CARTESIAN_POINT ( 'NONE',  ( 109.1587776205901861, -0.001442274044995847443, 0.007186028091168150840 ) ) ;
#24055 = CIRCLE ( 'NONE', #14843, 34.60786435723138510 ) ;
#24056 = CARTESIAN_POINT ( 'NONE',  ( 109.1592201516379674, -0.0003082430542016361633, -0.007856029051022768092 ) ) ;
#24057 = CONICAL_SURFACE ( 'NONE', #19432, 34.60786435723138510, 0.8559913436420825139 ) ;
#24058 = AXIS2_PLACEMENT_3D ( 'NONE', #13152, #15023, #8285 ) ;
#24059 = CARTESIAN_POINT ( 'NONE',  ( 1.833603222531957844, -108.1346772638452904, 96.76619886578292551 ) ) ;
#24060 = CARTESIAN_POINT ( 'NONE',  ( 25.64692232868533139, -56.73833653200176030, -97.62014907493936278 ) ) ;
#24061 = ORIENTED_EDGE ( 'NONE', *, *, #16432, .F. ) ;
#24062 = VERTEX_POINT ( 'NONE', #12248 ) ;
#24063 = EDGE_LOOP ( 'NONE', ( #1221, #14913, #13895, #15386 ) ) ;
#24064 = CARTESIAN_POINT ( 'NONE',  ( -25.21435515916042647, 15.02493970636146692, -31.17620025257592786 ) ) ;
#24065 = FACE_OUTER_BOUND ( 'NONE', #10298, .T. ) ;
#24066 = CARTESIAN_POINT ( 'NONE',  ( 9.884929003653608603, 141.8132360130357768, 50.49804566712172260 ) ) ;
#24067 = EDGE_CURVE ( 'NONE', #26154, #21665, #9962, .T. ) ;
#24068 = ORIENTED_EDGE ( 'NONE', *, *, #25078, .T. ) ;
#24069 = CARTESIAN_POINT ( 'NONE',  ( -4.162674018437135359, 31.44946543094296487, -37.46098494546600932 ) ) ;
#24070 = EDGE_CURVE ( 'NONE', #7819, #1487, #9659, .T. ) ;
#24071 = VECTOR ( 'NONE', #26183, 1000.000000000000114 ) ;
#24072 = CARTESIAN_POINT ( 'NONE',  ( 2.108393763691171596, -142.3786741588522773, 28.95405853987470479 ) ) ;
#24073 = EDGE_CURVE ( 'NONE', #17580, #27461, #9892, .T. ) ;
#24074 = FACE_OUTER_BOUND ( 'NONE', #25957, .T. ) ;
#24075 = ADVANCED_FACE ( 'NONE', ( #7956 ), #7631, .F. ) ;
#24076 = ADVANCED_BREP_SHAPE_REPRESENTATION ( '', ( #7750, #27263 ), #6137 ) ;
#24077 = DIRECTION ( 'NONE',  ( 0.000000000000000000, 5.223019709707975211E-21, -1.000000000000000000 ) ) ;
#24078 = CARTESIAN_POINT ( 'NONE',  ( -1.539760825549682632, -11.93465943778483584, 44.72358953107743673 ) ) ;
#24079 = CARTESIAN_POINT ( 'NONE',  ( 2.433796855181205476, 125.2830755159753977, 74.00833731765604284 ) ) ;
#24080 = CARTESIAN_POINT ( 'NONE',  ( -20.24419206586952669, 18.44224248888906814, 23.20105925399704461 ) ) ;
#24081 = CARTESIAN_POINT ( 'NONE',  ( -4.473127245936434626, 26.34600523034538355, -41.70021447285062521 ) ) ;
#24082 = CARTESIAN_POINT ( 'NONE',  ( -1.031422197589716205, -25.67058493451469658, -37.93675465142464276 ) ) ;
#24083 = ORIENTED_EDGE ( 'NONE', *, *, #12738, .T. ) ;
#24084 = ORIENTED_EDGE ( 'NONE', *, *, #7894, .F. ) ;
#24085 = CARTESIAN_POINT ( 'NONE',  ( 2.108985857320913482, -108.8271972979193833, -96.26411661813142473 ) ) ;
#24086 = CARTESIAN_POINT ( 'NONE',  ( 10.93730112725932635, 0.000000000000000000, 0.000000000000000000 ) ) ;
#24087 = ORIENTED_EDGE ( 'NONE', *, *, #18923, .F. ) ;
#24088 = EDGE_CURVE ( 'NONE', #10927, #2573, #3749, .T. ) ;
#24089 = ORIENTED_EDGE ( 'NONE', *, *, #16432, .T. ) ;
#24090 = VERTEX_POINT ( 'NONE', #12940 ) ;
#24091 = ADVANCED_FACE ( 'NONE', ( #26049 ), #25262, .F. ) ;
#24092 = CARTESIAN_POINT ( 'NONE',  ( 1.833206310202337264, -144.2348262833783110, 15.90849712171692509 ) ) ;
#24093 = CARTESIAN_POINT ( 'NONE',  ( 5.340103579038279591, -146.8647350263016449, -13.12023871299875566 ) ) ;
#24094 = EDGE_CURVE ( 'NONE', #7451, #25971, #5772, .T. ) ;
#24095 = CARTESIAN_POINT ( 'NONE',  ( 25.86096068574580187, -107.2082119295150022, -35.88291140784026112 ) ) ;
#24096 = ADVANCED_FACE ( 'NONE', ( #28059 ), #6685, .F. ) ;
#24097 = CIRCLE ( 'NONE', #16749, 34.60786435723138510 ) ;
#24098 = DIRECTION ( 'NONE',  ( 1.000000000000000000, -6.938893903907226837E-18, 1.734723475976806709E-18 ) ) ;
#24099 = CARTESIAN_POINT ( 'NONE',  ( 109.1589550718175161, -0.003591809816099570795, 0.006669585340474254269 ) ) ;
#24100 = CARTESIAN_POINT ( 'NONE',  ( 25.64681081121879203, 46.30456157731467925, -102.9795863647023850 ) ) ;
#24101 = CARTESIAN_POINT ( 'NONE',  ( -25.21435515916043357, 16.39063784838743132, -30.48034229288645136 ) ) ;
#24102 = CARTESIAN_POINT ( 'NONE',  ( -55.24728320129491266, -0.003868537197316542463, 0.01402509393918130107 ) ) ;
#24103 = CARTESIAN_POINT ( 'NONE',  ( 25.87036335909428075, 113.0557711752706354, -0.9898498320591554434 ) ) ;
#24104 = LINE ( 'NONE', #21927, #20161 ) ;
#24105 = ORIENTED_EDGE ( 'NONE', *, *, #1883, .T. ) ;
#24106 = EDGE_LOOP ( 'NONE', ( #10739, #1261, #15707, #12299 ) ) ;
#24108 = CARTESIAN_POINT ( 'NONE',  ( -23.79223135445719706, 7.157574570129600744, 32.40779366744824586 ) ) ;
#24107 = CARTESIAN_POINT ( 'NONE',  ( -1.583189561560255143, 2.490696082059864924, -46.33203782964461936 ) ) ;
#24109 = B_SPLINE_CURVE_WITH_KNOTS ( 'NONE', 3,
 ( #16265, #24918, #5179, #22766 ),
 .UNSPECIFIED., .F., .F.,
 ( 4, 4 ),
 ( 0.000000000000000000, 0.01077107196513814660 ),
 .UNSPECIFIED. ) ;
#24110 = CARTESIAN_POINT ( 'NONE',  ( -9.156249394959713683, 38.17928057392048657, 38.89149400288364689 ) ) ;
#24111 = CARTESIAN_POINT ( 'NONE',  ( 2.433796855181233454, -133.5135467655514390, -57.85512797798025275 ) ) ;
#24112 = CARTESIAN_POINT ( 'NONE',  ( -6.574463467970651287, -34.08059230520071736, -38.37705091668365043 ) ) ;
#24113 = VERTEX_POINT ( 'NONE', #14958 ) ;
#24114 = CARTESIAN_POINT ( 'NONE',  ( -55.25719721206881729, 0.01115102788683056123, 0.0006290797159205457727 ) ) ;
#24115 = CARTESIAN_POINT ( 'NONE',  ( -1.583189561560256253, 2.490696082060512406, 46.33203782964458384 ) ) ;
#24116 = CARTESIAN_POINT ( 'NONE',  ( -1.050229599974486616, -36.90196321294315140, -27.12684363859242254 ) ) ;
#24117 = ORIENTED_EDGE ( 'NONE', *, *, #14293, .T. ) ;
#24118 = ORIENTED_EDGE ( 'NONE', *, *, #5169, .T. ) ;
#24119 = CARTESIAN_POINT ( 'NONE',  ( 109.1586900883932856, 0.001385221016527459588, -0.007002774699553642249 ) ) ;
#24120 = ORIENTED_EDGE ( 'NONE', *, *, #15419, .F. ) ;
#24121 = CARTESIAN_POINT ( 'NONE',  ( 109.1586900883932856, -0.004851151255037395443, -0.005236795036860529204 ) ) ;
#24122 = ORIENTED_EDGE ( 'NONE', *, *, #19204, .T. ) ;
#24123 = CARTESIAN_POINT ( 'NONE',  ( -20.57838717382308147, 10.78122205917000365, -27.96569011373090063 ) ) ;
#24124 = EDGE_CURVE ( 'NONE', #25504, #8387, #6211, .T. ) ;
#24125 = EDGE_CURVE ( 'NONE', #5967, #3087, #19166, .T. ) ;
#24126 = VERTEX_POINT ( 'NONE', #25777 ) ;
#24127 = CARTESIAN_POINT ( 'NONE',  ( 13.84597867724986919, 142.4258194868990017, 35.16314962059880855 ) ) ;
#24128 = CARTESIAN_POINT ( 'NONE',  ( 24.01988960052056754, -80.44223964539912686, 103.4492499592081600 ) ) ;
#24129 = B_SPLINE_CURVE_WITH_KNOTS ( 'NONE', 3,
 ( #18812, #16366, #12469, #14343 ),
 .UNSPECIFIED., .F., .F.,
 ( 4, 4 ),
 ( 0.000000000000000000, 0.01077107196513875723 ),
 .UNSPECIFIED. ) ;
#24130 = CARTESIAN_POINT ( 'NONE',  ( 6.224689322667630975, 71.79702446228303359, 129.4863684118289768 ) ) ;
#24131 = FACE_OUTER_BOUND ( 'NONE', #1967, .T. ) ;
#24132 = FACE_OUTER_BOUND ( 'NONE', #3147, .T. ) ;
#24133 =( BOUNDED_SURFACE ( )  B_SPLINE_SURFACE ( 3, 1, ( 
 ( #28253, #21506 ),
 ( #1779, #2057 ),
 ( #10576, #15016 ),
 ( #15293, #24110 ) ),
 .UNSPECIFIED., .F., .F., .F. ) 
 B_SPLINE_SURFACE_WITH_KNOTS ( ( 4, 4 ),
 ( 2, 2 ),
 ( 0.000000000000000000, 1.000000000000000000 ),
 ( 0.000000000000000000, 1.000000000000000000 ),
 .UNSPECIFIED. ) 
 GEOMETRIC_REPRESENTATION_ITEM ( )  RATIONAL_B_SPLINE_SURFACE ( (
 ( 1.000000000000000000, 1.000000000000000000),
 ( 0.7789835883360576307, 0.9689951854195403280),
 ( 0.7789835883360576307, 0.9689951854195403280),
 ( 1.000000000000000000, 1.000000000000000000) ) ) 
 REPRESENTATION_ITEM ( '' )  SURFACE ( )  );
#24134 = CARTESIAN_POINT ( 'NONE',  ( 25.98552792386798771, 103.7897946223266246, 45.02923844025520594 ) ) ;
#24136 = CARTESIAN_POINT ( 'NONE',  ( -28.41354790283022069, 8.345538364877077342, -21.64275480268750940 ) ) ;
#24135 = CARTESIAN_POINT ( 'NONE',  ( -19.53423201713129842, 1.550869255229030165E-16, 28.92774122539760384 ) ) ;
#24137 = CARTESIAN_POINT ( 'NONE',  ( 25.64703792032469565, -56.32669596053506211, 97.85829113439940841 ) ) ;
#24138 = VERTEX_POINT ( 'NONE', #25645 ) ;
#24139 = CARTESIAN_POINT ( 'NONE',  ( 25.64681081121879203, 107.5125461021407318, -34.49579773461672971 ) ) ;
#24140 = CARTESIAN_POINT ( 'NONE',  ( 1.833603222531973609, -72.93978951866073146, 125.4455769441940021 ) ) ;
#24141 = CARTESIAN_POINT ( 'NONE',  ( 2.263178607246701723, -31.59906277834119592, -141.9207363487297187 ) ) ;
#24142 = CARTESIAN_POINT ( 'NONE',  ( -8.259864102781671491, -47.98931516265581365, 22.52209142944983711 ) ) ;
#24143 = CARTESIAN_POINT ( 'NONE',  ( 25.65782528836480481, 97.50004228081050428, 56.95887699624769596 ) ) ;
#24144 = CARTESIAN_POINT ( 'NONE',  ( 1.833485406944057594, -0.5339064996874559599, -145.1085452359073429 ) ) ;
#24145 = CARTESIAN_POINT ( 'NONE',  ( 1.833603222531957844, -45.26427810762999826, 137.8693250773476393 ) ) ;
#24146 = CARTESIAN_POINT ( 'NONE',  ( -7.711401346138264223, -38.61705198405337569, 35.51061203065550131 ) ) ;
#24147 = CARTESIAN_POINT ( 'NONE',  ( -55.24340739397742084, 0.007744344507855094144, 0.006539691034612383526 ) ) ;
#24148 = CARTESIAN_POINT ( 'NONE',  ( 25.64708010899964208, 110.4325102642037848, -23.52908206539794023 ) ) ;
#24149 = ORIENTED_EDGE ( 'NONE', *, *, #9468, .F. ) ;
#24150 = CARTESIAN_POINT ( 'NONE',  ( -55.25297051322618813, -0.01093108995494780980, 0.01019003092403480623 ) ) ;
#24151 = EDGE_CURVE ( 'NONE', #21420, #437, #23641, .T. ) ;
#24152 = CARTESIAN_POINT ( 'NONE',  ( 109.1721716018069657, 0.01127028715940102920, -0.01281875973824529898 ) ) ;
#24154 = EDGE_CURVE ( 'NONE', #6991, #16951, #23484, .T. ) ;
#24153 = CARTESIAN_POINT ( 'NONE',  ( 2.433796855181233454, -60.50726454507816499, -132.3327394885237425 ) ) ;
#24155 = EDGE_LOOP ( 'NONE', ( #10295, #16957, #13530, #5292 ) ) ;
#24156 = CARTESIAN_POINT ( 'NONE',  ( 25.64681081121879203, -112.9102952884414606, 0.4157506337723927414 ) ) ;
#24157 = EDGE_CURVE ( 'NONE', #4316, #10927, #25347, .T. ) ;
#24158 = CARTESIAN_POINT ( 'NONE',  ( -21.81686047589426636, -5.181745222995193245, 38.17230180719262478 ) ) ;
#24159 = CARTESIAN_POINT ( 'NONE',  ( 109.1592201516379674, 0.001331853079208314200, 0.007748443302128560708 ) ) ;
#24160 = VERTEX_POINT ( 'NONE', #1588 ) ;
#24161 =( LENGTH_UNIT ( ) NAMED_UNIT ( * ) SI_UNIT ( .MILLI., .METRE. ) );
#24162 = EDGE_CURVE ( 'NONE', #14748, #3038, #12631, .T. ) ;
#24163 = CARTESIAN_POINT ( 'NONE',  ( 26.11404676487259024, 55.62948129436384193, -98.61392875273304526 ) ) ;
#24164 = CARTESIAN_POINT ( 'NONE',  ( -8.786685647604706162, -38.68584556812290032, 37.00619870957955015 ) ) ;
#24165 = CARTESIAN_POINT ( 'NONE',  ( 2.430230287190592531, 133.5180086894991405, 57.85706160874190829 ) ) ;
#24166 = CARTESIAN_POINT ( 'NONE',  ( 2.433796855181233454, -46.34326152018648060, -137.9325382748289996 ) ) ;
#24167 = CARTESIAN_POINT ( 'NONE',  ( 1.833691583653553003, -132.7086741139086712, 58.69608658929877976 ) ) ;
#24168 = CARTESIAN_POINT ( 'NONE',  ( 55.49584447822657296, 72.12568090333341786, 7.849835876628574738 ) ) ;
#24169 = CARTESIAN_POINT ( 'NONE',  ( 109.1586900883932856, -0.006960773163856040675, -0.001582822706024231271 ) ) ;
#24170 = LINE ( 'NONE', #10790, #7015 ) ;
#24171 = CARTESIAN_POINT ( 'NONE',  ( 13.36082413113061307, 67.94366799843001559, -137.0038452127793676 ) ) ;
#24172 = ORIENTED_EDGE ( 'NONE', *, *, #25964, .F. ) ;
#24173 =( BOUNDED_SURFACE ( )  B_SPLINE_SURFACE ( 3, 1, ( 
 ( #23289, #16362 ),
 ( #18667, #16656 ),
 ( #18955, #9903 ),
 ( #25297, #23576 ) ),
 .UNSPECIFIED., .F., .F., .F. ) 
 B_SPLINE_SURFACE_WITH_KNOTS ( ( 4, 4 ),
 ( 2, 2 ),
 ( 0.000000000000000000, 1.000000000000000000 ),
 ( 0.000000000000000000, 1.000000000000000000 ),
 .UNSPECIFIED. ) 
 GEOMETRIC_REPRESENTATION_ITEM ( )  RATIONAL_B_SPLINE_SURFACE ( (
 ( 1.000000000000000000, 1.000000000000000000),
 ( 0.7789835883360578528, 0.9689951854195403280),
 ( 0.7789835883360578528, 0.9689951854195403280),
 ( 1.000000000000000000, 1.000000000000000000) ) ) 
 REPRESENTATION_ITEM ( '' )  SURFACE ( )  );
#24174 = ORIENTED_EDGE ( 'NONE', *, *, #20796, .T. ) ;
#24175 = ORIENTED_EDGE ( 'NONE', *, *, #13601, .F. ) ;
#24176 = CARTESIAN_POINT ( 'NONE',  ( -1.045287976400362417, -28.14015102489855735, -36.12803364096578207 ) ) ;
#24177 = CARTESIAN_POINT ( 'NONE',  ( -20.47566262905010603, 1.586617686065558974, -29.82700878811084522 ) ) ;
#24178 = CARTESIAN_POINT ( 'NONE',  ( 109.1589550718175161, 0.002553077953680937557, 0.007132058561966991318 ) ) ;
#24179 = CARTESIAN_POINT ( 'NONE',  ( 2.108393763691168932, -141.8460676169243015, -31.45977531353440071 ) ) ;
#24180 = CARTESIAN_POINT ( 'NONE',  ( 1.833691583653482615, 72.86287859464769667, -125.4903330494892515 ) ) ;
#24181 = CARTESIAN_POINT ( 'NONE',  ( -20.24399999263414784, 1.282322917263463813, -29.60996018918694617 ) ) ;
#24182 = VERTEX_POINT ( 'NONE', #23777 ) ;
#24183 = CARTESIAN_POINT ( 'NONE',  ( 25.64670758986458310, -34.41755235608670205, -107.5375791514046568 ) ) ;
#24184 = CARTESIAN_POINT ( 'NONE',  ( 109.1721716018069657, -0.01467989464939304170, 0.008708654716139565752 ) ) ;
#24185 = CARTESIAN_POINT ( 'NONE',  ( 1.833750490713712322, 117.5529286802298401, -85.07723081767763063 ) ) ;
#24186 = CARTESIAN_POINT ( 'NONE',  ( 2.430230287190572103, 98.44218333480918659, -107.1617224697454134 ) ) ;
#24187 = CARTESIAN_POINT ( 'NONE',  ( 1.833838850093517436, -0.08898415480133092803, 145.1097630783160923 ) ) ;
#24188 = CARTESIAN_POINT ( 'NONE',  ( 1.833485406944043827, 85.72460230293849293, -117.0814567582535659 ) ) ;
#24189 = PRODUCT_DEFINITION_SHAPE ( 'NONE', 'NONE',  #23390 ) ;
#24190 = EDGE_CURVE ( 'NONE', #675, #22412, #11609, .T. ) ;
#24191 = ORIENTED_EDGE ( 'NONE', *, *, #1050, .T. ) ;
#24192 = CARTESIAN_POINT ( 'NONE',  ( 1.833838850855486369, -107.8971100408355994, 97.03125735562200305 ) ) ;
#24193 = CARTESIAN_POINT ( 'NONE',  ( 25.64703792032472407, -56.58441811305539915, -97.70949518026556291 ) ) ;
#24194 = ORIENTED_EDGE ( 'NONE', *, *, #5315, .F. ) ;
#24195 = EDGE_CURVE ( 'NONE', #1130, #12174, #24757, .T. ) ;
#24196 = B_SPLINE_CURVE_WITH_KNOTS ( 'NONE', 3,
 ( #11316, #9451, #7440, #22556, #9588, #18208, #18348 ),
 .UNSPECIFIED., .F., .F.,
 ( 4, 3, 4 ),
 ( 5.253892930763821798E-16, 0.02816610861753246833, 0.04000277880656270824 ),
 .UNSPECIFIED. ) ;
#24197 = ORIENTED_EDGE ( 'NONE', *, *, #26677, .T. ) ;
#24198 = EDGE_LOOP ( 'NONE', ( #14580, #28, #22754, #3927 ) ) ;
#24199 = EDGE_CURVE ( 'NONE', #3264, #25953, #1968, .T. ) ;
#24200 = CARTESIAN_POINT ( 'NONE',  ( 13.36082413113061307, 117.7941133658651438, -97.52406103376640090 ) ) ;
#24201 = CARTESIAN_POINT ( 'NONE',  ( 2.430230287190589422, 96.28466919684248637, -109.1043569252004488 ) ) ;
#24202 = CARTESIAN_POINT ( 'NONE',  ( 2.433796855181219243, 86.69855925933974561, 116.8607839509059829 ) ) ;
#24203 = EDGE_LOOP ( 'NONE', ( #4119, #18736, #7221, #26258 ) ) ;
#24204 = CARTESIAN_POINT ( 'NONE',  ( -25.21435515916043713, -30.48034229288627017, 16.39063784838775462 ) ) ;
#24205 = CARTESIAN_POINT ( 'NONE',  ( -4.162674018437137136, 45.34593312138912324, 18.33413805792392992 ) ) ;
#24206 = ORIENTED_EDGE ( 'NONE', *, *, #25718, .F. ) ;
#24207 = CARTESIAN_POINT ( 'NONE',  ( -1.045287976400365970, -25.66401692419961833, 37.92705037016786918 ) ) ;
#24208 = EDGE_LOOP ( 'NONE', ( #28400, #26239, #19634, #20486 ) ) ;
#24209 = DIRECTION ( 'NONE',  ( 0.000000000000000000, 0.000000000000000000, 1.000000000000000000 ) ) ;
#24210 = CARTESIAN_POINT ( 'NONE',  ( 1.833838850093465922, -44.84138612520995082, -138.0075846865485403 ) ) ;
#24211 = CARTESIAN_POINT ( 'NONE',  ( -55.24271866751342941, 0.006757859501006707216, 0.006671293903669109175 ) ) ;
#24212 = CARTESIAN_POINT ( 'NONE',  ( 55.79472521941426777, -58.42842213658298078, -43.35047097963510510 ) ) ;
#24213 = CARTESIAN_POINT ( 'NONE',  ( -55.24340739397742794, 0.0007387096945709508214, 0.01010924026184075245 ) ) ;
#24214 = CARTESIAN_POINT ( 'NONE',  ( -10.86508079875781618, -36.95527278096552237, -35.35100740321762913 ) ) ;
#24215 = CARTESIAN_POINT ( 'NONE',  ( -20.24419206586952313, -7.929973069813210707, 28.55732805495823712 ) ) ;
#24216 = DIRECTION ( 'NONE',  ( -0.000000000000000000, 1.000000000000000000, 0.000000000000000000 ) ) ;
#24217 = CARTESIAN_POINT ( 'NONE',  ( -1.045287976400365970, 44.00138577190666922, 12.68782741917247670 ) ) ;
#24218 =( BOUNDED_SURFACE ( )  B_SPLINE_SURFACE ( 3, 1, ( 
 ( #1044, #25091 ),
 ( #16002, #18291 ),
 ( #9834, #27375 ),
 ( #9984, #12268 ) ),
 .UNSPECIFIED., .F., .F., .F. ) 
 B_SPLINE_SURFACE_WITH_KNOTS ( ( 4, 4 ),
 ( 2, 2 ),
 ( 0.000000000000000000, 1.000000000000000000 ),
 ( 0.000000000000000000, 1.000000000000000000 ),
 .UNSPECIFIED. ) 
 GEOMETRIC_REPRESENTATION_ITEM ( )  RATIONAL_B_SPLINE_SURFACE ( (
 ( 1.000000000000000000, 1.000000000000000000),
 ( 0.9960225298536222738, 0.9999952330161893110),
 ( 0.9960225298536222738, 0.9999952330161893110),
 ( 1.000000000000000000, 1.000000000000000000) ) ) 
 REPRESENTATION_ITEM ( '' )  SURFACE ( )  );
#24219 = ORIENTED_EDGE ( 'NONE', *, *, #27770, .T. ) ;
#24220 = EDGE_LOOP ( 'NONE', ( #20170, #3137, #9527, #15265 ) ) ;
#24221 = CARTESIAN_POINT ( 'NONE',  ( -25.21435515916042647, 25.00736669481023355, -23.92354251275945742 ) ) ;
#24222 = B_SPLINE_CURVE_WITH_KNOTS ( 'NONE', 3,
 ( #14683, #12522, #18870, #16987 ),
 .UNSPECIFIED., .F., .F.,
 ( 4, 4 ),
 ( 0.000000000000000000, 0.01077107196513812405 ),
 .UNSPECIFIED. ) ;
#24223 = CARTESIAN_POINT ( 'NONE',  ( -1.045287976400365970, 45.76855895860946077, 1.530335034933974381 ) ) ;
#24224 = ORIENTED_EDGE ( 'NONE', *, *, #16012, .T. ) ;
#24225 = ADVANCED_FACE ( 'NONE', ( #269 ), #15312, .F. ) ;
#24226 = EDGE_LOOP ( 'NONE', ( #22577, #1916, #16359, #22966 ) ) ;
#24227 = VERTEX_POINT ( 'NONE', #2562 ) ;
#24228 = CARTESIAN_POINT ( 'NONE',  ( 109.1586900883932856, -0.002995460350188440014, -0.006479576224398238618 ) ) ;
#24229 = EDGE_CURVE ( 'NONE', #20163, #864, #13504, .T. ) ;
#24230 = EDGE_CURVE ( 'NONE', #19162, #12813, #28463, .T. ) ;
#24231 = CARTESIAN_POINT ( 'NONE',  ( 109.1592201516379674, 0.005027640251767214602, 0.006044422199822552418 ) ) ;
#24232 = CARTESIAN_POINT ( 'NONE',  ( 25.98107933586729601, -83.34070894055808765, -76.50887835172612483 ) ) ;
#24233 = ITEM_DEFINED_TRANSFORMATION ( 'NONE', 'NONE', #11665,  #27263 ) ;
#24234 = CARTESIAN_POINT ( 'NONE',  ( 25.86096068574581963, 10.82483750674603407, 112.5344699600049410 ) ) ;
#24235 = CARTESIAN_POINT ( 'NONE',  ( -20.20700224038492010, -16.58740185276728241, -24.51628800869040958 ) ) ;
#24236 = CARTESIAN_POINT ( 'NONE',  ( -1.239374126674604337, 25.08410696974298304, 38.61989855450910625 ) ) ;
#24237 = CARTESIAN_POINT ( 'NONE',  ( 25.64699802086721903, 66.55977212001160126, 91.20712948285684263 ) ) ;
#24238 = CARTESIAN_POINT ( 'NONE',  ( 28.37644542392834168, -42.25924161793970768, 116.9383271603245191 ) ) ;
#24239 = CARTESIAN_POINT ( 'NONE',  ( 25.64708010899966339, -110.4325102642036001, 23.52908206539865787 ) ) ;
#24240 = CARTESIAN_POINT ( 'NONE',  ( -1.464342487929860992, 11.94843286121917814, -44.64187261869783896 ) ) ;
#24241 = CARTESIAN_POINT ( 'NONE',  ( -1.048171036023497260, 37.64178826568608116, -26.08692787913882327 ) ) ;
#24242 = CARTESIAN_POINT ( 'NONE',  ( 32.73300124599739291, -103.7392577722171865, -55.46353551262117776 ) ) ;
#24243 = EDGE_LOOP ( 'NONE', ( #7399, #25544, #26892, #23649 ) ) ;
#24244 = ORIENTED_EDGE ( 'NONE', *, *, #7854, .T. ) ;
#24245 = CARTESIAN_POINT ( 'NONE',  ( -20.57838717382308147, 7.715628353034087894, 28.96176188950209962 ) ) ;
#24246 = CARTESIAN_POINT ( 'NONE',  ( 8.186469829613987059, 140.9315935955037844, 49.43817854882337315 ) ) ;
#24247 = CARTESIAN_POINT ( 'NONE',  ( -1.113548883309555704, 38.22628252420811634, -25.34012683631568308 ) ) ;
#24248 = CARTESIAN_POINT ( 'NONE',  ( -7.733045908741344121, 10.42750254442610114, 51.44704017882764191 ) ) ;
#24249 = CARTESIAN_POINT ( 'NONE',  ( 30.58324630866340854, -113.7441547345750195, 41.10517620771165070 ) ) ;
#24250 = VERTEX_POINT ( 'NONE', #6902 ) ;
#24251 = ORIENTED_EDGE ( 'NONE', *, *, #70, .F. ) ;
#24252 = CARTESIAN_POINT ( 'NONE',  ( 25.64681081121880624, 103.3177883989785499, -45.54494737132120008 ) ) ;
#24253 = CARTESIAN_POINT ( 'NONE',  ( -1.049817751779885233, -26.50542916749595435, -37.35030165458165641 ) ) ;
#24254 = ORIENTED_EDGE ( 'NONE', *, *, #17212, .F. ) ;
#24255 = ORIENTED_EDGE ( 'NONE', *, *, #4811, .F. ) ;
#24256 = EDGE_CURVE ( 'NONE', #9585, #14332, #27410, .T. ) ;
#24257 = CARTESIAN_POINT ( 'NONE',  ( -1.113427685306992876, -28.52429901637193410, -35.91272432484649357 ) ) ;
#24258 = ORIENTED_EDGE ( 'NONE', *, *, #8210, .T. ) ;
#24259 = CARTESIAN_POINT ( 'NONE',  ( -8.786685647604890903, -48.22796981442753150, 23.24040270374441874 ) ) ;
#24260 = EDGE_LOOP ( 'NONE', ( #22414, #4524, #8732, #9894, #26138, #18061, #21759, #22900, #18810, #17390, #14611, #24489, #3056, #6538, #21351, #25835, #12196, #1110, #14465, #28342, #25372, #571, #26906, #8840, #22781, #14099, #2122, #22073, #2540, #5433, #12639, #16224, #1163, #16614, #23253, #21577, #24854, #4595, #13223, #8282, #26197, #2826, #10728, #6522, #7882, #26721, #23947, #25701, #8274, #15576, #2839, #5855, #9452, #18045, #25360, #21241, #26812, #27250, #3901, #634, #2755, #12835, #28268, #4164, #14494, #27132, #719, #24746, #11467, #26961, #10424, #12697, #6022, #15444, #17692, #18519, #17704, #13793, #14197, #15499, #2553, #20054, #11097, #16278, #13578, #16690, #12729, #7060, #18943, #10698, #12333, #7929, #12989, #7186, #22817, #10145, #3611, #4454, #11916, #26930, #24969, #11121, #400, #6186, #24174, #18562, #16026, #5823, #2621, #24671, #16255, #18724, #17954, #6370, #18767, #27806, #13401, #7644, #14234, #25610, #5681, #27169, #9695, #9826, #6147, #14960, #10582, #26204, #5824, #26081, #3473, #7271, #7328, #23660, #23681, #6399, #22529, #16853, #17550, #22287, #16286, #10053, #22520, #15639, #7958, #19056, #19145, #10302, #23565, #11145, #2722, #2187, #6755, #12953, #11595, #21747, #26364, #15522, #7554, #7981, #23002, #22863, #12789, #22641, #18319, #23711, #17559, #6904, #24117, #11218, #13428, #26112, #20193, #9996, #14051, #27291, #7677, #5474, #682, #12733, #22232, #4499, #1714, #19153 ) ) ;
#24261 = B_SPLINE_CURVE_WITH_KNOTS ( 'NONE', 3,
 ( #8217, #14821, #10250, #10387, #21443, #12246, #19011, #14240, #16859, #21011 ),
 .UNSPECIFIED., .F., .F.,
 ( 4, 3, 3, 4 ),
 ( 1.387778780781445676E-17, 0.0002669560319015811456, 0.0005492286108966765818, 0.0008315040496093515114 ),
 .UNSPECIFIED. ) ;
#24262 = B_SPLINE_CURVE_WITH_KNOTS ( 'NONE', 3,
 ( #9118, #13710, #51, #19758 ),
 .UNSPECIFIED., .F., .F.,
 ( 4, 4 ),
 ( 0.000000000000000000, 0.01077107196513807721 ),
 .UNSPECIFIED. ) ;
#24263 = CARTESIAN_POINT ( 'NONE',  ( 25.69398547355840634, 66.98507266663752091, 90.93418986874829102 ) ) ;
#24264 = ORIENTED_EDGE ( 'NONE', *, *, #12479, .T. ) ;
#24265 = CARTESIAN_POINT ( 'NONE',  ( -55.24271866751342941, -0.009369360294294061531, 0.001545935011626861600 ) ) ;
#24266 = CARTESIAN_POINT ( 'NONE',  ( -55.24340739397742084, 0.009842732675352565408, -0.002421372372454350108 ) ) ;
#24267 = CARTESIAN_POINT ( 'NONE',  ( 1.833485406944057594, -141.8265699653869376, 30.69200235378888308 ) ) ;
#24268 = CARTESIAN_POINT ( 'NONE',  ( 2.063896406836609909, 13.84738934186382586, -144.6078654718900225 ) ) ;
#24269 = CARTESIAN_POINT ( 'NONE',  ( 5.340103579038256498, -100.3626145943027268, -108.0219267094756503 ) ) ;
#24270 = CARTESIAN_POINT ( 'NONE',  ( -20.38016308990357928, -16.25718651464962861, 24.94368798801368925 ) ) ;
#24271 = CARTESIAN_POINT ( 'NONE',  ( -1.045287976400383290, 28.14015102489806708, -36.12803364096618708 ) ) ;
#24272 = CARTESIAN_POINT ( 'NONE',  ( 10.93730112725932635, 0.000000000000000000, 0.000000000000000000 ) ) ;
#24273 = VERTEX_POINT ( 'NONE', #13785 ) ;
#24274 = CARTESIAN_POINT ( 'NONE',  ( 10.93730112725978287, -97.44200844886353252, 115.5857507957700250 ) ) ;
#24275 = CARTESIAN_POINT ( 'NONE',  ( 2.433796855181219243, 142.0211193075560061, -31.67151202412830813 ) ) ;
#24276 = CARTESIAN_POINT ( 'NONE',  ( 32.73300124599739291, -113.0038235389599635, -32.68291970228351317 ) ) ;
#24277 = CARTESIAN_POINT ( 'NONE',  ( 13.36082413113063083, 81.89226687792086068, 129.1512766091124149 ) ) ;
#24278 = B_SPLINE_CURVE_WITH_KNOTS ( 'NONE', 3,
 ( #16201, #25010, #22850, #9022, #5263, #7016, #14038, #11179, #24581, #22411 ),
 .UNSPECIFIED., .F., .F.,
 ( 4, 2, 2, 2, 4 ),
 ( 2.884421207865724908E-16, 0.0003346187017559065996, 0.0006692374035115252352, 0.001003856105267143979, 0.001338474807022762723 ),
 .UNSPECIFIED. ) ;
#24279 = CARTESIAN_POINT ( 'NONE',  ( 1.833838850093516104, -0.1779693352084075475, -145.1097630783160923 ) ) ;
#24280 = EDGE_CURVE ( 'NONE', #8439, #2946, #6125, .T. ) ;
#24281 = ORIENTED_EDGE ( 'NONE', *, *, #11494, .F. ) ;
#24282 = CARTESIAN_POINT ( 'NONE',  ( 109.1587776205901861, -0.004965871434398078446, -0.005390665547495563856 ) ) ;
#24283 = EDGE_CURVE ( 'NONE', #10817, #1068, #14368, .T. ) ;
#24284 = FACE_OUTER_BOUND ( 'NONE', #5435, .T. ) ;
#24285 = CARTESIAN_POINT ( 'NONE',  ( 30.59138290137912009, 55.75105126024056545, -101.9665464510083979 ) ) ;
#24286 = CARTESIAN_POINT ( 'NONE',  ( 109.1587776205901861, 0.004240403845331873305, -0.005978137617721855993 ) ) ;
#24288 = EDGE_CURVE ( 'NONE', #15681, #12261, #11484, .T. ) ;
#24287 = EDGE_LOOP ( 'NONE', ( #5089, #26451, #24910, #10607 ) ) ;
#24289 = CARTESIAN_POINT ( 'NONE',  ( -7.078251931573406708, -20.86696228105259365, -47.71415099571797924 ) ) ;
#24290 = AXIS2_PLACEMENT_3D ( 'NONE', #21733, #13216, #22006 ) ;
#24291 =( BOUNDED_SURFACE ( )  B_SPLINE_SURFACE ( 3, 1, ( 
 ( #10012, #25414 ),
 ( #24991, #5689 ),
 ( #23261, #12294 ),
 ( #21064, #27974 ) ),
 .UNSPECIFIED., .F., .F., .F. ) 
 B_SPLINE_SURFACE_WITH_KNOTS ( ( 4, 4 ),
 ( 2, 2 ),
 ( 0.000000000000000000, 1.000000000000000000 ),
 ( 0.000000000000000000, 1.000000000000000000 ),
 .UNSPECIFIED. ) 
 GEOMETRIC_REPRESENTATION_ITEM ( )  RATIONAL_B_SPLINE_SURFACE ( (
 ( 1.000000000000000000, 1.000000000000000000),
 ( 0.6386103224230302855, 0.9954351624131538845),
 ( 0.6386103224230302855, 0.9954351624131538845),
 ( 1.000000000000000000, 1.000000000000000000) ) ) 
 REPRESENTATION_ITEM ( '' )  SURFACE ( )  );
#24292 = CARTESIAN_POINT ( 'NONE',  ( -20.57838717382308147, -29.92853265176830746, 1.611677988432673070 ) ) ;
#24293 = ORIENTED_EDGE ( 'NONE', *, *, #25927, .F. ) ;
#24294 = CARTESIAN_POINT ( 'NONE',  ( 109.1778270068192853, -0.002542344697966384976, 0.008960903982066587004 ) ) ;
#24295 = CARTESIAN_POINT ( 'NONE',  ( 1.834118845439484335, -125.7578880615050281, 72.40084790867285847 ) ) ;
#24296 = FACE_OUTER_BOUND ( 'NONE', #16144, .T. ) ;
#24297 = EDGE_LOOP ( 'NONE', ( #910, #19835, #23902, #49 ) ) ;
#24298 =( BOUNDED_SURFACE ( )  B_SPLINE_SURFACE ( 3, 1, ( 
 ( #7980, #9540 ),
 ( #3202, #9835 ),
 ( #7687, #20753 ),
 ( #11983, #16445 ) ),
 .UNSPECIFIED., .F., .F., .F. ) 
 B_SPLINE_SURFACE_WITH_KNOTS ( ( 4, 4 ),
 ( 2, 2 ),
 ( 0.000000000000000000, 1.000000000000000000 ),
 ( 0.000000000000000000, 1.000000000000000000 ),
 .UNSPECIFIED. ) 
 GEOMETRIC_REPRESENTATION_ITEM ( )  RATIONAL_B_SPLINE_SURFACE ( (
 ( 1.000000000000000000, 1.000000000000000000),
 ( 0.9956975270656955868, 0.8568959468854907557),
 ( 0.9956975270656955868, 0.8568959468854907557),
 ( 1.000000000000000000, 1.000000000000000000) ) ) 
 REPRESENTATION_ITEM ( '' )  SURFACE ( )  );
#24299 = DIRECTION ( 'NONE',  ( -1.000000000000000000, 6.938893903907226837E-18, -1.734723475976806709E-18 ) ) ;
#24300 = LINE ( 'NONE', #28448, #13894 ) ;
#24301 = CARTESIAN_POINT ( 'NONE',  ( 25.64692872815577473, 23.16082795281256068, 110.5102270591923457 ) ) ;
#24302 = CARTESIAN_POINT ( 'NONE',  ( 25.64692232868535626, 110.5112661748245131, 23.15582834340323259 ) ) ;
#24303 = ORIENTED_EDGE ( 'NONE', *, *, #17280, .T. ) ;
#24304 = CARTESIAN_POINT ( 'NONE',  ( 1.833485406944057594, -125.9346397303430223, -72.09189602597842850 ) ) ;
#24305 = VECTOR ( 'NONE', #23426, 1000.000000000000114 ) ;
#24306 = CARTESIAN_POINT ( 'NONE',  ( -1.583189561560252701, -11.94859433442933394, -44.83405390829668136 ) ) ;
#24307 = CARTESIAN_POINT ( 'NONE',  ( 55.49584447822657296, 14.82242356768033886, -71.02133150427242470 ) ) ;
#24308 = VECTOR ( 'NONE', #23278, 1000.000000000000114 ) ;
#24309 = CARTESIAN_POINT ( 'NONE',  ( -4.178947244162628749, 18.28784278438515543, 45.38689110596700260 ) ) ;
#24310 = ORIENTED_EDGE ( 'NONE', *, *, #20276, .T. ) ;
#24311 = EDGE_CURVE ( 'NONE', #10429, #21463, #10271, .T. ) ;
#24312 = ORIENTED_EDGE ( 'NONE', *, *, #11460, .F. ) ;
#24314 = VERTEX_POINT ( 'NONE', #18547 ) ;
#24313 = B_SPLINE_CURVE_WITH_KNOTS ( 'NONE', 3,
 ( #1794, #28139, #26126, #216, #17204, #24127, #9004 ),
 .UNSPECIFIED., .F., .F.,
 ( 4, 3, 4 ),
 ( 0.000000000000000000, 0.02398743853561356720, 0.04000277880656211843 ),
 .UNSPECIFIED. ) ;
#24315 = LINE ( 'NONE', #402, #8793 ) ;
#24316 = B_SPLINE_CURVE_WITH_KNOTS ( 'NONE', 3,
 ( #19776, #24404, #2505, #4674 ),
 .UNSPECIFIED., .F., .F.,
 ( 4, 4 ),
 ( 1.092738104725961435E-16, 0.008383748772659562962 ),
 .UNSPECIFIED. ) ;
#24317 = CARTESIAN_POINT ( 'NONE',  ( -20.37983603106074426, -10.62371319148622284, 27.81368274044722000 ) ) ;
#24318 = CARTESIAN_POINT ( 'NONE',  ( -23.79248802219722947, -3.207402715357382306, -33.03370827286730105 ) ) ;
#24319 = CARTESIAN_POINT ( 'NONE',  ( 2.063896406836609909, -84.29612368209232898, 118.3103904147678804 ) ) ;
#24320 = CARTESIAN_POINT ( 'NONE',  ( 32.73300124599732186, 0.000000000000000000, 0.000000000000000000 ) ) ;
#24321 = CARTESIAN_POINT ( 'NONE',  ( -20.57838717382308147, 1.611677988432361097, -29.92853265176831812 ) ) ;
#24322 = ADVANCED_FACE ( 'NONE', ( #1132 ), #22321, .F. ) ;
#24323 = ORIENTED_EDGE ( 'NONE', *, *, #23044, .T. ) ;
#24324 = CARTESIAN_POINT ( 'NONE',  ( -8.786685647604890903, -9.545808661480235102, 52.67761315067295413 ) ) ;
#24325 = CARTESIAN_POINT ( 'NONE',  ( 25.64692232868535982, 12.12735788170810913, 112.2580042965357592 ) ) ;
#24326 = CARTESIAN_POINT ( 'NONE',  ( 109.1592201516379674, -0.0003082430542016361633, -0.007856029051022768092 ) ) ;
#24327 = EDGE_CURVE ( 'NONE', #6378, #24693, #14073, .T. ) ;
#24328 = CARTESIAN_POINT ( 'NONE',  ( 25.98107933586707574, -74.88680433646190693, -84.80123094405294637 ) ) ;
#24329 = CARTESIAN_POINT ( 'NONE',  ( 1.833485406944043827, 45.34878176254417070, -137.8414413349080974 ) ) ;
#24330 = FACE_OUTER_BOUND ( 'NONE', #9352, .T. ) ;
#24331 = CARTESIAN_POINT ( 'NONE',  ( -55.24728320129491266, -0.01362040845703352439, -0.005114031043468804730 ) ) ;
#24332 = ORIENTED_EDGE ( 'NONE', *, *, #1885, .T. ) ;
#24333 = ORIENTED_EDGE ( 'NONE', *, *, #15416, .T. ) ;
#24334 = ORIENTED_EDGE ( 'NONE', *, *, #20228, .T. ) ;
#24335 = B_SPLINE_CURVE_WITH_KNOTS ( 'NONE', 3,
 ( #6301, #27755, #19245, #6175, #21270, #16948 ),
 .UNSPECIFIED., .F., .F.,
 ( 4, 2, 4 ),
 ( 3.208066105977133993E-16, 0.003576372551511132307, 0.007152745103021943690 ),
 .UNSPECIFIED. ) ;
#24336 = CARTESIAN_POINT ( 'NONE',  ( -20.24399999263415850, -18.44171895251379567, 23.20123049637386003 ) ) ;
#24337 = CARTESIAN_POINT ( 'NONE',  ( 109.1589550718174877, -0.007008495014548490887, 0.002874971999843633271 ) ) ;
#24338 = CARTESIAN_POINT ( 'NONE',  ( -6.588769196390761529, 20.50531526814562966, -47.06982923582516065 ) ) ;
#24339 =( BOUNDED_SURFACE ( )  B_SPLINE_SURFACE ( 3, 1, ( 
 ( #22363, #9544 ),
 ( #9260, #3204 ),
 ( #2771, #2626 ),
 ( #15873, #27076 ) ),
 .UNSPECIFIED., .F., .F., .F. ) 
 B_SPLINE_SURFACE_WITH_KNOTS ( ( 4, 4 ),
 ( 2, 2 ),
 ( 0.000000000000000000, 1.000000000000000000 ),
 ( 0.000000000000000000, 1.000000000000000000 ),
 .UNSPECIFIED. ) 
 GEOMETRIC_REPRESENTATION_ITEM ( )  RATIONAL_B_SPLINE_SURFACE ( (
 ( 1.000000000000000000, 1.000000000000000000),
 ( 0.6386103224230302855, 0.9954351624131538845),
 ( 0.6386103224230302855, 0.9954351624131538845),
 ( 1.000000000000000000, 1.000000000000000000) ) ) 
 REPRESENTATION_ITEM ( '' )  SURFACE ( )  );
#24340 = EDGE_LOOP ( 'NONE', ( #25820, #21381, #26643, #18790 ) ) ;
#24341 = DIRECTION ( 'NONE',  ( -1.000000000000000000, -0.000000000000000000, -0.000000000000000000 ) ) ;
#24342 = CARTESIAN_POINT ( 'NONE',  ( -1.045287976400362417, -1.530335034933495653, 45.76855895860946788 ) ) ;
#24343 = ORIENTED_EDGE ( 'NONE', *, *, #24654, .F. ) ;
#24344 = EDGE_CURVE ( 'NONE', #2563, #4669, #24998, .T. ) ;
#24345 = CARTESIAN_POINT ( 'NONE',  ( 25.64660436782554243, 91.68669413043151906, 65.89729635302943223 ) ) ;
#24346 = ORIENTED_EDGE ( 'NONE', *, *, #18354, .F. ) ;
#24347 = CARTESIAN_POINT ( 'NONE',  ( 1.833485406944057594, 125.9346397303435197, 72.09189602597754742 ) ) ;
#24348 = EDGE_CURVE ( 'NONE', #7024, #1356, #4280, .T. ) ;
#24349 = CARTESIAN_POINT ( 'NONE',  ( -1.048994561756784405, -37.49601524795390617, 26.29622118251720764 ) ) ;
#24350 = CARTESIAN_POINT ( 'NONE',  ( -1.031422197589716205, 44.01264471863865424, 12.69107518035457005 ) ) ;
#24351 = CARTESIAN_POINT ( 'NONE',  ( -55.24198130335446422, 0.004276389980776598189, 0.008252882783650057619 ) ) ;
#24352 = B_SPLINE_CURVE_WITH_KNOTS ( 'NONE', 3,
 ( #23203, #3459, #18861, #16713, #25505, #16024, #7267, #7131, #15737, #8994 ),
 .UNSPECIFIED., .F., .F.,
 ( 4, 3, 3, 4 ),
 ( 4.163336342344337027E-17, 0.0002669559177086231047, 0.0005339118354151080542, 0.001067817517169163816 ),
 .UNSPECIFIED. ) ;
#24353 = CARTESIAN_POINT ( 'NONE',  ( 2.263178607246658203, 73.90841395012587611, 125.2099936970370635 ) ) ;
#24354 = CARTESIAN_POINT ( 'NONE',  ( -55.24390624410018802, 0.007245494385991800047, -0.007503127514277958821 ) ) ;
#24355 = CARTESIAN_POINT ( 'NONE',  ( -25.21435515916043357, -25.00736669481038987, -23.92354251275926558 ) ) ;
#24356 = CARTESIAN_POINT ( 'NONE',  ( -20.20612091757425333, -24.59769958242376120, 16.46550228026422502 ) ) ;
#24357 = EDGE_CURVE ( 'NONE', #15804, #26995, #23962, .T. ) ;
#24358 = CARTESIAN_POINT ( 'NONE',  ( 1.833838850855475933, 15.07960613928627325, 144.3241377520099604 ) ) ;
#24359 = CARTESIAN_POINT ( 'NONE',  ( -25.21435515916043713, -23.92354251275918031, 25.00736669481048224 ) ) ;
#24360 = CARTESIAN_POINT ( 'NONE',  ( -55.24300891470650754, 0.003362556190412917256, 0.009225237711101274066 ) ) ;
#24361 = CARTESIAN_POINT ( 'NONE',  ( 25.87036335909428431, -0.9898498320579764975, -113.0557711752706354 ) ) ;
#24362 = EDGE_CURVE ( 'NONE', #11536, #22381, #22589, .T. ) ;
#24363 = ORIENTED_EDGE ( 'NONE', *, *, #15590, .F. ) ;
#24364 = ORIENTED_EDGE ( 'NONE', *, *, #20397, .F. ) ;
#24365 = DIRECTION ( 'NONE',  ( 0.000000000000000000, -1.000000000000000000, -3.469446951953603342E-16 ) ) ;
#24366 = CARTESIAN_POINT ( 'NONE',  ( -4.473127245936434626, -26.34600523034507802, 41.70021447285083127 ) ) ;
#24367 = EDGE_LOOP ( 'NONE', ( #8848, #338, #20388, #18241 ) ) ;
#24368 = EDGE_LOOP ( 'NONE', ( #340, #25732, #22712, #11898 ) ) ;
#24369 = ORIENTED_EDGE ( 'NONE', *, *, #9890, .F. ) ;
#24370 = B_SPLINE_CURVE_WITH_KNOTS ( 'NONE', 3,
 ( #6303, #28295, #8595, #26426, #6725, #20084 ),
 .UNSPECIFIED., .F., .F.,
 ( 4, 2, 4 ),
 ( 2.168404344971008868E-18, 0.0006311636237756755499, 0.001262327247551348931 ),
 .UNSPECIFIED. ) ;
#24371 = CARTESIAN_POINT ( 'NONE',  ( 32.73300124599741423, 117.3295799645430435, -8.473903470904879498 ) ) ;
#24372 = CARTESIAN_POINT ( 'NONE',  ( -55.24340739397742794, 0.005344433640974572026, -0.008612749836242874699 ) ) ;
#24373 = CARTESIAN_POINT ( 'NONE',  ( -1.058197053496169548, -45.77356582045592859, -1.754224732379389362 ) ) ;
#24374 = DIRECTION ( 'NONE',  ( 0.000000000000000000, 0.000000000000000000, 1.000000000000000000 ) ) ;
#24375 = DIRECTION ( 'NONE',  ( 0.000000000000000000, 5.223019709707975211E-21, -1.000000000000000000 ) ) ;
#24376 = CARTESIAN_POINT ( 'NONE',  ( -12.82751273423880711, 33.78816682541337002, 35.32125660155409008 ) ) ;
#24377 = B_SPLINE_CURVE_WITH_KNOTS ( 'NONE', 3,
 ( #10976, #16895, #4060, #1626, #6520, #28234, #26218, #6374 ),
 .UNSPECIFIED., .F., .F.,
 ( 4, 2, 2, 4 ),
 ( 0.000000000000000000, 0.002761524886576651079, 0.005523049773153302158, 0.01104609954630660432 ),
 .UNSPECIFIED. ) ;
#24378 = EDGE_CURVE ( 'NONE', #15269, #14457, #613, .T. ) ;
#24379 = CARTESIAN_POINT ( 'NONE',  ( -2.265401668238147259, 43.82493763960408728, 17.02144111536834004 ) ) ;
#24380 =( BOUNDED_SURFACE ( )  B_SPLINE_SURFACE ( 3, 1, ( 
 ( #25060, #2881 ),
 ( #2729, #11366 ),
 ( #7213, #7497 ),
 ( #572, #20432 ) ),
 .UNSPECIFIED., .F., .F., .F. ) 
 B_SPLINE_SURFACE_WITH_KNOTS ( ( 4, 4 ),
 ( 2, 2 ),
 ( 0.000000000000000000, 1.000000000000000000 ),
 ( 0.000000000000000000, 1.000000000000000000 ),
 .UNSPECIFIED. ) 
 GEOMETRIC_REPRESENTATION_ITEM ( )  RATIONAL_B_SPLINE_SURFACE ( (
 ( 1.000000000000000000, 1.000000000000000000),
 ( 0.7789835883360576307, 0.9689951854195403280),
 ( 0.7789835883360576307, 0.9689951854195403280),
 ( 1.000000000000000000, 1.000000000000000000) ) ) 
 REPRESENTATION_ITEM ( '' )  SURFACE ( )  );
#24381 = CARTESIAN_POINT ( 'NONE',  ( 26.11404676487257603, -65.63269960453305885, 92.25884714080386573 ) ) ;
#24382 = FACE_OUTER_BOUND ( 'NONE', #15081, .T. ) ;
#24383 = DIRECTION ( 'NONE',  ( 0.000000000000000000, 0.000000000000000000, 1.000000000000000000 ) ) ;
#24385 = VERTEX_POINT ( 'NONE', #27314 ) ;
#24384 = EDGE_CURVE ( 'NONE', #15583, #20437, #5454, .T. ) ;
#24386 = AXIS2_PLACEMENT_3D ( 'NONE', #6898, #24463, #7049 ) ;
#24387 = CARTESIAN_POINT ( 'NONE',  ( 6.224689322667647851, -147.4941644018827560, -12.92299475787110019 ) ) ;
#24388 = CIRCLE ( 'NONE', #27112, 151.1787379149930359 ) ;
#24389 = CARTESIAN_POINT ( 'NONE',  ( 1.833809397773872307, -144.2961330457378608, -15.34508223002595884 ) ) ;
#24390 = DIRECTION ( 'NONE',  ( -0.7563875759206388771, 0.5078650950445624535, -0.4122509917856805317 ) ) ;
#24391 = B_SPLINE_CURVE_WITH_KNOTS ( 'NONE', 3,
 ( #19519, #15466, #17218, #24274 ),
 .UNSPECIFIED., .F., .F.,
 ( 4, 4 ),
 ( 3.450729209734431367E-16, 0.01077107486149810056 ),
 .UNSPECIFIED. ) ;
#24392 = CARTESIAN_POINT ( 'NONE',  ( 13.36082413113061307, 37.97423473099499347, -148.1362653800998999 ) ) ;
#24393 = DIRECTION ( 'NONE',  ( 0.000000000000000000, 0.000000000000000000, 1.000000000000000000 ) ) ;
#24394 = CARTESIAN_POINT ( 'NONE',  ( -20.57838717382308147, 18.89542499756500149, -23.26537097894111383 ) ) ;
#24395 = ORIENTED_EDGE ( 'NONE', *, *, #15192, .F. ) ;
#24396 = FACE_OUTER_BOUND ( 'NONE', #6079, .T. ) ;
#24397 = CARTESIAN_POINT ( 'NONE',  ( -20.20700224038492721, -23.35150625415645820, 18.19058640100249491 ) ) ;
#24398 = ORIENTED_EDGE ( 'NONE', *, *, #23459, .F. ) ;
#24399 = ORIENTED_EDGE ( 'NONE', *, *, #23662, .T. ) ;
#24400 = CARTESIAN_POINT ( 'NONE',  ( -1.058473599757816963, -28.32531354681309566, -35.99997772736203672 ) ) ;
#24401 = ORIENTED_EDGE ( 'NONE', *, *, #22336, .F. ) ;
#24402 = CARTESIAN_POINT ( 'NONE',  ( 32.73300124599739291, -99.90245962373785460, -62.10906484417343165 ) ) ;
#24403 = ORIENTED_EDGE ( 'NONE', *, *, #21879, .F. ) ;
#24404 = CARTESIAN_POINT ( 'NONE',  ( 30.59138290137876837, 70.47507990428549363, 92.40465044710759912 ) ) ;
#24405 = AXIS2_PLACEMENT_3D ( 'NONE', #6978, #18169, #13711 ) ;
#24406 = AXIS2_PLACEMENT_3D ( 'NONE', #21312, #23069, #19019 ) ;
#24407 = VECTOR ( 'NONE', #20638, 1000.000000000000114 ) ;
#24408 = CARTESIAN_POINT ( 'NONE',  ( -1.048172774974290622, -15.11899685083854727, -43.23017713506519755 ) ) ;
#24409 = DIRECTION ( 'NONE',  ( 0.000000000000000000, 0.000000000000000000, -1.000000000000000000 ) ) ;
#24410 = LINE ( 'NONE', #4827, #11538 ) ;
#24411 = LINE ( 'NONE', #20209, #15617 ) ;
#24412 = EDGE_CURVE ( 'NONE', #5523, #20564, #15370, .T. ) ;
#24413 = CARTESIAN_POINT ( 'NONE',  ( 2.433796855181233454, 133.5135467655518369, 57.85512797797937168 ) ) ;
#24415 = CARTESIAN_POINT ( 'NONE',  ( 25.69398547355841700, -34.19446713634657442, 107.6418378907642932 ) ) ;
#24414 = CARTESIAN_POINT ( 'NONE',  ( -7.078251931573400491, -47.71415099571819951, -20.86696228105206075 ) ) ;
#24416 = CARTESIAN_POINT ( 'NONE',  ( -55.24271866751342941, -0.004256484107795216812, 0.008488649505342837909 ) ) ;
#24417 =( BOUNDED_SURFACE ( )  B_SPLINE_SURFACE ( 3, 1, ( 
 ( #19668, #26296 ),
 ( #6592, #15344 ),
 ( #24152, #4415 ),
 ( #13186, #21978 ) ),
 .UNSPECIFIED., .F., .F., .F. ) 
 B_SPLINE_SURFACE_WITH_KNOTS ( ( 4, 4 ),
 ( 2, 2 ),
 ( 0.000000000000000000, 1.000000000000000000 ),
 ( 0.000000000000000000, 1.000000000000000000 ),
 .UNSPECIFIED. ) 
 GEOMETRIC_REPRESENTATION_ITEM ( )  RATIONAL_B_SPLINE_SURFACE ( (
 ( 1.000000000000000000, 1.000000000000000000),
 ( 0.6386103224230302855, 0.9954351624131538845),
 ( 0.6386103224230302855, 0.9954351624131538845),
 ( 1.000000000000000000, 1.000000000000000000) ) ) 
 REPRESENTATION_ITEM ( '' )  SURFACE ( )  );
#24418 = EDGE_CURVE ( 'NONE', #6949, #24273, #20525, .T. ) ;
#24419 = ORIENTED_EDGE ( 'NONE', *, *, #935, .T. ) ;
#24420 = CARTESIAN_POINT ( 'NONE',  ( 10.93730112725971715, 20.69552240458328995, 149.7554878793148703 ) ) ;
#24421 = CARTESIAN_POINT ( 'NONE',  ( -55.24271866751342941, 0.004256484107795918508, -0.008488649505343059953 ) ) ;
#24422 = EDGE_CURVE ( 'NONE', #12444, #17575, #22274, .T. ) ;
#24423 = CARTESIAN_POINT ( 'NONE',  ( -20.57838717382308147, -18.89542499756516847, -23.26537097894098594 ) ) ;
#24424 = B_SPLINE_CURVE_WITH_KNOTS ( 'NONE', 3,
 ( #13862, #18471, #20340, #7126, #24692, #5515, #3361, #11714 ),
 .UNSPECIFIED., .F., .F.,
 ( 4, 2, 2, 4 ),
 ( 2.225109362706117716E-16, 0.002761568181852862899, 0.005523136363705503753, 0.01104627272741078546 ),
 .UNSPECIFIED. ) ;
#24425 = CARTESIAN_POINT ( 'NONE',  ( -20.21097721712959228, -28.26295595852180043, 8.835581498567762537 ) ) ;
#24426 = B_SPLINE_CURVE_WITH_KNOTS ( 'NONE', 3,
 ( #10937, #11073, #17540, #131, #9489, #25046 ),
 .UNSPECIFIED., .F., .F.,
 ( 4, 2, 4 ),
 ( 1.504716382203053018E-16, 0.003570751334075636125, 0.007141502668151121329 ),
 .UNSPECIFIED. ) ;
#24427 = VERTEX_POINT ( 'NONE', #11000 ) ;
#24428 = CARTESIAN_POINT ( 'NONE',  ( 1.833809397773814576, -45.01060836636616358, 137.9524943416724625 ) ) ;
#24429 = AXIS2_PLACEMENT_3D ( 'NONE', #18594, #14409, #16139 ) ;
#24430 = CARTESIAN_POINT ( 'NONE',  ( 32.73300124599739291, -108.9684813982485707, -44.31599526638064646 ) ) ;
#24431 = LINE ( 'NONE', #4841, #19896 ) ;
#24432 = CARTESIAN_POINT ( 'NONE',  ( 2.433796855181205476, 46.34326152018925171, -137.9325382748280333 ) ) ;
#24433 = VECTOR ( 'NONE', #3657, 1000.000000000000114 ) ;
#24434 = VERTEX_POINT ( 'NONE', #23445 ) ;
#24435 = CARTESIAN_POINT ( 'NONE',  ( 1.832998868059890096, -137.8420662456173034, 45.34898734666001019 ) ) ;
#24436 = CARTESIAN_POINT ( 'NONE',  ( -20.57838717382308502, 23.26537097894105699, -18.89542499756508320 ) ) ;
#24437 = EDGE_LOOP ( 'NONE', ( #20201, #5651, #828, #8426 ) ) ;
#24439 = EDGE_CURVE ( 'NONE', #27978, #11607, #3986, .T. ) ;
#24438 = CARTESIAN_POINT ( 'NONE',  ( 30.59138290137911653, 33.33271994911483915, -111.3296280985502165 ) ) ;
#24440 = CARTESIAN_POINT ( 'NONE',  ( -1.619063947482197729, 46.30105812165548684, 2.489035965910320503 ) ) ;
#24441 = CARTESIAN_POINT ( 'NONE',  ( 109.1587776205901577, 0.002904816147418920556, 0.006729130500857913137 ) ) ;
#24442 = VERTEX_POINT ( 'NONE', #1681 ) ;
#24443 =( LENGTH_UNIT ( ) NAMED_UNIT ( * ) SI_UNIT ( .MILLI., .METRE. ) );
#24444 = ADVANCED_FACE ( 'NONE', ( #15435, #27756 ), #26525, .F. ) ;
#24445 = CARTESIAN_POINT ( 'NONE',  ( -55.24728320129491266, -0.01453410071985230222, 0.0006547948648737443372 ) ) ;
#24446 = CARTESIAN_POINT ( 'NONE',  ( 32.73300124599732186, 0.000000000000000000, 0.000000000000000000 ) ) ;
#24447 = CARTESIAN_POINT ( 'NONE',  ( -25.21435515916043357, -15.02493970636125198, 31.17620025257602379 ) ) ;
#24448 = CARTESIAN_POINT ( 'NONE',  ( 109.1586900883932856, 0.004113747440992326053, -0.005833932871491330496 ) ) ;
#24449 = EDGE_CURVE ( 'NONE', #25142, #9465, #12985, .T. ) ;
#24450 = EDGE_LOOP ( 'NONE', ( #17151, #21208, #5625, #289 ) ) ;
#24451 = EDGE_CURVE ( 'NONE', #5381, #12412, #21198, .T. ) ;
#24452 = CARTESIAN_POINT ( 'NONE',  ( -7.078251931573406708, -44.92740138729184451, -26.33626633876207634 ) ) ;
#24453 = CARTESIAN_POINT ( 'NONE',  ( -55.24390624410018802, 0.004572280736703349113, -0.009374879212967143077 ) ) ;
#24454 = CARTESIAN_POINT ( 'NONE',  ( -55.24198130335446422, 0.008252882783650522525, -0.004276389980776339715 ) ) ;
#24455 = VERTEX_POINT ( 'NONE', #8987 ) ;
#24456 = CIRCLE ( 'NONE', #14808, 151.1787379149930359 ) ;
#24457 = ORIENTED_EDGE ( 'NONE', *, *, #18152, .F. ) ;
#24458 = VERTEX_POINT ( 'NONE', #19248 ) ;
#24459 = B_SPLINE_CURVE_WITH_KNOTS ( 'NONE', 3,
 ( #3620, #18741, #1737, #5495, #6092, #18886, #20897 ),
 .UNSPECIFIED., .F., .F.,
 ( 4, 3, 4 ),
 ( 0.000000000000000000, 0.02398743853561404946, 0.04000277880656225027 ),
 .UNSPECIFIED. ) ;
#24460 = CARTESIAN_POINT ( 'NONE',  ( -1.045287976400365970, -43.05558670614224326, 15.59869763335140469 ) ) ;
#24461 = DIRECTION ( 'NONE',  ( -0.5914120900931443270, 0.6476200150380249099, -0.4804373588864701006 ) ) ;
#24462 = FACE_OUTER_BOUND ( 'NONE', #25086, .T. ) ;
#24463 = DIRECTION ( 'NONE',  ( 1.000000000000000000, -6.938893903907226837E-18, 1.734723475976806709E-18 ) ) ;
#24464 = CARTESIAN_POINT ( 'NONE',  ( 1.833838848569457225, 144.3334397096297721, 14.99110384899575621 ) ) ;
#24465 = CARTESIAN_POINT ( 'NONE',  ( -6.588769196390767746, -51.10255870850473769, -4.956336548259470121 ) ) ;
#24466 = CARTESIAN_POINT ( 'NONE',  ( 13.84597867724985321, -121.4327876424619461, 82.31427113894737602 ) ) ;
#24467 = ORIENTED_EDGE ( 'NONE', *, *, #15550, .T. ) ;
#24468 = CARTESIAN_POINT ( 'NONE',  ( 30.59138290137878613, 2.701446546448210029, 116.1811451928593044 ) ) ;
#24469 = FACE_OUTER_BOUND ( 'NONE', #26789, .T. ) ;
#24470 = CARTESIAN_POINT ( 'NONE',  ( 109.1721716018069657, 0.01392660302850754449, 0.009868622090676223979 ) ) ;
#24471 =( BOUNDED_SURFACE ( )  B_SPLINE_SURFACE ( 3, 1, ( 
 ( #18533, #20678 ),
 ( #23161, #12057 ),
 ( #25301, #10047 ),
 ( #14631, #23430 ) ),
 .UNSPECIFIED., .F., .F., .F. ) 
 B_SPLINE_SURFACE_WITH_KNOTS ( ( 4, 4 ),
 ( 2, 2 ),
 ( 0.000000000000000000, 1.000000000000000000 ),
 ( 0.000000000000000000, 1.000000000000000000 ),
 .UNSPECIFIED. ) 
 GEOMETRIC_REPRESENTATION_ITEM ( )  RATIONAL_B_SPLINE_SURFACE ( (
 ( 1.000000000000000000, 1.000000000000000000),
 ( 0.7789835883360578528, 0.9689951854195403280),
 ( 0.7789835883360578528, 0.9689951854195403280),
 ( 1.000000000000000000, 1.000000000000000000) ) ) 
 REPRESENTATION_ITEM ( '' )  SURFACE ( )  );
#24472 = CARTESIAN_POINT ( 'NONE',  ( 6.224689322667630975, 89.08920297664369059, -118.2566963816762211 ) ) ;
#24473 = VERTEX_POINT ( 'NONE', #13283 ) ;
#24474 = CARTESIAN_POINT ( 'NONE',  ( 1.834118845439484335, 72.40084790867331321, 125.7578880615047439 ) ) ;
#24475 = CARTESIAN_POINT ( 'NONE',  ( -20.47566338032518019, 29.82700953060488303, -1.586617869343990739 ) ) ;
#24476 = CARTESIAN_POINT ( 'NONE',  ( -55.24198130335446422, 0.001391250620101877958, 0.009190321388310107587 ) ) ;
#24477 = VERTEX_POINT ( 'NONE', #25608 ) ;
#24479 =( BOUNDED_SURFACE ( )  B_SPLINE_SURFACE ( 3, 1, ( 
 ( #24119, #6841 ),
 ( #4382, #65 ),
 ( #19771, #22081 ),
 ( #13156, #11152 ) ),
 .UNSPECIFIED., .F., .F., .F. ) 
 B_SPLINE_SURFACE_WITH_KNOTS ( ( 4, 4 ),
 ( 2, 2 ),
 ( 0.000000000000000000, 1.000000000000000000 ),
 ( 0.000000000000000000, 1.000000000000000000 ),
 .UNSPECIFIED. ) 
 GEOMETRIC_REPRESENTATION_ITEM ( )  RATIONAL_B_SPLINE_SURFACE ( (
 ( 1.000000000000000000, 1.000000000000000000),
 ( 0.9960225298536222738, 0.9999952330161893110),
 ( 0.9960225298536222738, 0.9999952330161893110),
 ( 1.000000000000000000, 1.000000000000000000) ) ) 
 REPRESENTATION_ITEM ( '' )  SURFACE ( )  );
#24478 = AXIS2_PLACEMENT_3D ( 'NONE', #10343, #9908, #23011 ) ;
#24480 = ORIENTED_EDGE ( 'NONE', *, *, #10128, .T. ) ;
#24481 = ORIENTED_EDGE ( 'NONE', *, *, #5525, .T. ) ;
#24482 = VECTOR ( 'NONE', #16849, 1000.000000000000000 ) ;
#24483 = CARTESIAN_POINT ( 'NONE',  ( 109.1721716018069657, 0.01281875973824526428, 0.01127028715940106736 ) ) ;
#24484 = DIRECTION ( 'NONE',  ( 0.000000000000000000, 0.000000000000000000, 1.000000000000000000 ) ) ;
#24485 = EDGE_CURVE ( 'NONE', #15158, #16092, #22217, .T. ) ;
#24486 = FACE_OUTER_BOUND ( 'NONE', #2682, .T. ) ;
#24487 = EDGE_CURVE ( 'NONE', #24434, #7787, #16249, .T. ) ;
#24488 = CARTESIAN_POINT ( 'NONE',  ( 2.433796855181205476, 28.83182736670536528, 142.6247129145649239 ) ) ;
#24489 = ORIENTED_EDGE ( 'NONE', *, *, #10163, .T. ) ;
#24490 = CARTESIAN_POINT ( 'NONE',  ( -55.24340739397742084, 0.0007387096945740994529, -0.01010924026184336841 ) ) ;
#24491 = CARTESIAN_POINT ( 'NONE',  ( -1.046935749539985583, -1.275486069320154847, 45.77872888003168583 ) ) ;
#24492 = ORIENTED_EDGE ( 'NONE', *, *, #10168, .T. ) ;
#24493 = CARTESIAN_POINT ( 'NONE',  ( 25.81918753295377300, 91.98563552013041544, 65.67738364544763385 ) ) ;
#24494 = ORIENTED_EDGE ( 'NONE', *, *, #8507, .T. ) ;
#24495 = CARTESIAN_POINT ( 'NONE',  ( 1.833838850855486147, 141.9572669680999013, -30.08297881069537993 ) ) ;
#24496 = CARTESIAN_POINT ( 'NONE',  ( 25.64692232868535626, -46.22343382108668663, -103.0161468101951954 ) ) ;
#24497 = CARTESIAN_POINT ( 'NONE',  ( -5.986830583229489022, -4.559539818181495896, -50.53158596890440180 ) ) ;
#24498 = CARTESIAN_POINT ( 'NONE',  ( -20.37983603106073716, 27.81368274044725553, 10.62371319148611981 ) ) ;
#24499 = FACE_OUTER_BOUND ( 'NONE', #8863, .T. ) ;
#24500 = CARTESIAN_POINT ( 'NONE',  ( 55.49584447822657296, 68.91748907713619587, -22.67407039687169501 ) ) ;
#24501 = CARTESIAN_POINT ( 'NONE',  ( 1.833485406944043827, 58.53321471326877656, 132.7804117027889674 ) ) ;
#24502 = CARTESIAN_POINT ( 'NONE',  ( -55.25297051322618813, -0.01093108995495129139, -0.01019003092403723831 ) ) ;
#24503 = VECTOR ( 'NONE', #7848, 999.9999999999998863 ) ;
#24504 = CARTESIAN_POINT ( 'NONE',  ( -23.77929240705206837, -32.66578242509734054, 15.74261278740706338 ) ) ;
#24505 = DIRECTION ( 'NONE',  ( 0.000000000000000000, 5.223019709708233256E-21, -1.000000000000000000 ) ) ;
#24506 = CARTESIAN_POINT ( 'NONE',  ( -25.21435515916043002, 31.17620025257588523, -15.02493970636157705 ) ) ;
#24507 = CARTESIAN_POINT ( 'NONE',  ( -25.21435515916043713, 4.655591116594827383, 34.29329011225949841 ) ) ;
#24508 = ORIENTED_EDGE ( 'NONE', *, *, #23183, .F. ) ;
#24509 = ORIENTED_EDGE ( 'NONE', *, *, #24288, .T. ) ;
#24510 = CARTESIAN_POINT ( 'NONE',  ( -20.21097721712958517, -9.464413111084555297, 28.05863618200118381 ) ) ;
#24511 = CARTESIAN_POINT ( 'NONE',  ( 25.69398547355841700, 107.1830796521259259, -35.60637981494741666 ) ) ;
#24512 = VERTEX_POINT ( 'NONE', #12621 ) ;
#24513 = ORIENTED_EDGE ( 'NONE', *, *, #15097, .F. ) ;
#24514 = AXIS2_PLACEMENT_3D ( 'NONE', #8059, #4227, #21121 ) ;
#24515 = ORIENTED_EDGE ( 'NONE', *, *, #74, .T. ) ;
#24516 =( BOUNDED_SURFACE ( )  B_SPLINE_SURFACE ( 3, 1, ( 
 ( #4295, #28452 ),
 ( #6749, #8617 ),
 ( #2116, #1841 ),
 ( #4567, #13339 ) ),
 .UNSPECIFIED., .F., .F., .F. ) 
 B_SPLINE_SURFACE_WITH_KNOTS ( ( 4, 4 ),
 ( 2, 2 ),
 ( 0.000000000000000000, 1.000000000000000000 ),
 ( 0.000000000000000000, 1.000000000000000000 ),
 .UNSPECIFIED. ) 
 GEOMETRIC_REPRESENTATION_ITEM ( )  RATIONAL_B_SPLINE_SURFACE ( (
 ( 1.000000000000000000, 1.000000000000000000),
 ( 0.9956975270656954757, 0.8568959468854893125),
 ( 0.9956975270656954757, 0.8568959468854893125),
 ( 1.000000000000000000, 1.000000000000000000) ) ) 
 REPRESENTATION_ITEM ( '' )  SURFACE ( )  );
#24517 = CARTESIAN_POINT ( 'NONE',  ( -1.045287976400365970, 45.76855895860943235, -1.530335034934267258 ) ) ;
#24518 = CARTESIAN_POINT ( 'NONE',  ( 6.224689322667630975, -33.28770499679432504, 144.2687111683194416 ) ) ;
#24519 = ADVANCED_FACE ( 'NONE', ( #22070 ), #4757, .T. ) ;
#24520 = ADVANCED_FACE ( 'NONE', ( #28019 ), #22143, .F. ) ;
#24521 = B_SPLINE_CURVE_WITH_KNOTS ( 'NONE', 3,
 ( #11278, #21796, #20046, #1917 ),
 .UNSPECIFIED., .F., .F.,
 ( 4, 4 ),
 ( 0.000000000000000000, 0.008383560773332731156 ),
 .UNSPECIFIED. ) ;
#24522 = AXIS2_PLACEMENT_3D ( 'NONE', #20532, #7310, #25448 ) ;
#24523 = FACE_OUTER_BOUND ( 'NONE', #24873, .T. ) ;
#24524 = CARTESIAN_POINT ( 'NONE',  ( 1.833721034905622549, 138.1171912769431174, 44.50273803001984874 ) ) ;
#24525 = VECTOR ( 'NONE', #15502, 1000.000000000000114 ) ;
#24526 = ORIENTED_EDGE ( 'NONE', *, *, #6043, .F. ) ;
#24527 = EDGE_CURVE ( 'NONE', #9673, #25484, #23256, .T. ) ;
#24528 = CARTESIAN_POINT ( 'NONE',  ( -55.24300891470648622, 0.006048736206180948920, -0.007734635432132875611 ) ) ;
#24529 = CARTESIAN_POINT ( 'NONE',  ( 109.1587776205901577, 0.006944419901758093830, 0.002343968083389380997 ) ) ;
#24530 = EDGE_CURVE ( 'NONE', #23418, #11824, #25659, .T. ) ;
#24531 = FACE_OUTER_BOUND ( 'NONE', #23983, .T. ) ;
#24532 = CARTESIAN_POINT ( 'NONE',  ( 25.64700659047694131, 66.18331466615558156, 91.48068002582046176 ) ) ;
#24533 = CARTESIAN_POINT ( 'NONE',  ( 24.01988960052067767, 4.273195451970473790, -130.9749633972836023 ) ) ;
#24534 = CARTESIAN_POINT ( 'NONE',  ( 109.1589550718174877, 0.003591809816104994842, 0.006669585340466659650 ) ) ;
#24535 = CARTESIAN_POINT ( 'NONE',  ( -1.619063947482201282, 11.94059994246159384, -44.80407745103787676 ) ) ;
#24537 = CIRCLE ( 'NONE', #3375, 117.6351876552689504 ) ;
#24536 = CARTESIAN_POINT ( 'NONE',  ( 2.063896406836605024, -98.19887492195931600, 107.0521644432414092 ) ) ;
#24538 = CARTESIAN_POINT ( 'NONE',  ( -55.24340739397742794, -0.009842732675348539115, -0.002421372372456522849 ) ) ;
#24539 = VERTEX_POINT ( 'NONE', #9120 ) ;
#24541 = CARTESIAN_POINT ( 'NONE',  ( 25.64692232868534560, -66.63160215461202540, -91.15460455808893414 ) ) ;
#24540 = CARTESIAN_POINT ( 'NONE',  ( 25.64703792032470275, 91.43447020678432580, 66.24710921678085640 ) ) ;
#24542 = CARTESIAN_POINT ( 'NONE',  ( 109.1721716018069515, -0.01019541462303045869, 0.01368917435590585353 ) ) ;
#24543 = CARTESIAN_POINT ( 'NONE',  ( -1.046935749539994465, -37.78548154587976882, 25.87617179820957602 ) ) ;
#24544 = CARTESIAN_POINT ( 'NONE',  ( -20.20700224038492721, 29.58392382092673500, 0.9908225410479544193 ) ) ;
#24545 = CARTESIAN_POINT ( 'NONE',  ( -8.259864102781671491, -36.24929574824938783, -38.68084189741935575 ) ) ;
#24546 = ORIENTED_EDGE ( 'NONE', *, *, #11221, .T. ) ;
#24547 = CARTESIAN_POINT ( 'NONE',  ( 26.11404676487257603, -47.08215554553588333, 102.9690087468800073 ) ) ;
#24548 = AXIS2_PLACEMENT_3D ( 'NONE', #5025, #9214, #574 ) ;
#24549 = ORIENTED_EDGE ( 'NONE', *, *, #20807, .F. ) ;
#24550 = CARTESIAN_POINT ( 'NONE',  ( 10.93730112725972781, -56.95489579269845137, 140.0398180619108359 ) ) ;
#24551 = CARTESIAN_POINT ( 'NONE',  ( -20.38016308990357217, -23.16952666206571365, 18.69911008768360361 ) ) ;
#24552 = EDGE_LOOP ( 'NONE', ( #17216, #16270, #814, #14929 ) ) ;
#24553 = VECTOR ( 'NONE', #11813, 1000.000000000000114 ) ;
#24554 = ORIENTED_EDGE ( 'NONE', *, *, #18959, .F. ) ;
#24555 = DIRECTION ( 'NONE',  ( 0.7637818620346800147, 0.5092696688508698832, 0.3965875333584785167 ) ) ;
#24556 = ORIENTED_EDGE ( 'NONE', *, *, #11967, .F. ) ;
#24557 = CARTESIAN_POINT ( 'NONE',  ( 1.833838850855450398, -97.03125735562164778, -107.8971100408360684 ) ) ;
#24558 = VERTEX_POINT ( 'NONE', #2782 ) ;
#24559 = B_SPLINE_CURVE_WITH_KNOTS ( 'NONE', 3,
 ( #4400, #22259, #19793, #20080, #87, #26696 ),
 .UNSPECIFIED., .F., .F.,
 ( 4, 2, 4 ),
 ( 0.000000000000000000, 0.003570751334075647834, 0.007141502668151295669 ),
 .UNSPECIFIED. ) ;
#24560 = ADVANCED_FACE ( 'NONE', ( #16164 ), #17877, .T. ) ;
#24561 = CARTESIAN_POINT ( 'NONE',  ( -55.24390624410018802, -0.009209468562452135382, -0.004896917417131697002 ) ) ;
#24562 = VECTOR ( 'NONE', #25217, 1000.000000000000000 ) ;
#24563 = EDGE_CURVE ( 'NONE', #24705, #22495, #11921, .T. ) ;
#24564 = CARTESIAN_POINT ( 'NONE',  ( -25.21435515916043357, -16.39063784838764093, -30.48034229288631991 ) ) ;
#24565 =( BOUNDED_SURFACE ( )  B_SPLINE_SURFACE ( 3, 1, ( 
 ( #2941, #22233 ),
 ( #772, #13719 ),
 ( #27093, #19923 ),
 ( #15442, #4510 ) ),
 .UNSPECIFIED., .F., .F., .F. ) 
 B_SPLINE_SURFACE_WITH_KNOTS ( ( 4, 4 ),
 ( 2, 2 ),
 ( 0.000000000000000000, 1.000000000000000000 ),
 ( 0.000000000000000000, 1.000000000000000000 ),
 .UNSPECIFIED. ) 
 GEOMETRIC_REPRESENTATION_ITEM ( )  RATIONAL_B_SPLINE_SURFACE ( (
 ( 1.000000000000000000, 1.000000000000000000),
 ( 0.9956975270656955868, 0.8568959468854907557),
 ( 0.9956975270656955868, 0.8568959468854907557),
 ( 1.000000000000000000, 1.000000000000000000) ) ) 
 REPRESENTATION_ITEM ( '' )  SURFACE ( )  );
#24566 = FACE_OUTER_BOUND ( 'NONE', #24012, .T. ) ;
#24567 = CARTESIAN_POINT ( 'NONE',  ( -6.574463467970658392, 50.12924290857549181, 11.01561683919999091 ) ) ;
#24568 = CARTESIAN_POINT ( 'NONE',  ( 1.833750490713712766, -72.32354185792470957, -125.8019536335927597 ) ) ;
#24569 = DIRECTION ( 'NONE',  ( 0.000000000000000000, -5.223019709708116647E-21, 1.000000000000000000 ) ) ;
#24570 = CARTESIAN_POINT ( 'NONE',  ( -55.24390624410018802, 0.01032895241566708991, 0.001451500391952845713 ) ) ;
#24571 = CARTESIAN_POINT ( 'NONE',  ( -23.79223135445719706, -24.83942264280416978, -22.01133905265676916 ) ) ;
#24572 = CARTESIAN_POINT ( 'NONE',  ( 25.70243777736189728, -0.7331659071603116029, 112.9457924277214005 ) ) ;
#24573 = CARTESIAN_POINT ( 'NONE',  ( 32.73300124599769134, -51.32617430724849328, -105.8473486001054198 ) ) ;
#24575 = ORIENTED_EDGE ( 'NONE', *, *, #653, .T. ) ;
#24574 = B_SPLINE_CURVE_WITH_KNOTS ( 'NONE', 3,
 ( #7624, #16823, #23021, #18683, #18544, #1545 ),
 .UNSPECIFIED., .F., .F.,
 ( 4, 2, 4 ),
 ( 1.734723475976807094E-18, 0.0004335184443140216969, 0.0008670368886280416590 ),
 .UNSPECIFIED. ) ;
#24576 = CARTESIAN_POINT ( 'NONE',  ( -2.904412668506660467, 11.97478724945576545, 46.12477647685262383 ) ) ;
#24577 = CARTESIAN_POINT ( 'NONE',  ( -1.049819825607597235, -26.50610175068240792, 37.34982882986871999 ) ) ;
#24578 = CARTESIAN_POINT ( 'NONE',  ( -22.23226125620943705, -20.31044300692189708, -24.24619897613468211 ) ) ;
#24579 = CARTESIAN_POINT ( 'NONE',  ( 1.833721036429677875, -0.3559391723973897581, -145.1093571290645627 ) ) ;
#24580 = CARTESIAN_POINT ( 'NONE',  ( 1.833838848569415036, 45.01064392477934462, 137.9525894882059447 ) ) ;
#24581 = CARTESIAN_POINT ( 'NONE',  ( -1.539763995773691940, 46.22267697748604576, 2.469814354917652999 ) ) ;
#24582 = CARTESIAN_POINT ( 'NONE',  ( -1.044557008772710516, -37.98985164565307571, 25.56990300677022177 ) ) ;
#24583 = ORIENTED_EDGE ( 'NONE', *, *, #13795, .T. ) ;
#24584 = CARTESIAN_POINT ( 'NONE',  ( 2.063896406836605024, -118.3103904147687331, 84.29612368209116369 ) ) ;
#24585 = ORIENTED_EDGE ( 'NONE', *, *, #18448, .F. ) ;
#24586 = CARTESIAN_POINT ( 'NONE',  ( 25.86096068574581253, -112.5344699600049978, 10.82483750674566814 ) ) ;
#24587 = B_SPLINE_CURVE_WITH_KNOTS ( 'NONE', 3,
 ( #13140, #6684, #17872, #20184, #46, #4935, #2482 ),
 .UNSPECIFIED., .F., .F.,
 ( 4, 3, 4 ),
 ( 6.445168920560267517E-16, 0.02816610861753245099, 0.04000277880656284701 ),
 .UNSPECIFIED. ) ;
#24588 = CARTESIAN_POINT ( 'NONE',  ( -20.24419206586953734, -28.55732805495821225, -7.929973069813295972 ) ) ;
#24589 = CARTESIAN_POINT ( 'NONE',  ( -1.045287976400365970, -36.12803364096568259, 28.14015102489869591 ) ) ;
#24590 = EDGE_CURVE ( 'NONE', #20894, #25218, #11561, .T. ) ;
#24591 = ORIENTED_EDGE ( 'NONE', *, *, #24384, .F. ) ;
#24592 = CARTESIAN_POINT ( 'NONE',  ( 25.87036335909425944, 112.3329723497412118, -12.80197335559845584 ) ) ;
#24593 = ORIENTED_EDGE ( 'NONE', *, *, #28376, .F. ) ;
#24594 = EDGE_CURVE ( 'NONE', #2946, #7265, #24637, .T. ) ;
#24595 = CARTESIAN_POINT ( 'NONE',  ( 109.1592201516379674, 0.007845213074660002325, 0.0005146241775907644525 ) ) ;
#24596 = ORIENTED_EDGE ( 'NONE', *, *, #18898, .F. ) ;
#24597 = EDGE_CURVE ( 'NONE', #675, #7808, #9417, .T. ) ;
#24598 = DIRECTION ( 'NONE',  ( 0.000000000000000000, 0.000000000000000000, 1.000000000000000000 ) ) ;
#24599 = CARTESIAN_POINT ( 'NONE',  ( -20.57838717382308147, -18.89542499756482741, 23.26537097894125594 ) ) ;
#24600 =( BOUNDED_SURFACE ( )  B_SPLINE_SURFACE ( 3, 1, ( 
 ( #5160, #273 ),
 ( #17959, #18390 ),
 ( #13509, #20418 ),
 ( #13357, #9061 ) ),
 .UNSPECIFIED., .F., .F., .F. ) 
 B_SPLINE_SURFACE_WITH_KNOTS ( ( 4, 4 ),
 ( 2, 2 ),
 ( 0.000000000000000000, 1.000000000000000000 ),
 ( 0.000000000000000000, 1.000000000000000000 ),
 .UNSPECIFIED. ) 
 GEOMETRIC_REPRESENTATION_ITEM ( )  RATIONAL_B_SPLINE_SURFACE ( (
 ( 1.000000000000000000, 1.000000000000000000),
 ( 0.6386103224230302855, 0.9954351624131538845),
 ( 0.6386103224230302855, 0.9954351624131538845),
 ( 1.000000000000000000, 1.000000000000000000) ) ) 
 REPRESENTATION_ITEM ( '' )  SURFACE ( )  );
#24601 = CARTESIAN_POINT ( 'NONE',  ( 109.1586900883932856, -0.004851151255031890298, 0.005236795036868143773 ) ) ;
#24602 = LINE ( 'NONE', #27406, #14945 ) ;
#24603 = CARTESIAN_POINT ( 'NONE',  ( -25.21435515916043713, 6.169479169075932745, 34.05351380035326514 ) ) ;
#24604 = CARTESIAN_POINT ( 'NONE',  ( 1.833485406944043827, -125.9346397303440455, 72.09189602597663793 ) ) ;
#24605 = EDGE_LOOP ( 'NONE', ( #15735, #7460, #11362, #4725 ) ) ;
#24606 = CARTESIAN_POINT ( 'NONE',  ( 6.224689322667647851, 147.4941644018828129, 12.92299475787008234 ) ) ;
#24607 = CARTESIAN_POINT ( 'NONE',  ( -55.24271866751342941, 0.006671293903669565407, -0.006757859501006440936 ) ) ;
#24608 = DIRECTION ( 'NONE',  ( 0.000000000000000000, 0.000000000000000000, 1.000000000000000000 ) ) ;
#24609 = ORIENTED_EDGE ( 'NONE', *, *, #12313, .F. ) ;
#24610 = ORIENTED_EDGE ( 'NONE', *, *, #18734, .F. ) ;
#24611 = VERTEX_POINT ( 'NONE', #7260 ) ;
#24612 = FACE_OUTER_BOUND ( 'NONE', #27345, .T. ) ;
#24613 = CARTESIAN_POINT ( 'NONE',  ( -55.24271866751342941, -0.008433070970613520956, 0.004365563123935277227 ) ) ;
#24614 = CARTESIAN_POINT ( 'NONE',  ( 25.70243777736190438, -24.19989514742795933, 110.3252221127464736 ) ) ;
#24615 = CARTESIAN_POINT ( 'NONE',  ( -1.056502255334265339, 37.35734037467636171, -26.51074901220517432 ) ) ;
#24616 = CARTESIAN_POINT ( 'NONE',  ( -20.90916690077944295, 39.20864005633548999, -5.322316104228152156 ) ) ;
#24617 = CARTESIAN_POINT ( 'NONE',  ( 32.73300124599732186, 0.000000000000000000, 0.000000000000000000 ) ) ;
#24618 = ADVANCED_FACE ( 'NONE', ( #16016 ), #17174, .F. ) ;
#24619 = CARTESIAN_POINT ( 'NONE',  ( -20.20612091757423912, 1.137293889216362874, -29.57813639663777039 ) ) ;
#24620 = ORIENTED_EDGE ( 'NONE', *, *, #219, .T. ) ;
#24621 = CARTESIAN_POINT ( 'NONE',  ( 2.063896406836609909, -142.3682421260905642, -28.88716984836465684 ) ) ;
#24622 = CARTESIAN_POINT ( 'NONE',  ( -6.574463467970653952, -11.01561683920017387, 50.12924290857549181 ) ) ;
#24623 = CARTESIAN_POINT ( 'NONE',  ( 1.833838850093440387, -145.1097630783161492, 3.453305159929904334E-06 ) ) ;
#24624 = FACE_OUTER_BOUND ( 'NONE', #5482, .T. ) ;
#24625 = CARTESIAN_POINT ( 'NONE',  ( 9.884929003653608603, 78.87917189085089831, -128.2151425008033243 ) ) ;
#24626 = VERTEX_POINT ( 'NONE', #9693 ) ;
#24627 = CARTESIAN_POINT ( 'NONE',  ( -5.986830583229505898, 43.56094206392996426, 26.01297580803277754 ) ) ;
#24628 = EDGE_CURVE ( 'NONE', #4100, #23015, #7124, .T. ) ;
#24629 = B_SPLINE_CURVE_WITH_KNOTS ( 'NONE', 3,
 ( #4542, #22261, #13604, #11449, #18066, #5114, #24276 ),
 .UNSPECIFIED., .F., .F.,
 ( 4, 3, 4 ),
 ( 5.872724359755720846E-16, 0.02816610861753247527, 0.04000277880656283314 ),
 .UNSPECIFIED. ) ;
#24630 = ORIENTED_EDGE ( 'NONE', *, *, #10070, .F. ) ;
#24631 = CARTESIAN_POINT ( 'NONE',  ( 2.433796855181205476, 142.6247129145651797, -28.83182736670396196 ) ) ;
#24632 = CARTESIAN_POINT ( 'NONE',  ( -55.24271866751342941, -0.001545935011630300039, 0.009369360294295641864 ) ) ;
#24633 = VERTEX_POINT ( 'NONE', #18469 ) ;
#24634 = EDGE_CURVE ( 'NONE', #14882, #2900, #26989, .T. ) ;
#24635 = ORIENTED_EDGE ( 'NONE', *, *, #7530, .F. ) ;
#24636 = ORIENTED_EDGE ( 'NONE', *, *, #27190, .F. ) ;
#24637 = B_SPLINE_CURVE_WITH_KNOTS ( 'NONE', 3,
 ( #13425, #22225, #13712, #330, #22374, #2637, #5226, #11418, #3077, #11851 ),
 .UNSPECIFIED., .F., .F.,
 ( 4, 3, 3, 4 ),
 ( 1.387778780781445676E-17, 0.0002669560319015815792, 0.0005492286108966455737, 0.0008315040496093443556 ),
 .UNSPECIFIED. ) ;
#24638 = CARTESIAN_POINT ( 'NONE',  ( 10.93730112725972425, -42.00474393596362432, 145.2260730187398678 ) ) ;
#24639 = CARTESIAN_POINT ( 'NONE',  ( 109.1624594426973118, -0.01358749486988776456, 0.008380433676413060612 ) ) ;
#24640 = CARTESIAN_POINT ( 'NONE',  ( -23.79248802219722592, -32.40806545715335574, -7.157555990716774730 ) ) ;
#24641 = CARTESIAN_POINT ( 'NONE',  ( 2.063896406836609909, -108.8509294491458661, -96.20114399516505443 ) ) ;
#24642 = CARTESIAN_POINT ( 'NONE',  ( 119.2224693531408803, 70.00000000000002842, 19.99999999999997513 ) ) ;
#24643 = EDGE_LOOP ( 'NONE', ( #5312, #19304, #26254, #8130 ) ) ;
#24644 = CARTESIAN_POINT ( 'NONE',  ( -1.019300379054419725, 28.53917295602949977, 35.83762006677368106 ) ) ;
#24645 = CARTESIAN_POINT ( 'NONE',  ( 25.64660436782558151, 45.39454672041254923, -103.3839381879726886 ) ) ;
#24646 = CARTESIAN_POINT ( 'NONE',  ( 109.1589550718174877, -0.006257602293694239197, 0.004269295012386535582 ) ) ;
#24647 = ORIENTED_EDGE ( 'NONE', *, *, #27619, .T. ) ;
#24648 = CARTESIAN_POINT ( 'NONE',  ( -22.23342874802667879, 31.55488258420089664, 2.180636882146622657 ) ) ;
#24649 = EDGE_LOOP ( 'NONE', ( #7971, #17076, #2752, #17506 ) ) ;
#24650 = CARTESIAN_POINT ( 'NONE',  ( -20.57838717382308147, 28.96176188950229502, 7.715628353033378239 ) ) ;
#24651 = CARTESIAN_POINT ( 'NONE',  ( -25.21435515916043713, 34.05351380035342146, 6.169479169075106739 ) ) ;
#24652 = CARTESIAN_POINT ( 'NONE',  ( -12.94347594948480484, 43.91326021875542551, 21.16159467081307710 ) ) ;
#24653 = CARTESIAN_POINT ( 'NONE',  ( -1.050231094221219408, 14.39477892760360689, 43.47885872350340009 ) ) ;
#24654 = EDGE_CURVE ( 'NONE', #3225, #13021, #15782, .T. ) ;
#24655 = CARTESIAN_POINT ( 'NONE',  ( 1.833691583653523693, 58.69608658929927714, 132.7086741139084722 ) ) ;
#24656 = CARTESIAN_POINT ( 'NONE',  ( -20.20612092514784308, -8.058517256680906016, 28.48192215759674184 ) ) ;
#24657 = B_SPLINE_CURVE_WITH_KNOTS ( 'NONE', 3,
 ( #12662, #21731, #28060, #1589, #26050, #4163, #6477 ),
 .UNSPECIFIED., .F., .F.,
 ( 4, 3, 4 ),
 ( 6.397367602755259510E-16, 0.02816610861753244405, 0.04000277880656278456 ),
 .UNSPECIFIED. ) ;
#24658 = CARTESIAN_POINT ( 'NONE',  ( -20.37983603106074071, 16.25728007463443703, 24.94323704205420000 ) ) ;
#24659 = CARTESIAN_POINT ( 'NONE',  ( 109.1586900883932856, -0.006130969560693689396, -0.003656351050324864460 ) ) ;
#24660 = CARTESIAN_POINT ( 'NONE',  ( -22.34422965417127216, -5.100074259622869199, -37.57019010019544680 ) ) ;
#24661 =( BOUNDED_SURFACE ( )  B_SPLINE_SURFACE ( 3, 1, ( 
 ( #23449, #10068 ),
 ( #12216, #25478 ),
 ( #5600, #21123 ),
 ( #23182, #27760 ) ),
 .UNSPECIFIED., .F., .F., .F. ) 
 B_SPLINE_SURFACE_WITH_KNOTS ( ( 4, 4 ),
 ( 2, 2 ),
 ( 0.000000000000000000, 1.000000000000000000 ),
 ( 0.000000000000000000, 1.000000000000000000 ),
 .UNSPECIFIED. ) 
 GEOMETRIC_REPRESENTATION_ITEM ( )  RATIONAL_B_SPLINE_SURFACE ( (
 ( 1.000000000000000000, 1.000000000000000000),
 ( 0.6386103224230316178, 0.9954351624131538845),
 ( 0.6386103224230316178, 0.9954351624131538845),
 ( 1.000000000000000000, 1.000000000000000000) ) ) 
 REPRESENTATION_ITEM ( '' )  SURFACE ( )  );
#24662 = FACE_OUTER_BOUND ( 'NONE', #13421, .T. ) ;
#24663 = EDGE_CURVE ( 'NONE', #17576, #19356, #19805, .T. ) ;
#24664 = EDGE_CURVE ( 'NONE', #24250, #19237, #1258, .T. ) ;
#24665 = ORIENTED_EDGE ( 'NONE', *, *, #13679, .F. ) ;
#24666 = CARTESIAN_POINT ( 'NONE',  ( -1.155031165708884533, 44.25214473648929925, 12.20332162035416879 ) ) ;
#24667 = CARTESIAN_POINT ( 'NONE',  ( 26.11404676487259024, 107.3263591096435476, -36.06104232266339693 ) ) ;
#24668 = EDGE_LOOP ( 'NONE', ( #19909, #4994, #18827, #28389 ) ) ;
#24669 = EDGE_CURVE ( 'NONE', #6550, #15305, #18615, .T. ) ;
#24670 = VERTEX_POINT ( 'NONE', #22956 ) ;
#24671 = ORIENTED_EDGE ( 'NONE', *, *, #8647, .T. ) ;
#24672 = CARTESIAN_POINT ( 'NONE',  ( 26.11404676487257603, -98.61392875273402581, 55.62948129436210110 ) ) ;
#24673 = CARTESIAN_POINT ( 'NONE',  ( -20.57838717382308147, 29.92853265176831812, -1.611677988432464126 ) ) ;
#24674 = CARTESIAN_POINT ( 'NONE',  ( 2.430230287190589422, 125.2872625092172569, -74.01081053030968349 ) ) ;
#24675 = CARTESIAN_POINT ( 'NONE',  ( 25.64681081121879203, -103.3177883989782657, 45.54494737132187510 ) ) ;
#24676 = CARTESIAN_POINT ( 'NONE',  ( -1.583189561560256253, 46.33203782964461936, -2.490696082060027017 ) ) ;
#24677 = CARTESIAN_POINT ( 'NONE',  ( 109.1592201516379674, 0.006649399203953390916, 0.004194960840980714069 ) ) ;
#24678 = CARTESIAN_POINT ( 'NONE',  ( 109.1589550718175161, 0.005994046294305907172, -0.004632048724982925844 ) ) ;
#24679 = CARTESIAN_POINT ( 'NONE',  ( 25.64708010899961721, 66.41183455464135932, 91.31497827399759615 ) ) ;
#24680 = CARTESIAN_POINT ( 'NONE',  ( 8.186469777910854617, -134.9918587298867863, 63.89871389959409242 ) ) ;
#24681 = CARTESIAN_POINT ( 'NONE',  ( 109.1592201516379674, 0.002913740842108636896, 0.007302213399779935825 ) ) ;
#24682 = CARTESIAN_POINT ( 'NONE',  ( -28.13707043255157103, -12.83104814250440029, 18.96624908365860662 ) ) ;
#24683 = CARTESIAN_POINT ( 'NONE',  ( -2.904412668506655582, -44.35433137608953302, -17.42365698954681719 ) ) ;
#24684 = DIRECTION ( 'NONE',  ( -1.000000000000000000, -0.000000000000000000, -0.000000000000000000 ) ) ;
#24685 = CARTESIAN_POINT ( 'NONE',  ( -20.47566262905010248, -23.19796652405687709, -18.81547655725238499 ) ) ;
#24686 = ADVANCED_FACE ( 'NONE', ( #7840 ), #13300, .F. ) ;
#24687 = ORIENTED_EDGE ( 'NONE', *, *, #19717, .T. ) ;
#24688 = DIRECTION ( 'NONE',  ( 0.7637818620346800147, -0.3965875333584803486, 0.5092696688508683289 ) ) ;
#24689 = CARTESIAN_POINT ( 'NONE',  ( 1.833603222531972277, -144.2675221341993108, -15.61050054119179187 ) ) ;
#24690 = DIRECTION ( 'NONE',  ( -0.5946245182733608248, -0.4749651461092209148, -0.6487139525627763081 ) ) ;
#24691 = CARTESIAN_POINT ( 'NONE',  ( 6.224689322667647851, -97.14981701196397523, 111.7293398381261653 ) ) ;
#24692 = CARTESIAN_POINT ( 'NONE',  ( -4.780792508754325709, -11.68149851467495637, -48.13366140756553335 ) ) ;
#24693 = VERTEX_POINT ( 'NONE', #12408 ) ;
#24694 = CARTESIAN_POINT ( 'NONE',  ( 16.05277956358212066, 34.34928806929423217, 139.1285124304119165 ) ) ;
#24695 =( BOUNDED_SURFACE ( )  B_SPLINE_SURFACE ( 3, 1, ( 
 ( #2663, #11736 ),
 ( #26692, #22102 ),
 ( #11169, #4535 ),
 ( #15760, #7004 ) ),
 .UNSPECIFIED., .F., .F., .F. ) 
 B_SPLINE_SURFACE_WITH_KNOTS ( ( 4, 4 ),
 ( 2, 2 ),
 ( 0.000000000000000000, 1.000000000000000000 ),
 ( 0.000000000000000000, 1.000000000000000000 ),
 .UNSPECIFIED. ) 
 GEOMETRIC_REPRESENTATION_ITEM ( )  RATIONAL_B_SPLINE_SURFACE ( (
 ( 1.000000000000000000, 1.000000000000000000),
 ( 0.6386103224230316178, 0.9954351624131538845),
 ( 0.6386103224230316178, 0.9954351624131538845),
 ( 1.000000000000000000, 1.000000000000000000) ) ) 
 REPRESENTATION_ITEM ( '' )  SURFACE ( )  );
#24696 = EDGE_CURVE ( 'NONE', #18134, #22961, #27366, .T. ) ;
#24697 = ORIENTED_EDGE ( 'NONE', *, *, #14566, .F. ) ;
#24698 = DIRECTION ( 'NONE',  ( 0.000000000000000000, 5.223019709708233256E-21, -1.000000000000000000 ) ) ;
#24699 = CARTESIAN_POINT ( 'NONE',  ( 55.79472521941428198, -30.25520714117862653, -66.16469064668328315 ) ) ;
#24700 = ORIENTED_EDGE ( 'NONE', *, *, #27657, .F. ) ;
#24701 = CARTESIAN_POINT ( 'NONE',  ( -10.86508079875780552, -6.877801422380434460, 50.67624451685642839 ) ) ;
#24702 = EDGE_CURVE ( 'NONE', #3658, #23165, #18076, .T. ) ;
#24703 = ORIENTED_EDGE ( 'NONE', *, *, #2413, .T. ) ;
#24704 = CARTESIAN_POINT ( 'NONE',  ( 1.833691583653538348, -96.83253123394135287, -108.0753610255262913 ) ) ;
#24705 = VERTEX_POINT ( 'NONE', #7651 ) ;
#24706 = B_SPLINE_CURVE_WITH_KNOTS ( 'NONE', 3,
 ( #17330, #21658, #19502, #2205, #26119, #12356 ),
 .UNSPECIFIED., .F., .F.,
 ( 4, 2, 4 ),
 ( 4.114075111014854645E-16, 0.003576372551511222079, 0.007152745103022032161 ),
 .UNSPECIFIED. ) ;
#24707 = ORIENTED_EDGE ( 'NONE', *, *, #8363, .T. ) ;
#24708 = CARTESIAN_POINT ( 'NONE',  ( -8.786685647604885574, 6.096987947571466530E-17, -1.524246986892866633E-17 ) ) ;
#24709 = FACE_OUTER_BOUND ( 'NONE', #13078, .T. ) ;
#24710 = CARTESIAN_POINT ( 'NONE',  ( -55.24271866751342941, -0.008488649505345847654, 0.004256484107793125603 ) ) ;
#24711 = CARTESIAN_POINT ( 'NONE',  ( -8.786685647604889127, 9.545808661480615243, -52.67761315067287597 ) ) ;
#24712 = CARTESIAN_POINT ( 'NONE',  ( 32.73300124599735739, 62.10906484417237294, 99.90245962373859356 ) ) ;
#24713 = CARTESIAN_POINT ( 'NONE',  ( -25.21435515916025594, 1.749597353048488237E-16, -4.373993382621220594E-17 ) ) ;
#24714 = CARTESIAN_POINT ( 'NONE',  ( -20.57838717382308147, -29.92853265176832878, -1.611677988432255848 ) ) ;
#24715 = CARTESIAN_POINT ( 'NONE',  ( 25.65782528836480481, 83.52701600504883572, 75.98558751977803638 ) ) ;
#24716 = EDGE_CURVE ( 'NONE', #10555, #4266, #17171, .T. ) ;
#24717 = ORIENTED_EDGE ( 'NONE', *, *, #7165, .T. ) ;
#24718 = ADVANCED_FACE ( 'NONE', ( #16264 ), #8442, .T. ) ;
#24720 = CARTESIAN_POINT ( 'NONE',  ( -6.574463467970464770, -44.27173031830730565, -25.96726214983177528 ) ) ;
#24719 = DIRECTION ( 'NONE',  ( 0.8320502949607718746, 0.000000000000000000, -0.5547001952908368061 ) ) ;
#24721 = CARTESIAN_POINT ( 'NONE',  ( -23.79248802219722947, 3.207402715357613676, 33.03370827286725842 ) ) ;
#24722 = CARTESIAN_POINT ( 'NONE',  ( 24.22246935314087324, -69.99999999999998579, 40.00000000000003553 ) ) ;
#24723 = ORIENTED_EDGE ( 'NONE', *, *, #6351, .T. ) ;
#24724 = CARTESIAN_POINT ( 'NONE',  ( -21.41427618760447160, -29.81030852927061758, 7.777551129310369404 ) ) ;
#24725 = EDGE_CURVE ( 'NONE', #13256, #1421, #717, .T. ) ;
#24726 = LINE ( 'NONE', #7157, #6496 ) ;
#24727 = CARTESIAN_POINT ( 'NONE',  ( 10.93730112725953596, 92.80059208661681680, 119.3442956573276206 ) ) ;
#24728 = ORIENTED_EDGE ( 'NONE', *, *, #23257, .F. ) ;
#24729 = FACE_OUTER_BOUND ( 'NONE', #9133, .T. ) ;
#24730 = VERTEX_POINT ( 'NONE', #18569 ) ;
#24731 = CARTESIAN_POINT ( 'NONE',  ( 1.833485406944043827, 117.0814567582556407, -85.72460230293573602 ) ) ;
#24732 = EDGE_CURVE ( 'NONE', #22719, #654, #6411, .T. ) ;
#24733 =( BOUNDED_SURFACE ( )  B_SPLINE_SURFACE ( 3, 1, ( 
 ( #7945, #18853 ),
 ( #14811, #23621 ),
 ( #3881, #21431 ),
 ( #10502, #3314 ) ),
 .UNSPECIFIED., .F., .F., .F. ) 
 B_SPLINE_SURFACE_WITH_KNOTS ( ( 4, 4 ),
 ( 2, 2 ),
 ( 0.000000000000000000, 1.000000000000000000 ),
 ( 0.000000000000000000, 1.000000000000000000 ),
 .UNSPECIFIED. ) 
 GEOMETRIC_REPRESENTATION_ITEM ( )  RATIONAL_B_SPLINE_SURFACE ( (
 ( 1.000000000000000000, 1.000000000000000000),
 ( 0.9956975270656955868, 0.8568959468854907557),
 ( 0.9956975270656955868, 0.8568959468854907557),
 ( 1.000000000000000000, 1.000000000000000000) ) ) 
 REPRESENTATION_ITEM ( '' )  SURFACE ( )  );
#24734 = VERTEX_POINT ( 'NONE', #24488 ) ;
#24735 = CARTESIAN_POINT ( 'NONE',  ( -1.239374126674604337, 35.79060836339814955, -28.97829083655452820 ) ) ;
#24736 = VERTEX_POINT ( 'NONE', #7074 ) ;
#24737 = CARTESIAN_POINT ( 'NONE',  ( 28.37644542392843405, -111.8804331835011681, -54.25112470585834501 ) ) ;
#24738 = B_SPLINE_CURVE_WITH_KNOTS ( 'NONE', 3,
 ( #9217, #2735, #577, #861, #26907, #1010 ),
 .UNSPECIFIED., .F., .F.,
 ( 4, 2, 4 ),
 ( 1.041737195591640451E-17, 0.0006311571484586107764, 0.001262314296917211144 ),
 .UNSPECIFIED. ) ;
#24739 = EDGE_LOOP ( 'NONE', ( #7484, #19853, #6696, #18621 ) ) ;
#24740 = B_SPLINE_CURVE_WITH_KNOTS ( 'NONE', 3,
 ( #16311, #11285, #9125, #26953, #9273, #9421, #20053, #15734, #4810, #13576 ),
 .UNSPECIFIED., .F., .F.,
 ( 4, 3, 3, 4 ),
 ( 3.816391647148975608E-17, 0.0002669559177086187137, 0.0005339118354150955859, 0.001067817517169158828 ),
 .UNSPECIFIED. ) ;
#24741 = LINE ( 'NONE', #9328, #4634 ) ;
#24742 = CARTESIAN_POINT ( 'NONE',  ( 10.93730112725997294, 26.59437931460951177, -148.8212007290660210 ) ) ;
#24743 = CARTESIAN_POINT ( 'NONE',  ( -21.41427618760458174, 23.81423075802610967, 19.54551635498102158 ) ) ;
#24744 = CARTESIAN_POINT ( 'NONE',  ( -1.323830074806771062, 16.42382241777537644, -43.04593525292974476 ) ) ;
#24745 = CARTESIAN_POINT ( 'NONE',  ( 119.2224693531408803, -90.00000000000005684, -40.00000000000002842 ) ) ;
#24746 = ORIENTED_EDGE ( 'NONE', *, *, #3216, .T. ) ;
#24747 = CARTESIAN_POINT ( 'NONE',  ( 10.93730112725972425, -65.95960219663204782, 136.0306644680981094 ) ) ;
#24748 = CARTESIAN_POINT ( 'NONE',  ( 109.1586059443104944, -0.006808232911144252927, 0.001921075557427531387 ) ) ;
#24749 = EDGE_LOOP ( 'NONE', ( #22461, #22709, #22852, #21509 ) ) ;
#24750 = VERTEX_POINT ( 'NONE', #5178 ) ;
#24751 = CARTESIAN_POINT ( 'NONE',  ( 25.65782528836481546, -91.01210296572892844, -66.83837989650162115 ) ) ;
#24752 = CARTESIAN_POINT ( 'NONE',  ( -55.24300891470648622, -0.008142823778061756071, 0.005486913146696262289 ) ) ;
#24753 = EDGE_CURVE ( 'NONE', #26116, #7560, #24917, .T. ) ;
#24754 = CARTESIAN_POINT ( 'NONE',  ( -25.21435515916042647, 15.02493970636146692, -31.17620025257592786 ) ) ;
#24755 = FACE_OUTER_BOUND ( 'NONE', #13018, .T. ) ;
#24756 = CARTESIAN_POINT ( 'NONE',  ( 1.833721034905647418, 108.0754384393934799, 96.83259691102536237 ) ) ;
#24757 = LINE ( 'NONE', #8769, #8896 ) ;
#24758 = VERTEX_POINT ( 'NONE', #13526 ) ;
#24759 = CARTESIAN_POINT ( 'NONE',  ( 109.1589550718174877, 0.005994046294307805826, 0.004632048724973738749 ) ) ;
#24760 = CARTESIAN_POINT ( 'NONE',  ( 26.11404676487256893, -55.62948129436175293, -98.61392875273419634 ) ) ;
#24761 = CARTESIAN_POINT ( 'NONE',  ( 1.831572820252009626, 145.1082523917587253, -0.9871191512919683664 ) ) ;
#24762 = CARTESIAN_POINT ( 'NONE',  ( 32.73300124599739291, 55.46353551262154014, -103.7392577722169875 ) ) ;
#24763 = EDGE_CURVE ( 'NONE', #20443, #8696, #19460, .T. ) ;
#24764 = DIRECTION ( 'NONE',  ( -1.000000000000000000, 6.938893903907227607E-18, -1.734723475976806902E-18 ) ) ;
#24765 = CARTESIAN_POINT ( 'NONE',  ( 10.93730112725994275, -26.59437931460641025, -148.8212007290665042 ) ) ;
#24766 = ORIENTED_EDGE ( 'NONE', *, *, #8507, .F. ) ;
#24768 = CARTESIAN_POINT ( 'NONE',  ( 1.834118845439484335, 59.18411796427230342, -132.4921483272722185 ) ) ;
#24767 = B_SPLINE_CURVE_WITH_KNOTS ( 'NONE', 3,
 ( #10463, #15316, #14901, #78 ),
 .UNSPECIFIED., .F., .F.,
 ( 4, 4 ),
 ( 6.938893903907228378E-18, 0.008383560773332717278 ),
 .UNSPECIFIED. ) ;
#24769 = VERTEX_POINT ( 'NONE', #1007 ) ;
#24770 = CARTESIAN_POINT ( 'NONE',  ( -8.786685647604885574, 6.096987947571466530E-17, -1.524246986892866633E-17 ) ) ;
#24771 = CARTESIAN_POINT ( 'NONE',  ( -1.463510566862822770, 11.94877850058565727, 44.64091840826476698 ) ) ;
#24772 = ORIENTED_EDGE ( 'NONE', *, *, #13331, .T. ) ;
#24773 = ORIENTED_EDGE ( 'NONE', *, *, #9241, .T. ) ;
#24774 = ORIENTED_EDGE ( 'NONE', *, *, #9684, .T. ) ;
#24775 = CARTESIAN_POINT ( 'NONE',  ( 25.87036335909429496, 84.67915015758852348, 74.91347493818284420 ) ) ;
#24776 = CARTESIAN_POINT ( 'NONE',  ( 109.1592201516379674, -0.007566779963325582538, -0.002134489919768117836 ) ) ;
#24777 = VECTOR ( 'NONE', #17985, 1000.000000000000114 ) ;
#24778 = CARTESIAN_POINT ( 'NONE',  ( -8.786685647604896232, 23.24040270374459993, 48.22796981442743913 ) ) ;
#24779 = CARTESIAN_POINT ( 'NONE',  ( 1.833838848569427249, 125.5797553397079724, -72.70900949568641636 ) ) ;
#24780 = CARTESIAN_POINT ( 'NONE',  ( 30.58324630866343696, 102.7123253644124219, -63.85566901681510643 ) ) ;
#24781 = CARTESIAN_POINT ( 'NONE',  ( 1.833838848569456559, 44.67212175382018557, -138.0625820091619573 ) ) ;
#24782 = DIRECTION ( 'NONE',  ( -1.000000000000000000, -0.000000000000000000, -0.000000000000000000 ) ) ;
#24783 = ORIENTED_EDGE ( 'NONE', *, *, #18488, .T. ) ;
#24784 = ORIENTED_EDGE ( 'NONE', *, *, #13448, .F. ) ;
#24785 = CARTESIAN_POINT ( 'NONE',  ( 26.11404676487257603, 47.08215554553657256, -102.9690087468796662 ) ) ;
#24786 = CARTESIAN_POINT ( 'NONE',  ( -1.259972190295298944, 43.01178231151332909, -16.33417789844387968 ) ) ;
#24787 = EDGE_CURVE ( 'NONE', #21943, #16608, #10730, .T. ) ;
#24788 = CARTESIAN_POINT ( 'NONE',  ( -2.904412668506668460, 47.56768199507434502, 2.864640348250799828 ) ) ;
#24789 = CARTESIAN_POINT ( 'NONE',  ( -20.20700224038492010, 27.82980252387833886, 10.08426345511560207 ) ) ;
#24790 = FACE_OUTER_BOUND ( 'NONE', #8436, .T. ) ;
#24791 = VERTEX_POINT ( 'NONE', #2586 ) ;
#24792 = CARTESIAN_POINT ( 'NONE',  ( -1.619063947482197729, -44.80407745103793360, -11.94059994246142331 ) ) ;
#24793 = DIRECTION ( 'NONE',  ( 0.000000000000000000, 5.223019709708233256E-21, -1.000000000000000000 ) ) ;
#24794 = ADVANCED_FACE ( 'NONE', ( #20288 ), #26176, .F. ) ;
#24795 = EDGE_CURVE ( 'NONE', #5592, #17694, #28365, .T. ) ;
#24796 = CARTESIAN_POINT ( 'NONE',  ( 10.93730112725945602, 84.82621002473440797, 125.1380233598478640 ) ) ;
#24797 = CARTESIAN_POINT ( 'NONE',  ( 25.86096068574582674, -76.38617895399404745, 83.34468010038263230 ) ) ;
#24798 = CARTESIAN_POINT ( 'NONE',  ( 109.1721716018069515, -0.009868622090669465496, -0.01392660302850068019 ) ) ;
#24799 = B_SPLINE_CURVE_WITH_KNOTS ( 'NONE', 3,
 ( #20853, #15952, #16094, #26888 ),
 .UNSPECIFIED., .F., .F.,
 ( 4, 4 ),
 ( 0.000000000000000000, 0.01077107196513859590 ),
 .UNSPECIFIED. ) ;
#24800 = ORIENTED_EDGE ( 'NONE', *, *, #5793, .T. ) ;
#24801 = CARTESIAN_POINT ( 'NONE',  ( 2.108393763691201350, -96.26428731761910740, -108.8265195087758599 ) ) ;
#24802 = ORIENTED_EDGE ( 'NONE', *, *, #11574, .T. ) ;
#24803 = EDGE_CURVE ( 'NONE', #27648, #12565, #20435, .T. ) ;
#24804 = EDGE_LOOP ( 'NONE', ( #12723, #23813, #25669, #10052 ) ) ;
#24805 = VERTEX_POINT ( 'NONE', #14383 ) ;
#24806 = CARTESIAN_POINT ( 'NONE',  ( 55.79472521941426777, 8.328398066092729479, -72.27573336313943742 ) ) ;
#24807 = CARTESIAN_POINT ( 'NONE',  ( 109.1589550718175161, 0.002874971999837422094, -0.007008495014555490496 ) ) ;
#24808 = CARTESIAN_POINT ( 'NONE',  ( -55.24728320129491266, 0.008013189884952347936, 0.01214321324517130159 ) ) ;
#24809 = B_SPLINE_CURVE_WITH_KNOTS ( 'NONE', 3,
 ( #18744, #27517, #7827, #7382 ),
 .UNSPECIFIED., .F., .F.,
 ( 4, 4 ),
 ( 1.895855152355442610E-16, 0.001982023823822946784 ),
 .UNSPECIFIED. ) ;
#24810 = CARTESIAN_POINT ( 'NONE',  ( -25.21435515916043713, 30.48034229288662544, 16.39063784838709736 ) ) ;
#24811 = CARTESIAN_POINT ( 'NONE',  ( 32.73300124599738581, -92.86301839380070078, 72.21147546950520280 ) ) ;
#24812 = ADVANCED_FACE ( 'NONE', ( #10378 ), #2461, .F. ) ;
#24813 = CARTESIAN_POINT ( 'NONE',  ( -1.464342487929843450, 2.431462367721978435, 46.14921266389554688 ) ) ;
#24814 = CARTESIAN_POINT ( 'NONE',  ( 10.93730112726003156, 71.28103789255123957, -133.3192575531793693 ) ) ;
#24815 = CARTESIAN_POINT ( 'NONE',  ( 25.64681081121879203, -34.49579773461859133, 107.5125461021401492 ) ) ;
#24816 = CARTESIAN_POINT ( 'NONE',  ( 25.64681081121879203, 34.49579773461785948, 107.5125461021403765 ) ) ;
#24817 = EDGE_CURVE ( 'NONE', #10890, #2646, #19113, .T. ) ;
#24818 = CARTESIAN_POINT ( 'NONE',  ( 1.893872463202063816, -31.10971550360678606, 141.7768406633803409 ) ) ;
#24819 = CARTESIAN_POINT ( 'NONE',  ( 2.433796855181233454, 60.50726454507903895, 132.3327394885233446 ) ) ;
#24820 = CARTESIAN_POINT ( 'NONE',  ( 9.884929003653608603, -128.2151425008035517, -78.87917189085047198 ) ) ;
#24821 = CARTESIAN_POINT ( 'NONE',  ( 26.28373643307408969, -112.4918671811455511, -60.14387450369948596 ) ) ;
#24822 = B_SPLINE_CURVE_WITH_KNOTS ( 'NONE', 3,
 ( #819, #11469, #22424, #13488, #677, #248, #16070 ),
 .UNSPECIFIED., .F., .F.,
 ( 4, 3, 4 ),
 ( 0.000000000000000000, 0.02398743853561366088, 0.04000277880656216006 ),
 .UNSPECIFIED. ) ;
#24823 = CARTESIAN_POINT ( 'NONE',  ( -20.20700224038492721, -24.51628800869059432, -16.58740185276701951 ) ) ;
#24824 = FACE_OUTER_BOUND ( 'NONE', #21814, .T. ) ;
#24825 = CARTESIAN_POINT ( 'NONE',  ( 1.832998868059890096, -125.9352106559978921, -72.09222286251215905 ) ) ;
#24826 = CARTESIAN_POINT ( 'NONE',  ( 109.1592201516379674, 0.007566779963318552571, -0.002134489919774391464 ) ) ;
#24827 = CARTESIAN_POINT ( 'NONE',  ( 25.64708228042118421, 83.93578330383188302, -75.52311986517946707 ) ) ;
#24828 = VERTEX_POINT ( 'NONE', #1704 ) ;
#24829 = ORIENTED_EDGE ( 'NONE', *, *, #12262, .T. ) ;
#24830 = CARTESIAN_POINT ( 'NONE',  ( 25.64670758986457955, 103.3508631837550809, -45.46974729533181403 ) ) ;
#24831 = CARTESIAN_POINT ( 'NONE',  ( -1.019300379054419947, 35.83762006677442002, 28.53917295602858673 ) ) ;
#24832 = ORIENTED_EDGE ( 'NONE', *, *, #10275, .T. ) ;
#24833 = ORIENTED_EDGE ( 'NONE', *, *, #8265, .F. ) ;
#24834 = ORIENTED_EDGE ( 'NONE', *, *, #21808, .F. ) ;
#24835 = CARTESIAN_POINT ( 'NONE',  ( 32.73300124599738581, -16.10546300444743650, -116.5274707358856858 ) ) ;
#24836 = FACE_OUTER_BOUND ( 'NONE', #10403, .T. ) ;
#24837 = EDGE_CURVE ( 'NONE', #25524, #7798, #19138, .T. ) ;
#24838 = DIRECTION ( 'NONE',  ( 0.7637818620346802367, -0.2198041754873842346, 0.6068965246771050870 ) ) ;
#24839 = CARTESIAN_POINT ( 'NONE',  ( 25.64692232868534205, -66.10288322707258146, 91.53874134430776621 ) ) ;
#24840 = ADVANCED_FACE ( 'NONE', ( #3733 ), #16439, .F. ) ;
#24841 = CARTESIAN_POINT ( 'NONE',  ( -1.619063947482201282, 11.94059994246159384, -44.80407745103787676 ) ) ;
#24842 = CARTESIAN_POINT ( 'NONE',  ( 1.833485406944057594, -84.86072343962649711, 117.7091014914947209 ) ) ;
#24843 = VECTOR ( 'NONE', #7713, 1000.000000000000114 ) ;
#24844 = CARTESIAN_POINT ( 'NONE',  ( 25.70243777736188662, -110.3252221127464452, -24.19989514742834658 ) ) ;
#24845 = CARTESIAN_POINT ( 'NONE',  ( -1.049817751779888342, 27.33161971822197955, -36.75003908324300994 ) ) ;
#24846 = CARTESIAN_POINT ( 'NONE',  ( 32.73300124599735739, -81.52272205837257957, 84.80615050150346690 ) ) ;
#24847 = ORIENTED_EDGE ( 'NONE', *, *, #8005, .F. ) ;
#24848 = VERTEX_POINT ( 'NONE', #14227 ) ;
#24849 = CARTESIAN_POINT ( 'NONE',  ( -1.031422197589716205, 44.01264471863849082, -12.69107518035517046 ) ) ;
#24851 = CARTESIAN_POINT ( 'NONE',  ( 25.86096068574583029, 57.38862431273717846, -97.40497849554822096 ) ) ;
#24850 = CARTESIAN_POINT ( 'NONE',  ( 55.79472521941428198, 6.880567342320674129, -72.42790650415567200 ) ) ;
#24852 = CARTESIAN_POINT ( 'NONE',  ( 1.832998868059858122, -44.33343224355328971, 138.1720401012265427 ) ) ;
#24853 = CARTESIAN_POINT ( 'NONE',  ( -25.21435515916043713, -34.29329011225952684, 4.655591116594705703 ) ) ;
#24854 = ORIENTED_EDGE ( 'NONE', *, *, #13944, .T. ) ;
#24855 = ORIENTED_EDGE ( 'NONE', *, *, #23364, .T. ) ;
#24856 = CARTESIAN_POINT ( 'NONE',  ( 1.833485406944057594, -30.69200235378832176, -141.8265699653870513 ) ) ;
#24857 = CARTESIAN_POINT ( 'NONE',  ( -22.23342874802668589, 16.78332232459680640, 26.81018246605520972 ) ) ;
#24858 = FACE_OUTER_BOUND ( 'NONE', #16433, .T. ) ;
#24859 = EDGE_LOOP ( 'NONE', ( #4375, #8014, #15412, #4459 ) ) ;
#24860 = CARTESIAN_POINT ( 'NONE',  ( -20.57838717382308147, -7.715628353033886278, -28.96176188950215646 ) ) ;
#24861 = VERTEX_POINT ( 'NONE', #23049 ) ;
#24862 = FACE_OUTER_BOUND ( 'NONE', #4986, .T. ) ;
#24863 = VECTOR ( 'NONE', #20299, 1000.000000000000114 ) ;
#24864 = CARTESIAN_POINT ( 'NONE',  ( 10.93730112725971004, 10.89264110825002163, 150.7858122213661147 ) ) ;
#24865 = CARTESIAN_POINT ( 'NONE',  ( 1.894214914920947068, -132.2104617488241445, 59.90782071839149836 ) ) ;
#24866 = LINE ( 'NONE', #20528, #17899 ) ;
#24867 = CIRCLE ( 'NONE', #5541, 34.60786435723138510 ) ;
#24868 = EDGE_CURVE ( 'NONE', #28115, #17891, #24987, .T. ) ;
#24869 = EDGE_LOOP ( 'NONE', ( #270, #28286, #11692, #6357 ) ) ;
#24870 = CARTESIAN_POINT ( 'NONE',  ( 19.66333377628710366, -123.9466021833767684, -60.10102584214492794 ) ) ;
#24871 = B_SPLINE_CURVE_WITH_KNOTS ( 'NONE', 3,
 ( #21424, #14803, #28307, #19541, #25896, #24158, #1700 ),
 .UNSPECIFIED., .F., .F.,
 ( 4, 3, 4 ),
 ( 1.114146325429624918E-17, 0.009512539173626377575, 0.02506242213020845946 ),
 .UNSPECIFIED. ) ;
#24872 = EDGE_CURVE ( 'NONE', #23610, #27689, #18442, .T. ) ;
#24873 = EDGE_LOOP ( 'NONE', ( #9099, #3023, #11478, #21618 ) ) ;
#24874 =( NAMED_UNIT ( * ) SI_UNIT ( $, .STERADIAN. ) SOLID_ANGLE_UNIT ( ) );
#24875 = LINE ( 'NONE', #386, #12907 ) ;
#24876 = EDGE_CURVE ( 'NONE', #23391, #9533, #16735, .T. ) ;
#24877 = CARTESIAN_POINT ( 'NONE',  ( 1.834118845439484335, 117.2918069668812393, -85.43746956709730966 ) ) ;
#24878 = DIRECTION ( 'NONE',  ( 0.000000000000000000, 5.223019709707975211E-21, -1.000000000000000000 ) ) ;
#24879 = CARTESIAN_POINT ( 'NONE',  ( -22.23226125620929139, -2.179935373562669643, -31.55376588768476509 ) ) ;
#24880 = B_SPLINE_CURVE_WITH_KNOTS ( 'NONE', 3,
 ( #26002, #24000, #7005, #2964, #3100, #3241, #506, #15761, #11737, #26840 ),
 .UNSPECIFIED., .F., .F.,
 ( 4, 2, 2, 2, 4 ),
 ( 1.563658610346375379E-18, 0.0003346267210630954943, 0.0006692534421261893624, 0.001003880163189283230, 0.001338506884252377207 ),
 .UNSPECIFIED. ) ;
#24881 = ORIENTED_EDGE ( 'NONE', *, *, #426, .F. ) ;
#24882 = EDGE_CURVE ( 'NONE', #8623, #5605, #17060, .T. ) ;
#24883 = CARTESIAN_POINT ( 'NONE',  ( 1.833206310202330158, -96.54250248081064001, 108.3342540861875705 ) ) ;
#24884 = CARTESIAN_POINT ( 'NONE',  ( 26.04756280548353686, 98.56594554799121966, 55.62433096787456321 ) ) ;
#24885 = ORIENTED_EDGE ( 'NONE', *, *, #11341, .F. ) ;
#24886 = CIRCLE ( 'NONE', #14759, 151.1787379149930359 ) ;
#24887 = ORIENTED_EDGE ( 'NONE', *, *, #25197, .F. ) ;
#24888 = ORIENTED_EDGE ( 'NONE', *, *, #18532, .T. ) ;
#24889 = DIRECTION ( 'NONE',  ( -0.000000000000000000, 1.000000000000000000, -0.000000000000000000 ) ) ;
#24890 = CARTESIAN_POINT ( 'NONE',  ( -28.13707043255157103, -12.83104814250467562, -18.96624908365841478 ) ) ;
#24892 = CARTESIAN_POINT ( 'NONE',  ( -24.53237795827023859, -3.868415699415882258, -33.71192251888856362 ) ) ;
#24891 = CARTESIAN_POINT ( 'NONE',  ( -19.53423201713129842, 1.353948732986041533E-16, 28.92774122539760384 ) ) ;
#24893 = AXIS2_PLACEMENT_3D ( 'NONE', #14025, #18494, #22837 ) ;
#24894 = DIRECTION ( 'NONE',  ( 0.000000000000000000, 1.110223024625156343E-15, 1.000000000000000000 ) ) ;
#24895 = CARTESIAN_POINT ( 'NONE',  ( -1.045287976400386842, -28.14015102489780062, 36.12803364096639314 ) ) ;
#24896 = ORIENTED_EDGE ( 'NONE', *, *, #2038, .T. ) ;
#24897 = CARTESIAN_POINT ( 'NONE',  ( -25.21435515916025594, 1.749597353048488237E-16, -4.373993382621220594E-17 ) ) ;
#24898 = FACE_OUTER_BOUND ( 'NONE', #12225, .T. ) ;
#24899 = CIRCLE ( 'NONE', #12001, 28.92774122539760384 ) ;
#24900 = DIRECTION ( 'NONE',  ( -5.541455922705464902E-20, 5.223019709708320524E-21, -1.000000000000000000 ) ) ;
#24901 = DIRECTION ( 'NONE',  ( 1.000000000000000000, -6.938893903907226837E-18, -5.541455922705464902E-20 ) ) ;
#24902 = CARTESIAN_POINT ( 'NONE',  ( 109.1586900883932856, 0.002301750759599774983, -0.006757191295060855155 ) ) ;
#24903 = CARTESIAN_POINT ( 'NONE',  ( -25.21435515916043002, 34.05351380035335040, -6.169479169075572145 ) ) ;
#24904 = ORIENTED_EDGE ( 'NONE', *, *, #16114, .F. ) ;
#24905 = LINE ( 'NONE', #22896, #2930 ) ;
#24906 =( BOUNDED_SURFACE ( )  B_SPLINE_SURFACE ( 3, 1, ( 
 ( #19508, #15458 ),
 ( #4245, #1942 ),
 ( #8866, #11021 ),
 ( #13031, #10748 ) ),
 .UNSPECIFIED., .F., .F., .F. ) 
 B_SPLINE_SURFACE_WITH_KNOTS ( ( 4, 4 ),
 ( 2, 2 ),
 ( 0.000000000000000000, 1.000000000000000000 ),
 ( 0.000000000000000000, 1.000000000000000000 ),
 .UNSPECIFIED. ) 
 GEOMETRIC_REPRESENTATION_ITEM ( )  RATIONAL_B_SPLINE_SURFACE ( (
 ( 1.000000000000000000, 1.000000000000000000),
 ( 0.6386103224230302855, 0.9954351624131538845),
 ( 0.6386103224230302855, 0.9954351624131538845),
 ( 1.000000000000000000, 1.000000000000000000) ) ) 
 REPRESENTATION_ITEM ( '' )  SURFACE ( )  );
#24907 = CYLINDRICAL_SURFACE ( 'NONE', #11550, 37.50000000000001421 ) ;
#24908 = DIRECTION ( 'NONE',  ( 0.000000000000000000, -5.223019709708233256E-21, 1.000000000000000000 ) ) ;
#24909 = ORIENTED_EDGE ( 'NONE', *, *, #8433, .T. ) ;
#24910 = ORIENTED_EDGE ( 'NONE', *, *, #6928, .F. ) ;
#24911 = ORIENTED_EDGE ( 'NONE', *, *, #25719, .T. ) ;
#24912 = AXIS2_PLACEMENT_3D ( 'NONE', #24770, #25332, #23039 ) ;
#24913 = EDGE_CURVE ( 'NONE', #11774, #15699, #4010, .T. ) ;
#24914 = DIRECTION ( 'NONE',  ( -1.000000000000000000, -0.000000000000000000, -0.000000000000000000 ) ) ;
#24915 = CIRCLE ( 'NONE', #22616, 117.6351876552689504 ) ;
#24916 = EDGE_CURVE ( 'NONE', #13041, #20671, #12572, .T. ) ;
#24917 = LINE ( 'NONE', #14090, #12130 ) ;
#24918 = CARTESIAN_POINT ( 'NONE',  ( 8.186469829614045679, 108.6390983847750107, 102.4860667297597416 ) ) ;
#24919 = CARTESIAN_POINT ( 'NONE',  ( 10.93730112726005999, 128.3908183996603327, -79.81734490845792607 ) ) ;
#24920 = CARTESIAN_POINT ( 'NONE',  ( 1.833809397773857874, 45.01060836636703044, -137.9524943416720930 ) ) ;
#24921 = CARTESIAN_POINT ( 'NONE',  ( 109.1586900883932856, 0.005833932871491316619, 0.004113747440992344268 ) ) ;
#24922 = ORIENTED_EDGE ( 'NONE', *, *, #13846, .F. ) ;
#24923 = ORIENTED_EDGE ( 'NONE', *, *, #6771, .F. ) ;
#24924 = CARTESIAN_POINT ( 'NONE',  ( -1.049817751779889008, -43.39729912094389874, -14.63752841325032250 ) ) ;
#24925 = CARTESIAN_POINT ( 'NONE',  ( 28.43349137099828994, 120.6297847406441122, -29.78331910005377026 ) ) ;
#24926 = CARTESIAN_POINT ( 'NONE',  ( -6.574463467970651287, -5.014313797967385966, -51.07975593197902953 ) ) ;
#24927 = DIRECTION ( 'NONE',  ( -1.000000000000000000, -0.000000000000000000, -0.000000000000000000 ) ) ;
#24928 = CARTESIAN_POINT ( 'NONE',  ( 1.832998868059890096, -108.1944082009163566, 96.70023740551089020 ) ) ;
#24929 = CARTESIAN_POINT ( 'NONE',  ( 1.833838850855475489, -138.0350826608190573, 44.75675607098882836 ) ) ;
#24930 = ORIENTED_EDGE ( 'NONE', *, *, #12850, .T. ) ;
#24931 = CARTESIAN_POINT ( 'NONE',  ( -1.056502255334264895, 13.66916755949850604, -43.72121397317227576 ) ) ;
#24932 = DIRECTION ( 'NONE',  ( 0.000000000000000000, 0.000000000000000000, 1.000000000000000000 ) ) ;
#24933 = B_SPLINE_CURVE_WITH_KNOTS ( 'NONE', 3,
 ( #11373, #19722, #26621, #8948, #26483, #7614 ),
 .UNSPECIFIED., .F., .F.,
 ( 4, 2, 4 ),
 ( 0.000000000000000000, 0.0004335151646191504364, 0.0008670303292383008727 ),
 .UNSPECIFIED. ) ;
#24934 = CARTESIAN_POINT ( 'NONE',  ( -1.323830074806768176, 44.47857376182273015, -12.01461446423216906 ) ) ;
#24935 = CARTESIAN_POINT ( 'NONE',  ( 30.59138290137880745, -44.78723476287375860, 107.2355347544031616 ) ) ;
#24936 = CARTESIAN_POINT ( 'NONE',  ( 25.64681081121879203, -107.5125461021405044, 34.49579773461748999 ) ) ;
#24937 = ORIENTED_EDGE ( 'NONE', *, *, #4879, .F. ) ;
#24939 =( BOUNDED_SURFACE ( )  B_SPLINE_SURFACE ( 3, 1, ( 
 ( #6728, #11318 ),
 ( #24286, #7160 ),
 ( #15920, #24584 ),
 ( #13319, #2379 ) ),
 .UNSPECIFIED., .F., .F., .F. ) 
 B_SPLINE_SURFACE_WITH_KNOTS ( ( 4, 4 ),
 ( 2, 2 ),
 ( 0.000000000000000000, 1.000000000000000000 ),
 ( 0.000000000000000000, 1.000000000000000000 ),
 .UNSPECIFIED. ) 
 GEOMETRIC_REPRESENTATION_ITEM ( )  RATIONAL_B_SPLINE_SURFACE ( (
 ( 1.000000000000000000, 1.000000000000000000),
 ( 0.9956975270656955868, 0.8568959468854907557),
 ( 0.9956975270656955868, 0.8568959468854907557),
 ( 1.000000000000000000, 1.000000000000000000) ) ) 
 REPRESENTATION_ITEM ( '' )  SURFACE ( )  );
#24938 = AXIS2_PLACEMENT_3D ( 'NONE', #7830, #896, #3203 ) ;
#24940 = VERTEX_POINT ( 'NONE', #4290 ) ;
#24941 = CARTESIAN_POINT ( 'NONE',  ( 10.93730112725990367, -125.1380233598473950, -84.82621002473567273 ) ) ;
#24942 = ORIENTED_EDGE ( 'NONE', *, *, #13443, .F. ) ;
#24943 = B_SPLINE_CURVE_WITH_KNOTS ( 'NONE', 3,
 ( #723, #9513, #27042, #7352, #28185, #4152, #14948, #5916, #16851, #25909 ),
 .UNSPECIFIED., .F., .F.,
 ( 4, 2, 2, 2, 4 ),
 ( 2.884421207865725401E-16, 0.0003346187017559067080, 0.0006692374035115243678, 0.001003856105267142028, 0.001338474807022759687 ),
 .UNSPECIFIED. ) ;
#24944 = ORIENTED_EDGE ( 'NONE', *, *, #22936, .T. ) ;
#24945 = ORIENTED_EDGE ( 'NONE', *, *, #22535, .T. ) ;
#24946 = CARTESIAN_POINT ( 'NONE',  ( 2.430230287190589422, 86.70145658344658557, 116.8646894862415166 ) ) ;
#24947 = B_SPLINE_CURVE_WITH_KNOTS ( 'NONE', 3,
 ( #10994, #8982, #19907, #2631, #9115, #4497, #8686, #4651 ),
 .UNSPECIFIED., .F., .F.,
 ( 4, 2, 2, 4 ),
 ( 2.251264292202123005E-16, 0.002761568181852872006, 0.005523136363705519365, 0.01104627272741081322 ),
 .UNSPECIFIED. ) ;
#24948 = EDGE_CURVE ( 'NONE', #4790, #22518, #898, .T. ) ;
#24949 = CARTESIAN_POINT ( 'NONE',  ( -1.056502255334265339, -43.40574022158784118, -14.64009593116085739 ) ) ;
#24950 = ADVANCED_FACE ( 'NONE', ( #14939 ), #23155, .T. ) ;
#24951 = CARTESIAN_POINT ( 'NONE',  ( 2.430230287190581429, -144.8619874886007892, 13.76600171652596849 ) ) ;
#24952 = EDGE_CURVE ( 'NONE', #14748, #391, #7063, .T. ) ;
#24953 = CARTESIAN_POINT ( 'NONE',  ( 2.263178113027024096, -98.32595894905907130, 107.1074314657341091 ) ) ;
#24954 = AXIS2_PLACEMENT_3D ( 'NONE', #4529, #22096, #24409 ) ;
#24955 = CARTESIAN_POINT ( 'NONE',  ( -10.86508079875801691, 6.877801422380844798, -50.67624451685624365 ) ) ;
#24956 = CARTESIAN_POINT ( 'NONE',  ( 2.433796855181233454, -144.8571464219888298, -13.76554153471842312 ) ) ;
#24957 = CARTESIAN_POINT ( 'NONE',  ( 1.833485406944057594, 107.4794113447422603, -97.49333871408586560 ) ) ;
#24958 = CARTESIAN_POINT ( 'NONE',  ( 109.1592201516379674, 0.007856029051022768092, -0.0003082430542016078114 ) ) ;
#24959 = DIRECTION ( 'NONE',  ( 0.5946245182733607137, 0.08110646981858531113, 0.7999021332774032267 ) ) ;
#24961 = CARTESIAN_POINT ( 'NONE',  ( 25.98552792386799126, -83.35136888841289249, 76.50165414343540249 ) ) ;
#24960 = CARTESIAN_POINT ( 'NONE',  ( -10.86508079875781263, 9.118642906269942117, 50.32133009257457701 ) ) ;
#24962 = CARTESIAN_POINT ( 'NONE',  ( 26.04756280548352976, 76.55292122840037905, 83.36043467252048345 ) ) ;
#24963 = CARTESIAN_POINT ( 'NONE',  ( 28.37644542392847313, 76.32685750075128794, -98.15613422114005004 ) ) ;
#24964 = B_SPLINE_CURVE_WITH_KNOTS ( 'NONE', 3,
 ( #6164, #19515, #17346, #26136, #2085, #15177 ),
 .UNSPECIFIED., .F., .F.,
 ( 4, 2, 4 ),
 ( 3.607901639910057446E-16, 0.003576372551511165700, 0.007152745103021970578 ),
 .UNSPECIFIED. ) ;
#24965 = FACE_OUTER_BOUND ( 'NONE', #25720, .T. ) ;
#24966 = CARTESIAN_POINT ( 'NONE',  ( 109.1624594426973118, -0.008380433676413013774, -0.01358749486988779405 ) ) ;
#24967 = CARTESIAN_POINT ( 'NONE',  ( 28.43349137099834678, -120.6297847406439558, 29.78331910005459093 ) ) ;
#24968 = EDGE_CURVE ( 'NONE', #7628, #3847, #4006, .T. ) ;
#24969 = ORIENTED_EDGE ( 'NONE', *, *, #19645, .T. ) ;
#24970 = CARTESIAN_POINT ( 'NONE',  ( 55.49584447822657296, 66.16986612640816645, -29.75369869230888753 ) ) ;
#24971 = VERTEX_POINT ( 'NONE', #10784 ) ;
#24972 = CARTESIAN_POINT ( 'NONE',  ( -20.20612091757420359, 23.26073043121660433, 18.30568244821352408 ) ) ;
#24973 = CARTESIAN_POINT ( 'NONE',  ( 25.64670758986457599, -12.29747533046042740, 112.2393466678477694 ) ) ;
#24974 = VERTEX_POINT ( 'NONE', #2112 ) ;
#24975 = VECTOR ( 'NONE', #5930, 1000.000000000000000 ) ;
#24976 = EDGE_CURVE ( 'NONE', #26958, #16481, #22901, .T. ) ;
#24977 = ORIENTED_EDGE ( 'NONE', *, *, #6406, .F. ) ;
#24978 = B_SPLINE_CURVE_WITH_KNOTS ( 'NONE', 3,
 ( #25427, #5547, #14032, #10024 ),
 .UNSPECIFIED., .F., .F.,
 ( 4, 4 ),
 ( 0.000000000000000000, 0.01077107196513844151 ),
 .UNSPECIFIED. ) ;
#24979 = VECTOR ( 'NONE', #20086, 1000.000000000000227 ) ;
#24980 = ORIENTED_EDGE ( 'NONE', *, *, #13312, .T. ) ;
#24981 = EDGE_CURVE ( 'NONE', #20437, #20945, #16348, .T. ) ;
#24982 = ADVANCED_FACE ( 'NONE', ( #6459, #8346 ), #6744, .F. ) ;
#24983 = CARTESIAN_POINT ( 'NONE',  ( 109.1586900883932856, -0.001582822706024301744, 0.006960773163856025063 ) ) ;
#24984 = FACE_OUTER_BOUND ( 'NONE', #26851, .T. ) ;
#24985 = B_SPLINE_CURVE_WITH_KNOTS ( 'NONE', 3,
 ( #13066, #24025, #8898, #105 ),
 .UNSPECIFIED., .F., .F.,
 ( 4, 4 ),
 ( 3.141122122899962401E-16, 0.01077107486149752116 ),
 .UNSPECIFIED. ) ;
#24986 = CARTESIAN_POINT ( 'NONE',  ( 1.831572820252008738, -84.49389457294057593, -117.9752562883675466 ) ) ;
#24987 = B_SPLINE_CURVE_WITH_KNOTS ( 'NONE', 3,
 ( #16546, #10085, #21429, #14526 ),
 .UNSPECIFIED., .F., .F.,
 ( 4, 4 ),
 ( 6.721062925282177188E-16, 0.008383748772660126747 ),
 .UNSPECIFIED. ) ;
#24988 = B_SPLINE_CURVE_WITH_KNOTS ( 'NONE', 3,
 ( #2520, #2226, #13603, #24720, #9445, #4969, #22404, #20217 ),
 .UNSPECIFIED., .F., .F.,
 ( 4, 2, 2, 4 ),
 ( 0.000000000000000000, 0.002761524886576556103, 0.005523049773153112206, 0.01104609954630622441 ),
 .UNSPECIFIED. ) ;
#24989 = CARTESIAN_POINT ( 'NONE',  ( 1.833838850855475266, 144.3241377520101025, -15.07960613928478644 ) ) ;
#24990 = CARTESIAN_POINT ( 'NONE',  ( -7.078251931573406708, 38.93060825814230697, -34.59014398252930533 ) ) ;
#24991 = CARTESIAN_POINT ( 'NONE',  ( 109.1624594426973118, 0.0004639210235602615490, 0.01595733256932007488 ) ) ;
#24992 = CARTESIAN_POINT ( 'NONE',  ( 0.000000000000000000, 0.000000000000000000, 0.000000000000000000 ) ) ;
#24993 = CARTESIAN_POINT ( 'NONE',  ( -1.239374126674604337, 16.50008610789298302, -42.99367564261284258 ) ) ;
#24994 = FACE_OUTER_BOUND ( 'NONE', #3959, .T. ) ;
#24995 = CARTESIAN_POINT ( 'NONE',  ( -1.619063947482197729, 25.20140673341430571, 38.92136151114879539 ) ) ;
#24996 = CARTESIAN_POINT ( 'NONE',  ( 109.1778270068192853, -0.002278716897417678439, -0.009031542838326005879 ) ) ;
#24997 = CARTESIAN_POINT ( 'NONE',  ( -1.050230347699842692, 1.897926697972695375E-16, 45.79907861674080749 ) ) ;
#24998 = CIRCLE ( 'NONE', #13942, 117.6351876552689504 ) ;
#24999 = ORIENTED_EDGE ( 'NONE', *, *, #20997, .T. ) ;
#25000 = ORIENTED_EDGE ( 'NONE', *, *, #4039, .F. ) ;
#25001 = CARTESIAN_POINT ( 'NONE',  ( -28.41354790283022069, -8.345538364876929904, 21.64275480268756269 ) ) ;
#25002 = VECTOR ( 'NONE', #16269, 999.9999999999998863 ) ;
#25004 = CARTESIAN_POINT ( 'NONE',  ( 10.93730112726002623, 56.95489579269933955, -140.0398180619107507 ) ) ;
#25003 = CARTESIAN_POINT ( 'NONE',  ( 25.64681081121879203, 66.03065707439057519, -91.59071981940505225 ) ) ;
#25005 = CARTESIAN_POINT ( 'NONE',  ( -12.94347594948484392, -8.691477019903656398, -47.96504705787742040 ) ) ;
#25006 = CARTESIAN_POINT ( 'NONE',  ( 2.433796855181205476, 138.8296532063094162, -43.58222566461498815 ) ) ;
#25007 = CARTESIAN_POINT ( 'NONE',  ( -25.21435515916043713, 25.00736669481056751, 23.92354251275909505 ) ) ;
#25008 = ORIENTED_EDGE ( 'NONE', *, *, #27691, .F. ) ;
#25009 = CARTESIAN_POINT ( 'NONE',  ( 2.433796855181205476, -46.34326152018838485, 137.9325382748283744 ) ) ;
#25010 = CARTESIAN_POINT ( 'NONE',  ( -1.044557008772710072, 45.76404748504490527, 1.643388457098048372 ) ) ;
#25011 = CARTESIAN_POINT ( 'NONE',  ( -1.113548883309548376, -38.22628252420791739, 25.34012683631596374 ) ) ;
#25012 = EDGE_LOOP ( 'NONE', ( #13801, #15578, #21769, #7097 ) ) ;
#25013 = LINE ( 'NONE', #20658, #10533 ) ;
#25014 = FACE_OUTER_BOUND ( 'NONE', #688, .T. ) ;
#25015 = EDGE_CURVE ( 'NONE', #26642, #10842, #24300, .T. ) ;
#25016 = EDGE_CURVE ( 'NONE', #24473, #19926, #8753, .T. ) ;
#25017 = CARTESIAN_POINT ( 'NONE',  ( 26.11404676487257603, -65.63269960453179408, -92.25884714080473259 ) ) ;
#25018 = EDGE_CURVE ( 'NONE', #3333, #8623, #13333, .T. ) ;
#25019 = B_SPLINE_CURVE_WITH_KNOTS ( 'NONE', 3,
 ( #2609, #4779, #7238, #22347, #11390, #17854, #13396, #452 ),
 .UNSPECIFIED., .F., .F.,
 ( 4, 2, 2, 4 ),
 ( 2.860979249076398407E-17, 0.0002429592666046945682, 0.0004859185332093605134, 0.0009718370664186819956 ),
 .UNSPECIFIED. ) ;
#25020 = VERTEX_POINT ( 'NONE', #19408 ) ;
#25021 = CARTESIAN_POINT ( 'NONE',  ( 9.884929003653626367, -148.0628878137278832, -27.17402761732495975 ) ) ;
#25022 = VERTEX_POINT ( 'NONE', #5139 ) ;
#25023 = CARTESIAN_POINT ( 'NONE',  ( 26.11404676487256893, 1.130420376098718593, -113.2169081140373663 ) ) ;
#25024 = ORIENTED_EDGE ( 'NONE', *, *, #24872, .F. ) ;
#25025 = CIRCLE ( 'NONE', #15765, 151.1787379149930359 ) ;
#25026 = CARTESIAN_POINT ( 'NONE',  ( -20.38016308990359349, -10.62413300761005353, -27.81387210821418776 ) ) ;
#25027 = CARTESIAN_POINT ( 'NONE',  ( -20.21097721712959938, -17.13687106192361398, -24.14932359587282917 ) ) ;
#25028 = CARTESIAN_POINT ( 'NONE',  ( 19.66333377628703261, 137.6761449113044478, 4.491394265032717215 ) ) ;
#25029 = CARTESIAN_POINT ( 'NONE',  ( -55.25719721206881729, 0.01079965405819919254, 0.002847566758682530588 ) ) ;
#25030 = VERTEX_POINT ( 'NONE', #9330 ) ;
#25031 = LINE ( 'NONE', #15174, #5208 ) ;
#25032 = CARTESIAN_POINT ( 'NONE',  ( -20.20700224038492721, 0.9908225410478516126, -29.58392382092673145 ) ) ;
#25033 = CARTESIAN_POINT ( 'NONE',  ( 30.59138290137909877, -2.701446546447516361, -116.1811451928595318 ) ) ;
#25034 = ORIENTED_EDGE ( 'NONE', *, *, #9941, .F. ) ;
#25035 = EDGE_LOOP ( 'NONE', ( #11860, #7180, #490, #13378 ) ) ;
#25036 = ORIENTED_EDGE ( 'NONE', *, *, #26328, .T. ) ;
#25037 = DIRECTION ( 'NONE',  ( 0.000000000000000000, 5.223019709707975211E-21, -1.000000000000000000 ) ) ;
#25038 = CARTESIAN_POINT ( 'NONE',  ( -55.24340739397742084, 0.008612749836246956503, -0.005344433640973183380 ) ) ;
#25040 = CARTESIAN_POINT ( 'NONE',  ( 109.1587776205901861, 0.007280006032835106486, -0.0008489206734500846221 ) ) ;
#25039 = DIRECTION ( 'NONE',  ( 0.000000000000000000, 0.000000000000000000, 1.000000000000000000 ) ) ;
#25041 = CARTESIAN_POINT ( 'NONE',  ( -1.045287976400365970, 1.530335034933814731, -45.76855895860946788 ) ) ;
#25042 = CARTESIAN_POINT ( 'NONE',  ( 28.37603512858355970, 10.20681926544516216, -114.2774673387025075 ) ) ;
#25043 = CARTESIAN_POINT ( 'NONE',  ( -1.019300379054419725, -35.83762006677378764, 28.53917295602937187 ) ) ;
#25044 = ORIENTED_EDGE ( 'NONE', *, *, #22907, .F. ) ;
#25045 = CARTESIAN_POINT ( 'NONE',  ( 28.37599760073042532, 104.0705811520814024, 48.29934869928204222 ) ) ;
#25046 = CARTESIAN_POINT ( 'NONE',  ( -25.21435515916043713, 30.48034229288662544, 16.39063784838709736 ) ) ;
#25047 = DIRECTION ( 'NONE',  ( -1.000000000000000000, -0.000000000000000000, -0.000000000000000000 ) ) ;
#25048 = ADVANCED_FACE ( 'NONE', ( #22726 ), #8380, .F. ) ;
#25049 = FACE_OUTER_BOUND ( 'NONE', #24198, .T. ) ;
#25050 = CARTESIAN_POINT ( 'NONE',  ( 1.832998868059890096, 108.1944082009169961, -96.70023740551017966 ) ) ;
#25051 = CARTESIAN_POINT ( 'NONE',  ( 21.16825799904932381, 125.4548537968709638, 51.02216409572595524 ) ) ;
#25052 = CARTESIAN_POINT ( 'NONE',  ( 26.11404676487259024, -12.95861723607377414, -112.4785329405483338 ) ) ;
#25054 = ADVANCED_FACE ( 'NONE', ( #7458 ), #13916, .T. ) ;
#25053 = CARTESIAN_POINT ( 'NONE',  ( 32.73300124599737160, -89.94078864464117373, 75.82012867748450446 ) ) ;
#25055 = CARTESIAN_POINT ( 'NONE',  ( 2.433796855181233454, -142.6247129145646397, -28.83182736670683610 ) ) ;
#25056 = EDGE_CURVE ( 'NONE', #23267, #1161, #15989, .T. ) ;
#25057 = VERTEX_POINT ( 'NONE', #18223 ) ;
#25058 = ORIENTED_EDGE ( 'NONE', *, *, #23934, .F. ) ;
#25059 = CARTESIAN_POINT ( 'NONE',  ( -4.162674018437130030, -18.33413805792406492, 45.34593312138898824 ) ) ;
#25060 = CARTESIAN_POINT ( 'NONE',  ( -55.24390624410018802, -0.001811362924362171613, 0.01027195578988007209 ) ) ;
#25061 = FACE_OUTER_BOUND ( 'NONE', #2829, .T. ) ;
#25062 = CARTESIAN_POINT ( 'NONE',  ( 1.833206310202348588, 58.34025049825128661, -132.8652722326992546 ) ) ;
#25063 = CARTESIAN_POINT ( 'NONE',  ( -20.37983603106073716, 23.16947629293390065, 18.69865230096500852 ) ) ;
#25064 = CARTESIAN_POINT ( 'NONE',  ( -1.619063947482197729, -25.20140673341401438, -38.92136151114898723 ) ) ;
#25065 = CARTESIAN_POINT ( 'NONE',  ( 1.833485406944057594, 44.33323125130110043, -138.1714136985304151 ) ) ;
#25066 = CARTESIAN_POINT ( 'NONE',  ( 1.832998868059858122, -132.7810136645734360, -58.53348008137778180 ) ) ;
#25067 = ORIENTED_EDGE ( 'NONE', *, *, #21812, .F. ) ;
#25068 = ORIENTED_EDGE ( 'NONE', *, *, #11705, .T. ) ;
#25069 = CARTESIAN_POINT ( 'NONE',  ( 6.224689322667630975, -121.2721959030543672, 84.93872395422938837 ) ) ;
#25070 = CARTESIAN_POINT ( 'NONE',  ( 30.58324630866341565, -16.55818995381066472, -119.8048187378265794 ) ) ;
#25071 = CARTESIAN_POINT ( 'NONE',  ( 10.93730112725932635, 0.000000000000000000, -151.1787379149930359 ) ) ;
#25072 = CARTESIAN_POINT ( 'NONE',  ( 109.1592201516379674, -0.007620268632971095163, 0.001934867487021801630 ) ) ;
#25073 =( BOUNDED_SURFACE ( )  B_SPLINE_SURFACE ( 3, 1, ( 
 ( #3855, #21117 ),
 ( #10061, #19385 ),
 ( #10355, #8460 ),
 ( #3985, #27595 ) ),
 .UNSPECIFIED., .F., .F., .F. ) 
 B_SPLINE_SURFACE_WITH_KNOTS ( ( 4, 4 ),
 ( 2, 2 ),
 ( 0.000000000000000000, 1.000000000000000000 ),
 ( 0.000000000000000000, 1.000000000000000000 ),
 .UNSPECIFIED. ) 
 GEOMETRIC_REPRESENTATION_ITEM ( )  RATIONAL_B_SPLINE_SURFACE ( (
 ( 1.000000000000000000, 1.000000000000000000),
 ( 0.9934239774497838349, 0.8357310067453913582),
 ( 0.9934239774497838349, 0.8357310067453913582),
 ( 1.000000000000000000, 1.000000000000000000) ) ) 
 REPRESENTATION_ITEM ( '' )  SURFACE ( )  );
#25074 = VERTEX_POINT ( 'NONE', #9469 ) ;
#25075 = CARTESIAN_POINT ( 'NONE',  ( 55.79472521941426777, -49.22042574086461997, 53.57698701322198076 ) ) ;
#25076 = CARTESIAN_POINT ( 'NONE',  ( -1.050230347699842248, -0.2550051351976088121, -45.79907861674080749 ) ) ;
#25077 = CARTESIAN_POINT ( 'NONE',  ( -1.619063947482197729, -25.20140673341401438, -38.92136151114898723 ) ) ;
#25078 = EDGE_CURVE ( 'NONE', #22323, #15612, #19402, .T. ) ;
#25079 = EDGE_CURVE ( 'NONE', #24828, #335, #27668, .T. ) ;
#25080 = CARTESIAN_POINT ( 'NONE',  ( -55.24198130335446422, 0.001516807524708540730, -0.009170435128245290474 ) ) ;
#25081 = DIRECTION ( 'NONE',  ( 1.000000000000000000, -6.938893903907226837E-18, 1.734723475976806709E-18 ) ) ;
#25082 = CARTESIAN_POINT ( 'NONE',  ( 25.64700659047694842, -107.4550658295753749, 34.67498789830411710 ) ) ;
#25084 = EDGE_CURVE ( 'NONE', #3139, #18502, #20778, .T. ) ;
#25083 = CARTESIAN_POINT ( 'NONE',  ( 1.833838850093465700, 145.1097630783160923, -3.453306173377954874E-06 ) ) ;
#25085 = ORIENTED_EDGE ( 'NONE', *, *, #16035, .F. ) ;
#25086 = EDGE_LOOP ( 'NONE', ( #18068, #12593, #13407, #7733 ) ) ;
#25087 = VERTEX_POINT ( 'NONE', #20392 ) ;
#25088 = CARTESIAN_POINT ( 'NONE',  ( 26.11404676487257603, -84.89295829319543429, 74.91683232330944975 ) ) ;
#25089 = CARTESIAN_POINT ( 'NONE',  ( 13.84597867724998288, 132.0026437215597355, 64.00674338125878648 ) ) ;
#25090 = CARTESIAN_POINT ( 'NONE',  ( 9.884929003653626367, 132.4189379373570432, 71.59798461011378379 ) ) ;
#25091 = CARTESIAN_POINT ( 'NONE',  ( 1.832998868059890096, -108.1944082009150634, -96.70023740551232549 ) ) ;
#25092 = CARTESIAN_POINT ( 'NONE',  ( -28.41354790283022069, -14.62505768302813713, -18.00456980371894744 ) ) ;
#25093 = CARTESIAN_POINT ( 'NONE',  ( 55.49584447822657296, -71.02133150427246733, -14.82242356768008662 ) ) ;
#25094 = CARTESIAN_POINT ( 'NONE',  ( 1.894214914920933079, -132.9862534094753528, -58.16536411968072429 ) ) ;
#25095 = CARTESIAN_POINT ( 'NONE',  ( 1.832998868059858122, 137.8420662456176160, -45.34898734665906517 ) ) ;
#25096 = CARTESIAN_POINT ( 'NONE',  ( 1.833206308920072081, -30.89799439741721798, 141.7818018507502416 ) ) ;
#25097 = CARTESIAN_POINT ( 'NONE',  ( -20.57838717382308502, 25.16001208503106668, -16.28767523336130196 ) ) ;
#25098 = FACE_OUTER_BOUND ( 'NONE', #18860, .T. ) ;
#25099 = CARTESIAN_POINT ( 'NONE',  ( 28.43349137099836810, -109.5743306972602511, -58.58376153369822248 ) ) ;
#25100 =( BOUNDED_SURFACE ( )  B_SPLINE_SURFACE ( 3, 1, ( 
 ( #2977, #11752 ),
 ( #665, #806 ),
 ( #4976, #15918 ),
 ( #5122, #13899 ) ),
 .UNSPECIFIED., .F., .F., .F. ) 
 B_SPLINE_SURFACE_WITH_KNOTS ( ( 4, 4 ),
 ( 2, 2 ),
 ( 0.000000000000000000, 1.000000000000000000 ),
 ( 0.000000000000000000, 1.000000000000000000 ),
 .UNSPECIFIED. ) 
 GEOMETRIC_REPRESENTATION_ITEM ( )  RATIONAL_B_SPLINE_SURFACE ( (
 ( 1.000000000000000000, 1.000000000000000000),
 ( 0.6386103224230316178, 0.9954351624131538845),
 ( 0.6386103224230316178, 0.9954351624131538845),
 ( 1.000000000000000000, 1.000000000000000000) ) ) 
 REPRESENTATION_ITEM ( '' )  SURFACE ( )  );
#25101 = EDGE_CURVE ( 'NONE', #207, #17966, #5170, .T. ) ;
#25102 = CARTESIAN_POINT ( 'NONE',  ( 13.36082413113063083, 41.18148072373809043, -147.2768864064163665 ) ) ;
#25103 = CARTESIAN_POINT ( 'NONE',  ( 26.11404676487256893, 1.130420376098718593, -113.2169081140373663 ) ) ;
#25104 = FACE_OUTER_BOUND ( 'NONE', #19858, .T. ) ;
#25105 = VERTEX_POINT ( 'NONE', #534 ) ;
#25106 = DIRECTION ( 'NONE',  ( -1.000000000000000000, -0.000000000000000000, -0.000000000000000000 ) ) ;
#25107 = ORIENTED_EDGE ( 'NONE', *, *, #8167, .F. ) ;
#25109 = EDGE_CURVE ( 'NONE', #6415, #18758, #18365, .T. ) ;
#25108 = CARTESIAN_POINT ( 'NONE',  ( 25.64681081121879203, 112.9102952884414464, 0.4157506337731812773 ) ) ;
#25110 = FACE_OUTER_BOUND ( 'NONE', #10060, .T. ) ;
#25111 = EDGE_LOOP ( 'NONE', ( #23990, #7851, #9971, #16190 ) ) ;
#25112 = EDGE_CURVE ( 'NONE', #20568, #17620, #4320, .T. ) ;
#25113 = B_SPLINE_CURVE_WITH_KNOTS ( 'NONE', 3,
 ( #12137, #1193, #16591, #18746, #27520, #7831, #21251, #10339, #14627, #25860 ),
 .UNSPECIFIED., .F., .F.,
 ( 4, 3, 3, 4 ),
 ( 1.387778780781445676E-17, 0.0002669560319015911202, 0.0005492286108966362495, 0.0008315040496093336220 ),
 .UNSPECIFIED. ) ;
#25114 = ORIENTED_EDGE ( 'NONE', *, *, #4811, .T. ) ;
#25115 = EDGE_LOOP ( 'NONE', ( #6956, #25768, #27193, #23125 ) ) ;
#25116 = EDGE_LOOP ( 'NONE', ( #16436, #23300, #28341, #14837 ) ) ;
#25117 = CARTESIAN_POINT ( 'NONE',  ( -1.239374126674604337, 11.92219841463829333, -44.48112152129351671 ) ) ;
#25118 = DIRECTION ( 'NONE',  ( -0.000000000000000000, 1.000000000000000000, 0.000000000000000000 ) ) ;
#25119 = CARTESIAN_POINT ( 'NONE',  ( -20.20700224038492721, -18.19058640100206503, 23.35150625415678860 ) ) ;
#25120 = CARTESIAN_POINT ( 'NONE',  ( 25.64700659047697684, -66.55152787776188461, 91.21315746821495907 ) ) ;
#25121 = CARTESIAN_POINT ( 'NONE',  ( -1.155031165708883867, -2.068616213631259804, -45.85732438018710155 ) ) ;
#25122 = FACE_OUTER_BOUND ( 'NONE', #543, .T. ) ;
#25123 = CARTESIAN_POINT ( 'NONE',  ( 25.64681081121879203, 75.24277141833491100, 84.18689316040072868 ) ) ;
#25124 = B_SPLINE_CURVE_WITH_KNOTS ( 'NONE', 3,
 ( #27625, #23335, #17108, #16705, #3734, #12503 ),
 .UNSPECIFIED., .F., .F.,
 ( 4, 2, 4 ),
 ( 1.396102177145585797E-16, 0.003570751334075633089, 0.007141502668151126533 ),
 .UNSPECIFIED. ) ;
#25125 = CARTESIAN_POINT ( 'NONE',  ( -20.21097721650786738, 17.67178726257392896, 23.76068422213738529 ) ) ;
#25126 = CARTESIAN_POINT ( 'NONE',  ( -20.57838717382308147, -7.715628353033481268, 28.96176188950225949 ) ) ;
#25127 = CARTESIAN_POINT ( 'NONE',  ( 1.832998868059890096, -97.49378069860723883, -107.4798986104869982 ) ) ;
#25128 = VERTEX_POINT ( 'NONE', #4714 ) ;
#25129 = ORIENTED_EDGE ( 'NONE', *, *, #24288, .F. ) ;
#25130 = CARTESIAN_POINT ( 'NONE',  ( 109.1586900883932856, 0.007002774699553638779, 0.001385221016527484091 ) ) ;
#25132 = CARTESIAN_POINT ( 'NONE',  ( 25.86096068574581253, 76.38617895399458746, -83.34468010038209229 ) ) ;
#25131 = DIRECTION ( 'NONE',  ( 0.000000000000000000, 0.000000000000000000, 1.000000000000000000 ) ) ;
#25133 = EDGE_CURVE ( 'NONE', #14003, #8000, #13489, .T. ) ;
#25134 = CARTESIAN_POINT ( 'NONE',  ( -4.178947244162639407, -18.28784278438482858, -45.38689110596713050 ) ) ;
#25135 = CARTESIAN_POINT ( 'NONE',  ( 1.833485406944043827, 85.72460230293692973, 117.0814567582547596 ) ) ;
#25136 = CARTESIAN_POINT ( 'NONE',  ( 2.108393763691185363, -71.53437599919723766, -126.4628696952926958 ) ) ;
#25137 = ORIENTED_EDGE ( 'NONE', *, *, #12265, .F. ) ;
#25138 = CARTESIAN_POINT ( 'NONE',  ( -22.34422965417122242, 27.39717383755282043, -26.20925041532862920 ) ) ;
#25140 = EDGE_CURVE ( 'NONE', #5543, #19578, #9172, .T. ) ;
#25139 = CARTESIAN_POINT ( 'NONE',  ( -1.323830074806772394, 35.86387698262958423, 28.92190886481825274 ) ) ;
#25141 = CARTESIAN_POINT ( 'NONE',  ( 1.833485406944043827, -14.63699153649458040, 144.3694338680884641 ) ) ;
#25142 = VERTEX_POINT ( 'NONE', #14484 ) ;
#25143 = CARTESIAN_POINT ( 'NONE',  ( 25.64704443564078673, -97.85065179540796976, 56.33997466860367354 ) ) ;
#25144 = CARTESIAN_POINT ( 'NONE',  ( -1.259972190295303385, -16.33417789844404666, -43.01178231151323672 ) ) ;
#25145 =( BOUNDED_SURFACE ( )  B_SPLINE_SURFACE ( 3, 1, ( 
 ( #6012, #14768 ),
 ( #1944, #12743 ),
 ( #1534, #3839 ),
 ( #7898, #6158 ) ),
 .UNSPECIFIED., .F., .F., .F. ) 
 B_SPLINE_SURFACE_WITH_KNOTS ( ( 4, 4 ),
 ( 2, 2 ),
 ( 0.000000000000000000, 1.000000000000000000 ),
 ( 0.000000000000000000, 1.000000000000000000 ),
 .UNSPECIFIED. ) 
 GEOMETRIC_REPRESENTATION_ITEM ( )  RATIONAL_B_SPLINE_SURFACE ( (
 ( 1.000000000000000000, 1.000000000000000000),
 ( 0.6386103224230316178, 0.9954351624131538845),
 ( 0.6386103224230316178, 0.9954351624131538845),
 ( 1.000000000000000000, 1.000000000000000000) ) ) 
 REPRESENTATION_ITEM ( '' )  SURFACE ( )  );
#25146 = EDGE_LOOP ( 'NONE', ( #26644, #14993, #7933, #13871 ) ) ;
#25147 = LINE ( 'NONE', #27286, #11976 ) ;
#25148 = ORIENTED_EDGE ( 'NONE', *, *, #27628, .F. ) ;
#25149 = CARTESIAN_POINT ( 'NONE',  ( 25.70243777736189372, -45.26941207740225082, -103.4793210720852983 ) ) ;
#25150 = CARTESIAN_POINT ( 'NONE',  ( 6.224689322667630975, -118.2566963816764911, -89.08920297664333532 ) ) ;
#25151 = VERTEX_POINT ( 'NONE', #10193 ) ;
#25152 = B_SPLINE_CURVE_WITH_KNOTS ( 'NONE', 3,
 ( #25965, #6388, #13417, #13137, #24239, #19616, #28245, #26377, #43, #8683 ),
 .UNSPECIFIED., .F., .F.,
 ( 4, 3, 3, 4 ),
 ( 6.938893903907228378E-18, 0.0002669560319015750198, 0.0005492286108966477421, 0.0008315040496093457651 ),
 .UNSPECIFIED. ) ;
#25153 = APPLICATION_PROTOCOL_DEFINITION ( 'draft international standard', 'automotive_design', 1998, #16352 ) ;
#25154 = CARTESIAN_POINT ( 'NONE',  ( 0.000000000000000000, 1.806757805586603712E-14, 143.8872038478949946 ) ) ;
#25155 = CARTESIAN_POINT ( 'NONE',  ( 1.833206310202334377, -117.8322271314358716, -84.68961945193576923 ) ) ;
#25156 = CARTESIAN_POINT ( 'NONE',  ( 2.433796855181205476, -13.76554153471595043, -144.8571464219890572 ) ) ;
#25157 = CARTESIAN_POINT ( 'NONE',  ( -20.21097721650786383, 28.05863614620939472, -9.464413208035171721 ) ) ;
#25158 = ORIENTED_EDGE ( 'NONE', *, *, #27106, .T. ) ;
#25159 = ADVANCED_FACE ( 'NONE', ( #7897 ), #24173, .F. ) ;
#25160 = CARTESIAN_POINT ( 'NONE',  ( 32.73300124599737160, -108.9684813982492244, 44.31599526637918274 ) ) ;
#25161 = CARTESIAN_POINT ( 'NONE',  ( 13.36082413113063083, -143.3553710183992962, 53.25066407421756054 ) ) ;
#25162 = CARTESIAN_POINT ( 'NONE',  ( 1.834118845439484335, 141.9019470378991343, -30.34413640949558655 ) ) ;
#25163 = ORIENTED_EDGE ( 'NONE', *, *, #3907, .F. ) ;
#25164 = EDGE_CURVE ( 'NONE', #15699, #8105, #9106, .T. ) ;
#25165 = VERTEX_POINT ( 'NONE', #27440 ) ;
#25166 = ORIENTED_EDGE ( 'NONE', *, *, #3641, .T. ) ;
#25167 = CARTESIAN_POINT ( 'NONE',  ( -7.078251931573406708, -50.86685171665420313, -11.16394717458656949 ) ) ;
#25168 = CARTESIAN_POINT ( 'NONE',  ( 16.75465622695673673, 79.80233222761980016, 117.7275519421676506 ) ) ;
#25170 = DIRECTION ( 'NONE',  ( -1.000000000000000000, -0.000000000000000000, -0.000000000000000000 ) ) ;
#25169 = CARTESIAN_POINT ( 'NONE',  ( 6.224689322667647851, -76.23997225729179661, -126.9212313063852662 ) ) ;
#25171 = ADVANCED_FACE ( 'NONE', ( #18527 ), #11296, .F. ) ;
#25172 = CARTESIAN_POINT ( 'NONE',  ( 8.186469777910918566, -3.468244369820856932, -149.3111477498017905 ) ) ;
#25173 = CARTESIAN_POINT ( 'NONE',  ( 1.833838850093477912, -132.5643663243753281, -59.02145475724777413 ) ) ;
#25174 = CARTESIAN_POINT ( 'NONE',  ( -20.24419206586952313, -18.44224248888889051, -23.20105925399719382 ) ) ;
#25175 = ORIENTED_EDGE ( 'NONE', *, *, #24634, .T. ) ;
#25176 = CARTESIAN_POINT ( 'NONE',  ( 26.11404676487257603, 98.61392875273364211, 55.62948129436280453 ) ) ;
#25177 = CARTESIAN_POINT ( 'NONE',  ( 2.063896406836605024, 43.61045647697694250, 138.5688025270880246 ) ) ;
#25178 = CARTESIAN_POINT ( 'NONE',  ( -20.57838717382308147, 28.96176188950229502, 7.715628353033378239 ) ) ;
#25179 = CARTESIAN_POINT ( 'NONE',  ( -8.786685647604885574, 6.096987947571466530E-17, -1.524246986892866633E-17 ) ) ;
#25180 = CARTESIAN_POINT ( 'NONE',  ( 25.64692232868534560, 107.4854307433087257, 34.58055111992081265 ) ) ;
#25181 = CARTESIAN_POINT ( 'NONE',  ( -1.045287976400365970, -45.76855895860942525, 1.530335034934587002 ) ) ;
#25182 = CARTESIAN_POINT ( 'NONE',  ( 1.832998868059858122, -144.2584710144579390, -15.69902610990523151 ) ) ;
#25183 = ORIENTED_EDGE ( 'NONE', *, *, #5496, .T. ) ;
#25184 = CARTESIAN_POINT ( 'NONE',  ( 1.832998868059890096, 58.53348008137826497, -132.7810136645732371 ) ) ;
#25185 = CARTESIAN_POINT ( 'NONE',  ( 1.833750490713643266, -29.90883416717514010, -141.9939712933759211 ) ) ;
#25186 = CARTESIAN_POINT ( 'NONE',  ( 109.1589550718175161, 0.001354998915253774082, -0.007453082872782202176 ) ) ;
#25187 = ORIENTED_EDGE ( 'NONE', *, *, #1971, .F. ) ;
#25188 = ORIENTED_EDGE ( 'NONE', *, *, #17337, .F. ) ;
#25189 = CARTESIAN_POINT ( 'NONE',  ( -1.048171036023513025, 45.78635789057865679, 1.020520027229292470 ) ) ;
#25190 = CARTESIAN_POINT ( 'NONE',  ( -1.046936909428682450, -43.93225665392624535, -12.93351869073256388 ) ) ;
#25191 = CARTESIAN_POINT ( 'NONE',  ( 109.1587776205901577, -0.003592288931009647752, -0.006388631651928880321 ) ) ;
#25192 = EDGE_CURVE ( 'NONE', #7808, #25689, #12864, .T. ) ;
#25193 = CARTESIAN_POINT ( 'NONE',  ( 10.93730112725996051, 20.69552240458543224, -149.7554878793147282 ) ) ;
#25194 = VERTEX_POINT ( 'NONE', #14337 ) ;
#25195 = CARTESIAN_POINT ( 'NONE',  ( 28.37603512858456156, -55.80522682147343261, 100.2461737936628765 ) ) ;
#25196 = CARTESIAN_POINT ( 'NONE',  ( 1.833838850855499025, 44.92600961247843827, -137.9800888515318320 ) ) ;
#25197 = EDGE_CURVE ( 'NONE', #28149, #26886, #23156, .T. ) ;
#25198 = CARTESIAN_POINT ( 'NONE',  ( -28.13707043255157103, 18.96624908365864925, 12.83104814250432923 ) ) ;
#25199 = ORIENTED_EDGE ( 'NONE', *, *, #25638, .F. ) ;
#25200 = ADVANCED_FACE ( 'NONE', ( #20959 ), #28128, .T. ) ;
#25201 = EDGE_LOOP ( 'NONE', ( #276, #27176, #13967, #2147 ) ) ;
#25202 = CARTESIAN_POINT ( 'NONE',  ( -7.078251931573400491, -20.86696228105191864, 47.71415099571825635 ) ) ;
#25203 = CARTESIAN_POINT ( 'NONE',  ( 28.43349137099834678, -69.71646995966243310, 102.8504004831932832 ) ) ;
#25204 = DIRECTION ( 'NONE',  ( 0.000000000000000000, 0.000000000000000000, 1.000000000000000000 ) ) ;
#25205 = CARTESIAN_POINT ( 'NONE',  ( 55.49584447822657296, -36.50733923851242935, 62.69727227546388804 ) ) ;
#25206 = CARTESIAN_POINT ( 'NONE',  ( 1.832998868059890096, -107.4798986104866572, 97.49378069860762253 ) ) ;
#25207 = CARTESIAN_POINT ( 'NONE',  ( -1.619063947482197729, 2.489035965910159298, -46.30105812165548684 ) ) ;
#25208 = CARTESIAN_POINT ( 'NONE',  ( 32.73300124599732186, 0.000000000000000000, 0.000000000000000000 ) ) ;
#25209 = ORIENTED_EDGE ( 'NONE', *, *, #27996, .T. ) ;
#25210 = DIRECTION ( 'NONE',  ( -0.7563875759206388771, -0.2351350468682952832, -0.6104009704506900835 ) ) ;
#25211 = DIRECTION ( 'NONE',  ( -1.000000000000000000, -0.000000000000000000, -0.000000000000000000 ) ) ;
#25212 = CARTESIAN_POINT ( 'NONE',  ( 25.98107933586710772, -10.73978443746659295, -112.6229961579377203 ) ) ;
#25213 = B_SPLINE_CURVE_WITH_KNOTS ( 'NONE', 3,
 ( #25846, #6272, #22077, #13016, #6548, #28262, #25982 ),
 .UNSPECIFIED., .F., .F.,
 ( 4, 3, 4 ),
 ( 6.557988972572477070E-16, 0.02816610861753243711, 0.04000277880656291640 ),
 .UNSPECIFIED. ) ;
#25214 = CARTESIAN_POINT ( 'NONE',  ( 109.1587776205901577, 0.004965871434389453401, -0.005390665547499381982 ) ) ;
#25215 = ORIENTED_EDGE ( 'NONE', *, *, #1473, .F. ) ;
#25216 = CARTESIAN_POINT ( 'NONE',  ( 25.98552792386799837, -57.50018541500355695, -97.43552975939674354 ) ) ;
#25217 = DIRECTION ( 'NONE',  ( 0.7637818620346801257, 0.1788995134688915190, 0.6201872550346635427 ) ) ;
#25218 = VERTEX_POINT ( 'NONE', #8169 ) ;
#25219 = VECTOR ( 'NONE', #19580, 1000.000000000000114 ) ;
#25220 = ORIENTED_EDGE ( 'NONE', *, *, #18998, .T. ) ;
#25221 = CIRCLE ( 'NONE', #27018, 34.60786435723138510 ) ;
#25222 = ORIENTED_EDGE ( 'NONE', *, *, #11835, .F. ) ;
#25223 = CARTESIAN_POINT ( 'NONE',  ( -1.583189561560252701, -25.21827308671259615, -38.94740041318285506 ) ) ;
#25224 = DIRECTION ( 'NONE',  ( 0.000000000000000000, 0.000000000000000000, 1.000000000000000000 ) ) ;
#25225 = EDGE_CURVE ( 'NONE', #25959, #6949, #1245, .T. ) ;
#25226 = B_SPLINE_CURVE_WITH_KNOTS ( 'NONE', 3,
 ( #20465, #891, #9677, #3060, #16293, #25089, #1041 ),
 .UNSPECIFIED., .F., .F.,
 ( 4, 3, 4 ),
 ( 0.000000000000000000, 0.02398743853561325495, 0.04000277880656212537 ),
 .UNSPECIFIED. ) ;
#25227 = ADVANCED_FACE ( 'NONE', ( #12323 ), #13473, .F. ) ;
#25228 = CARTESIAN_POINT ( 'NONE',  ( 2.430230287190592531, -107.1617224697470903, 98.44218333480735339 ) ) ;
#25229 = B_SPLINE_CURVE_WITH_KNOTS ( 'NONE', 3,
 ( #25003, #26976, #20648, #1223, #3388, #16048, #940, #9729, #20936, #18064 ),
 .UNSPECIFIED., .F., .F.,
 ( 4, 3, 3, 4 ),
 ( 1.387778780781445676E-17, 0.0002669560319015871629, 0.0005492286108966491515, 0.0008315040496093398020 ),
 .UNSPECIFIED. ) ;
#25230 = CARTESIAN_POINT ( 'NONE',  ( -1.619063947482197729, 25.20140673341430571, 38.92136151114879539 ) ) ;
#25231 =( BOUNDED_SURFACE ( )  B_SPLINE_SURFACE ( 3, 1, ( 
 ( #24595, #16358 ),
 ( #13910, #25150 ),
 ( #22278, #11466 ),
 ( #20389, #2539 ) ),
 .UNSPECIFIED., .F., .F., .F. ) 
 B_SPLINE_SURFACE_WITH_KNOTS ( ( 4, 4 ),
 ( 2, 2 ),
 ( 0.000000000000000000, 1.000000000000000000 ),
 ( 0.000000000000000000, 1.000000000000000000 ),
 .UNSPECIFIED. ) 
 GEOMETRIC_REPRESENTATION_ITEM ( )  RATIONAL_B_SPLINE_SURFACE ( (
 ( 1.000000000000000000, 1.000000000000000000),
 ( 0.6386103224230302855, 0.9954351624131538845),
 ( 0.6386103224230302855, 0.9954351624131538845),
 ( 1.000000000000000000, 1.000000000000000000) ) ) 
 REPRESENTATION_ITEM ( '' )  SURFACE ( )  );
#25232 = CARTESIAN_POINT ( 'NONE',  ( -1.045287976400365970, 1.530335034934747318, 45.76855895860941814 ) ) ;
#25233 = EDGE_CURVE ( 'NONE', #12213, #25254, #25944, .T. ) ;
#25234 = DIRECTION ( 'NONE',  ( -0.5946245182733607137, -0.7870422510449642806, -0.1642747008466272085 ) ) ;
#25235 = CARTESIAN_POINT ( 'NONE',  ( -1.259972190295296057, 45.95417440459617353, -2.243354636025928439 ) ) ;
#25236 = B_SPLINE_CURVE_WITH_KNOTS ( 'NONE', 3,
 ( #10571, #6937, #2297, #11524, #21500, #588, #9229 ),
 .UNSPECIFIED., .F., .F.,
 ( 4, 3, 4 ),
 ( 4.730677113667733359E-16, 0.02816610861753244058, 0.04000277880656269436 ),
 .UNSPECIFIED. ) ;
#25237 = VECTOR ( 'NONE', #14432, 1000.000000000000114 ) ;
#25238 = ADVANCED_FACE ( 'NONE', ( #11023 ), #27082, .F. ) ;
#25239 = CARTESIAN_POINT ( 'NONE',  ( -25.21435515916043002, 31.17620025257588523, -15.02493970636157705 ) ) ;
#25240 = CARTESIAN_POINT ( 'NONE',  ( -25.21435515916043713, 16.39063784838786475, 30.48034229288620622 ) ) ;
#25241 = CARTESIAN_POINT ( 'NONE',  ( -20.20700224038492721, 18.19058640100257662, 23.35150625415638714 ) ) ;
#25242 = CIRCLE ( 'NONE', #2209, 117.6351876552689504 ) ;
#25243 = DIRECTION ( 'NONE',  ( 0.5946245182733607137, 0.7992853357633866729, 0.08697490616139734454 ) ) ;
#25244 = LINE ( 'NONE', #764, #21990 ) ;
#25245 = CARTESIAN_POINT ( 'NONE',  ( -28.13707043255157103, -7.802116958609158992, -21.52861750560936471 ) ) ;
#25246 = CARTESIAN_POINT ( 'NONE',  ( -55.24271866751342941, 0.008433070970614320663, 0.004365563123939306990 ) ) ;
#25247 = CARTESIAN_POINT ( 'NONE',  ( 13.36082413113061307, -106.9547846563642963, 109.3026516754228794 ) ) ;
#25248 = CARTESIAN_POINT ( 'NONE',  ( 2.108985857320894386, -107.1123114102935006, 98.16869034643272585 ) ) ;
#25249 = ORIENTED_EDGE ( 'NONE', *, *, #26965, .F. ) ;
#25250 = DIRECTION ( 'NONE',  ( 0.000000000000000000, 0.000000000000000000, 1.000000000000000000 ) ) ;
#25251 = ORIENTED_EDGE ( 'NONE', *, *, #21968, .T. ) ;
#25252 = CARTESIAN_POINT ( 'NONE',  ( 2.108985857320888169, -16.46110181986589183, -144.3577886602088256 ) ) ;
#25253 = DIRECTION ( 'NONE',  ( 0.000000000000000000, 5.223019709708116647E-21, -1.000000000000000000 ) ) ;
#25254 = VERTEX_POINT ( 'NONE', #15320 ) ;
#25255 = ORIENTED_EDGE ( 'NONE', *, *, #15511, .F. ) ;
#25256 = ORIENTED_EDGE ( 'NONE', *, *, #19568, .T. ) ;
#25257 = CARTESIAN_POINT ( 'NONE',  ( 28.37599760073042177, -114.7183216384031397, -1.794331790580630637 ) ) ;
#25258 = ADVANCED_FACE ( 'NONE', ( #1797 ), #18258, .F. ) ;
#25259 = CARTESIAN_POINT ( 'NONE',  ( 2.063896406836605024, -16.52087515463875178, 144.3268707900446657 ) ) ;
#25260 = B_SPLINE_CURVE_WITH_KNOTS ( 'NONE', 3,
 ( #17231, #10770, #8598, #15195 ),
 .UNSPECIFIED., .F., .F.,
 ( 4, 4 ),
 ( 0.000000000000000000, 0.01077107196513874682 ),
 .UNSPECIFIED. ) ;
#25261 = CARTESIAN_POINT ( 'NONE',  ( -1.031422197589711764, 44.01264471863847660, -12.69107518035516691 ) ) ;
#25262 =( BOUNDED_SURFACE ( )  B_SPLINE_SURFACE ( 3, 1, ( 
 ( #28196, #16984 ),
 ( #21584, #4026 ),
 ( #5924, #8092 ),
 ( #12796, #23636 ) ),
 .UNSPECIFIED., .F., .F., .F. ) 
 B_SPLINE_SURFACE_WITH_KNOTS ( ( 4, 4 ),
 ( 2, 2 ),
 ( 0.000000000000000000, 1.000000000000000000 ),
 ( 0.000000000000000000, 1.000000000000000000 ),
 .UNSPECIFIED. ) 
 GEOMETRIC_REPRESENTATION_ITEM ( )  RATIONAL_B_SPLINE_SURFACE ( (
 ( 1.000000000000000000, 1.000000000000000000),
 ( 0.9956975270656955868, 0.8568959468854907557),
 ( 0.9956975270656955868, 0.8568959468854907557),
 ( 1.000000000000000000, 1.000000000000000000) ) ) 
 REPRESENTATION_ITEM ( '' )  SURFACE ( )  );
#25263 = DIRECTION ( 'NONE',  ( 1.000000000000000000, 0.000000000000000000, 0.000000000000000000 ) ) ;
#25264 = ADVANCED_FACE ( 'NONE', ( #26129 ), #28187, .F. ) ;
#25265 = CARTESIAN_POINT ( 'NONE',  ( 6.224689322667647851, 62.55544044765247236, 134.1951906609240837 ) ) ;
#25266 = CARTESIAN_POINT ( 'NONE',  ( 32.73300124599735739, -99.90245962373877830, 62.10906484417201767 ) ) ;
#25267 = CARTESIAN_POINT ( 'NONE',  ( -55.24340739397742794, 0.003826481709800397344, 0.009386184976285138343 ) ) ;
#25268 = CARTESIAN_POINT ( 'NONE',  ( 1.833838850855462388, -58.94016894581382360, -132.6005571022085689 ) ) ;
#25269 = CARTESIAN_POINT ( 'NONE',  ( 1.832998868059890096, 58.53348008137649572, 132.7810136645739760 ) ) ;
#25270 = CARTESIAN_POINT ( 'NONE',  ( 180.4657679828686980, 20.00000000000000000, 2.618615375249201539E-15 ) ) ;
#25271 = VERTEX_POINT ( 'NONE', #21954 ) ;
#25272 = ORIENTED_EDGE ( 'NONE', *, *, #12188, .T. ) ;
#25273 = CARTESIAN_POINT ( 'NONE',  ( 10.93730112725990189, -97.44200844886194091, -115.5857507957714461 ) ) ;
#25275 = CARTESIAN_POINT ( 'NONE',  ( -24.53237795827023859, 6.738475012720130941, -33.25734978085264260 ) ) ;
#25274 = CARTESIAN_POINT ( 'NONE',  ( 1.833838850093464812, 85.29338149487213627, 117.3962623502777092 ) ) ;
#25276 = CARTESIAN_POINT ( 'NONE',  ( -20.24399999263415140, -7.930419334766389383, -28.55700515887716762 ) ) ;
#25277 =( LENGTH_UNIT ( ) NAMED_UNIT ( * ) SI_UNIT ( .MILLI., .METRE. ) );
#25278 = CARTESIAN_POINT ( 'NONE',  ( -1.113548883309550153, -35.91246368318222437, -28.52482525634933097 ) ) ;
#25279 = ORIENTED_EDGE ( 'NONE', *, *, #14289, .F. ) ;
#25280 = CARTESIAN_POINT ( 'NONE',  ( 109.1589550718175161, -0.001014448720249593950, -0.007507020724820351841 ) ) ;
#25281 = CARTESIAN_POINT ( 'NONE',  ( -8.786685647604887350, 53.04920435127183254, 7.199674155859139724 ) ) ;
#25282 = CARTESIAN_POINT ( 'NONE',  ( 21.16825799904935934, 133.3214686481432807, 23.82367662027858302 ) ) ;
#25283 = ORIENTED_EDGE ( 'NONE', *, *, #17705, .T. ) ;
#25284 = CARTESIAN_POINT ( 'NONE',  ( 13.36082413113061307, -150.7747251079863702, 25.56125765253402449 ) ) ;
#25285 = CARTESIAN_POINT ( 'NONE',  ( -1.539760825549682410, -29.16712717142786460, -35.94320866319479535 ) ) ;
#25286 = ORIENTED_EDGE ( 'NONE', *, *, #7410, .T. ) ;
#25287 = ORIENTED_EDGE ( 'NONE', *, *, #15140, .F. ) ;
#25288 = ORIENTED_EDGE ( 'NONE', *, *, #2121, .T. ) ;
#25289 = DIRECTION ( 'NONE',  ( 0.7563875759206388771, -0.3556158456312938365, -0.5490129373055243622 ) ) ;
#25290 = CARTESIAN_POINT ( 'NONE',  ( -20.20700224038492010, 18.19058640100223556, -23.35150625415664649 ) ) ;
#25291 = EDGE_CURVE ( 'NONE', #5142, #119, #11500, .T. ) ;
#25292 = VERTEX_POINT ( 'NONE', #14903 ) ;
#25293 = AXIS2_PLACEMENT_3D ( 'NONE', #16466, #22530, #2800 ) ;
#25294 = APPLICATION_PROTOCOL_DEFINITION ( 'draft international standard', 'automotive_design', 1998, #28110 ) ;
#25295 = CARTESIAN_POINT ( 'NONE',  ( -1.113427685306998649, -44.18561238466747199, -12.28784199929917875 ) ) ;
#25296 = EDGE_CURVE ( 'NONE', #4923, #5291, #11596, .T. ) ;
#25297 = CARTESIAN_POINT ( 'NONE',  ( -55.24390624410018802, 0.001811362924359719581, 0.01027195578987765215 ) ) ;
#25298 = CARTESIAN_POINT ( 'NONE',  ( 10.93730112725932635, 149.7554878793145576, 20.69552240458357062 ) ) ;
#25299 = ADVANCED_FACE ( 'NONE', ( #8575 ), #3404, .F. ) ;
#25300 = ORIENTED_EDGE ( 'NONE', *, *, #17061, .T. ) ;
#25301 = CARTESIAN_POINT ( 'NONE',  ( -55.24728320129491266, 0.0006547948648740692726, 0.01453410071985259712 ) ) ;
#25303 = CARTESIAN_POINT ( 'NONE',  ( 109.1586900883932856, 0.0001010081143884183533, -0.007137750914552287197 ) ) ;
#25302 = CARTESIAN_POINT ( 'NONE',  ( 55.49584447822657296, -72.18163437663935156, -7.317474139116371568 ) ) ;
#25304 = CARTESIAN_POINT ( 'NONE',  ( 25.73574536432416338, -102.8730547980546959, -46.68445899255593901 ) ) ;
#25305 = VERTEX_POINT ( 'NONE', #19509 ) ;
#25306 = ORIENTED_EDGE ( 'NONE', *, *, #6891, .F. ) ;
#25307 = ORIENTED_EDGE ( 'NONE', *, *, #18310, .T. ) ;
#25308 = CARTESIAN_POINT ( 'NONE',  ( -6.574463467970653952, -51.07975593197902953, 5.014313797967556496 ) ) ;
#25309 = CARTESIAN_POINT ( 'NONE',  ( 55.49584447822657296, -29.75369869230911135, -66.16986612640803855 ) ) ;
#25311 = CARTESIAN_POINT ( 'NONE',  ( -21.41427618760447515, -7.777551129310266376, -29.81030852927063890 ) ) ;
#25310 = CARTESIAN_POINT ( 'NONE',  ( 109.1587776205901577, 0.001605238040359037010, -0.007151389024634743213 ) ) ;
#25312 = CARTESIAN_POINT ( 'NONE',  ( 1.894214914920946624, 132.9862534094756938, 58.16536411967987164 ) ) ;
#25313 = CARTESIAN_POINT ( 'NONE',  ( -12.94347594948484037, 33.69581619287875895, -35.22469990145616237 ) ) ;
#25314 = VERTEX_POINT ( 'NONE', #13032 ) ;
#25315 = CARTESIAN_POINT ( 'NONE',  ( 1.833485406944043827, 107.4794113447409529, 97.49333871408727248 ) ) ;
#25316 =( BOUNDED_SURFACE ( )  B_SPLINE_SURFACE ( 3, 1, ( 
 ( #1464, #14560 ),
 ( #14842, #27939 ),
 ( #3477, #23654 ),
 ( #27811, #12538 ) ),
 .UNSPECIFIED., .F., .F., .F. ) 
 B_SPLINE_SURFACE_WITH_KNOTS ( ( 4, 4 ),
 ( 2, 2 ),
 ( 0.000000000000000000, 1.000000000000000000 ),
 ( 0.000000000000000000, 1.000000000000000000 ),
 .UNSPECIFIED. ) 
 GEOMETRIC_REPRESENTATION_ITEM ( )  RATIONAL_B_SPLINE_SURFACE ( (
 ( 1.000000000000000000, 1.000000000000000000),
 ( 0.9956975270656954757, 0.8568959468854893125),
 ( 0.9956975270656954757, 0.8568959468854893125),
 ( 1.000000000000000000, 1.000000000000000000) ) ) 
 REPRESENTATION_ITEM ( '' )  SURFACE ( )  );
#25317 = DIRECTION ( 'NONE',  ( 1.000000000000000000, 0.000000000000000000, 0.000000000000000000 ) ) ;
#25318 = ORIENTED_EDGE ( 'NONE', *, *, #5169, .F. ) ;
#25319 = CARTESIAN_POINT ( 'NONE',  ( 5.340103579038253834, -135.6222865281525571, -57.86178752084628485 ) ) ;
#25320 = CARTESIAN_POINT ( 'NONE',  ( 26.11404676487257603, 92.25884714080409310, 65.63269960453273200 ) ) ;
#25321 = CARTESIAN_POINT ( 'NONE',  ( -1.049817751779893227, 14.63752841325048237, -43.39729912094385611 ) ) ;
#25322 = CARTESIAN_POINT ( 'NONE',  ( 1.834118845439484335, 85.43746956710005236, -117.2918069668792498 ) ) ;
#25323 = VECTOR ( 'NONE', #25643, 1000.000000000000000 ) ;
#25325 = CIRCLE ( 'NONE', #40, 28.92774122539760384 ) ;
#25324 = CARTESIAN_POINT ( 'NONE',  ( -1.619063947482201282, 38.92136151114908671, -25.20140673341387227 ) ) ;
#25326 = DIRECTION ( 'NONE',  ( 1.000000000000000000, -0.000000000000000000, -0.000000000000000000 ) ) ;
#25327 = VECTOR ( 'NONE', #14268, 1000.000000000000000 ) ;
#25328 = ORIENTED_EDGE ( 'NONE', *, *, #24976, .F. ) ;
#25329 = CARTESIAN_POINT ( 'NONE',  ( -1.239374126674604337, -28.97829083655465254, -35.79060836339803586 ) ) ;
#25330 = ADVANCED_FACE ( 'NONE', ( #28276 ), #1491, .T. ) ;
#25331 = VECTOR ( 'NONE', #9212, 1000.000000000000000 ) ;
#25332 = DIRECTION ( 'NONE',  ( 1.000000000000000000, -6.938893903907226837E-18, 1.734723475976806709E-18 ) ) ;
#25333 = CARTESIAN_POINT ( 'NONE',  ( -55.24728320129491266, 0.0006547948648751116246, -0.01453410071985669280 ) ) ;
#25334 = ORIENTED_EDGE ( 'NONE', *, *, #8489, .T. ) ;
#25335 = ADVANCED_FACE ( 'NONE', ( #26836 ), #450, .F. ) ;
#25336 = CARTESIAN_POINT ( 'NONE',  ( -1.056502255334264895, 14.64009593116162478, 43.40574022158757828 ) ) ;
#25337 = B_SPLINE_CURVE_WITH_KNOTS ( 'NONE', 3,
 ( #4939, #4503, #2337, #476 ),
 .UNSPECIFIED., .F., .F.,
 ( 4, 4 ),
 ( 1.962615573354718958E-17, 0.008383560773332745034 ),
 .UNSPECIFIED. ) ;
#25338 = ORIENTED_EDGE ( 'NONE', *, *, #21125, .F. ) ;
#25339 = EDGE_CURVE ( 'NONE', #10065, #9585, #22528, .T. ) ;
#25340 = CARTESIAN_POINT ( 'NONE',  ( -1.050229599974477068, 45.79907399707867199, 0.2556477501661113538 ) ) ;
#25341 = CARTESIAN_POINT ( 'NONE',  ( -1.050231094221214301, -43.63617436699747287, -13.91061116148175536 ) ) ;
#25342 = CARTESIAN_POINT ( 'NONE',  ( -25.21435515916043002, 4.655591116594353984, -34.29329011225956947 ) ) ;
#25343 = AXIS2_PLACEMENT_3D ( 'NONE', #11795, #8957, #5306 ) ;
#25345 = AXIS2_PLACEMENT_3D ( 'NONE', #19989, #26600, #24900 ) ;
#25344 = CARTESIAN_POINT ( 'NONE',  ( 6.224689322667647851, -148.0369967195763081, 2.565137105443233700 ) ) ;
#25346 = LINE ( 'NONE', #23620, #27342 ) ;
#25347 = B_SPLINE_CURVE_WITH_KNOTS ( 'NONE', 3,
 ( #6069, #17395, #1719, #10516 ),
 .UNSPECIFIED., .F., .F.,
 ( 4, 4 ),
 ( 2.238801616996865814E-16, 0.008383748772659661841 ),
 .UNSPECIFIED. ) ;
#25348 = B_SPLINE_CURVE_WITH_KNOTS ( 'NONE', 3,
 ( #14820, #15085, #8361, #23905, #22001, #4022, #15369, #25915 ),
 .UNSPECIFIED., .F., .F.,
 ( 4, 2, 2, 4 ),
 ( 0.000000000000000000, 0.002761524886576646742, 0.005523049773153293485, 0.01104609954630660605 ),
 .UNSPECIFIED. ) ;
#25349 = CARTESIAN_POINT ( 'NONE',  ( 1.833603222531973387, -125.4455769441937605, -72.93978951866115779 ) ) ;
#25350 = CARTESIAN_POINT ( 'NONE',  ( 1.833206310202335265, 97.64934828277093004, 107.3376456496884401 ) ) ;
#25351 = CARTESIAN_POINT ( 'NONE',  ( 25.81918753295380142, -45.11728622333212968, 103.6306245682013696 ) ) ;
#25352 = VECTOR ( 'NONE', #25993, 1000.000000000000000 ) ;
#25353 = ORIENTED_EDGE ( 'NONE', *, *, #7450, .F. ) ;
#25354 = CARTESIAN_POINT ( 'NONE',  ( 9.884929003653626367, 57.36421526887348676, -139.1775604444698047 ) ) ;
#25355 = CARTESIAN_POINT ( 'NONE',  ( 30.59141879584271706, 116.1811685142589141, 2.701465575440082478 ) ) ;
#25356 = CARTESIAN_POINT ( 'NONE',  ( 6.224689322667630975, 134.1951906609239131, 62.55544044765293421 ) ) ;
#25357 = CARTESIAN_POINT ( 'NONE',  ( 119.2224693531409088, 70.00000000000002842, 19.99999999999995026 ) ) ;
#25358 = CARTESIAN_POINT ( 'NONE',  ( 2.433796855181219243, 107.1581411821798895, -98.43889364293755762 ) ) ;
#25359 = CARTESIAN_POINT ( 'NONE',  ( 1.833750490713715431, -138.0897889879342131, 44.58740205676281931 ) ) ;
#25360 = ORIENTED_EDGE ( 'NONE', *, *, #3144, .T. ) ;
#25361 = CARTESIAN_POINT ( 'NONE',  ( 1.833838848569386837, -144.2962335061013732, 15.34509722932487463 ) ) ;
#25362 = CARTESIAN_POINT ( 'NONE',  ( 2.433796855181219243, -31.67151202412867761, -142.0211193075559493 ) ) ;
#25363 =( BOUNDED_SURFACE ( )  B_SPLINE_SURFACE ( 3, 1, ( 
 ( #868, #4906 ),
 ( #6792, #22627 ),
 ( #11673, #13674 ),
 ( #20587, #15684 ) ),
 .UNSPECIFIED., .F., .F., .F. ) 
 B_SPLINE_SURFACE_WITH_KNOTS ( ( 4, 4 ),
 ( 2, 2 ),
 ( 0.000000000000000000, 1.000000000000000000 ),
 ( 0.000000000000000000, 1.000000000000000000 ),
 .UNSPECIFIED. ) 
 GEOMETRIC_REPRESENTATION_ITEM ( )  RATIONAL_B_SPLINE_SURFACE ( (
 ( 1.000000000000000000, 1.000000000000000000),
 ( 0.9960225298536222738, 0.9999952330161893110),
 ( 0.9960225298536222738, 0.9999952330161893110),
 ( 1.000000000000000000, 1.000000000000000000) ) ) 
 REPRESENTATION_ITEM ( '' )  SURFACE ( )  );
#25364 = CARTESIAN_POINT ( 'NONE',  ( 2.433796855181219243, 86.69855925933974561, 116.8607839509059829 ) ) ;
#25365 = CARTESIAN_POINT ( 'NONE',  ( -20.20612091757427109, -16.46550228026411844, -24.59769958242381094 ) ) ;
#25366 = ORIENTED_EDGE ( 'NONE', *, *, #6372, .T. ) ;
#25367 = CARTESIAN_POINT ( 'NONE',  ( 1.833721034905635205, 145.1093571238132540, -0.3559403234842271058 ) ) ;
#25368 = VECTOR ( 'NONE', #20275, 1000.000000000000000 ) ;
#25369 = CARTESIAN_POINT ( 'NONE',  ( 1.833485406944057594, 125.9346397303435197, 72.09189602597754742 ) ) ;
#25370 = ORIENTED_EDGE ( 'NONE', *, *, #10740, .F. ) ;
#25371 = AXIS2_PLACEMENT_3D ( 'NONE', #16052, #12031, #22702 ) ;
#25372 = ORIENTED_EDGE ( 'NONE', *, *, #19493, .T. ) ;
#25373 = EDGE_CURVE ( 'NONE', #27978, #3848, #21140, .T. ) ;
#25374 = EDGE_LOOP ( 'NONE', ( #25691, #15439, #12815, #7282 ) ) ;
#25375 = CIRCLE ( 'NONE', #1006, 151.1787379149930359 ) ;
#25376 = ADVANCED_FACE ( 'NONE', ( #4959 ), #9457, .F. ) ;
#25377 = CARTESIAN_POINT ( 'NONE',  ( 25.64692872815574631, -110.3764733653606953, -23.79008960806713802 ) ) ;
#25378 = CARTESIAN_POINT ( 'NONE',  ( 1.834118845439484335, 0.1779704863090299238, -145.1099497418795750 ) ) ;
#25379 = CARTESIAN_POINT ( 'NONE',  ( 2.430230287190592531, -86.70145658344580397, -116.8646894862420993 ) ) ;
#25380 = DIRECTION ( 'NONE',  ( -0.5914120900931442160, -0.2415416038593017345, 0.7693434820005526920 ) ) ;
#25381 = FACE_OUTER_BOUND ( 'NONE', #24106, .T. ) ;
#25382 = ORIENTED_EDGE ( 'NONE', *, *, #25015, .T. ) ;
#25383 = CARTESIAN_POINT ( 'NONE',  ( 55.79472521941428198, 35.74479459808936355, -63.36760613016186028 ) ) ;
#25384 = CARTESIAN_POINT ( 'NONE',  ( 9.884929003653608603, -109.0134320167725974, -103.8128997986868711 ) ) ;
#25385 = EDGE_CURVE ( 'NONE', #21385, #11913, #10496, .T. ) ;
#25386 = CARTESIAN_POINT ( 'NONE',  ( -20.20700224038492721, -27.82980252387812570, 10.08426345511618649 ) ) ;
#25387 = CARTESIAN_POINT ( 'NONE',  ( 109.1586059443104944, -0.003127959656212910868, 0.006344953511164418483 ) ) ;
#25388 = CARTESIAN_POINT ( 'NONE',  ( 25.64660436782551756, -110.3216080362391125, 24.04259444204624430 ) ) ;
#25389 = LINE ( 'NONE', #12142, #25237 ) ;
#25390 = AXIS2_PLACEMENT_3D ( 'NONE', #8413, #21220, #3653 ) ;
#25391 = CARTESIAN_POINT ( 'NONE',  ( 25.64700659047693776, -66.18331466615499892, -91.48068002582091651 ) ) ;
#25392 = CARTESIAN_POINT ( 'NONE',  ( -7.078251931573406708, -26.33626633876190937, 44.92740138729193689 ) ) ;
#25393 = CARTESIAN_POINT ( 'NONE',  ( 25.64692232868534560, -0.3267662677143608474, -112.9106972861223426 ) ) ;
#25394 = DIRECTION ( 'NONE',  ( 0.5914120900931444380, -0.5938529060132660131, -0.5455001977188070894 ) ) ;
#25395 = CARTESIAN_POINT ( 'NONE',  ( 25.86096068574584805, 12.80894308910881563, -112.3259320600842557 ) ) ;
#25396 = EDGE_LOOP ( 'NONE', ( #15289, #27965, #1790, #8990 ) ) ;
#25397 = FACE_OUTER_BOUND ( 'NONE', #23900, .T. ) ;
#25398 = EDGE_CURVE ( 'NONE', #10905, #23680, #5340, .T. ) ;
#25399 = ORIENTED_EDGE ( 'NONE', *, *, #21254, .T. ) ;
#25400 = CARTESIAN_POINT ( 'NONE',  ( -20.20612091757424622, 8.058516044219587116, 28.48192249925577357 ) ) ;
#25401 =( BOUNDED_SURFACE ( )  B_SPLINE_SURFACE ( 3, 1, ( 
 ( #12689, #14705 ),
 ( #23514, #6101 ),
 ( #12550, #21612 ),
 ( #28224, #1474 ) ),
 .UNSPECIFIED., .F., .F., .F. ) 
 B_SPLINE_SURFACE_WITH_KNOTS ( ( 4, 4 ),
 ( 2, 2 ),
 ( 0.000000000000000000, 1.000000000000000000 ),
 ( 0.000000000000000000, 1.000000000000000000 ),
 .UNSPECIFIED. ) 
 GEOMETRIC_REPRESENTATION_ITEM ( )  RATIONAL_B_SPLINE_SURFACE ( (
 ( 1.000000000000000000, 1.000000000000000000),
 ( 0.9960225298536222738, 0.9999952330161893110),
 ( 0.9960225298536222738, 0.9999952330161893110),
 ( 1.000000000000000000, 1.000000000000000000) ) ) 
 REPRESENTATION_ITEM ( '' )  SURFACE ( )  );
#25402 = B_SPLINE_CURVE_WITH_KNOTS ( 'NONE', 3,
 ( #222, #9438, #13882, #26837, #20503, #20074, #24712 ),
 .UNSPECIFIED., .F., .F.,
 ( 4, 3, 4 ),
 ( 4.909604562510253576E-17, 0.02816610861753246833, 0.04000277880656220864 ),
 .UNSPECIFIED. ) ;
#25403 = VERTEX_POINT ( 'NONE', #9568 ) ;
#25404 = EDGE_CURVE ( 'NONE', #13800, #21625, #2578, .T. ) ;
#25405 = ORIENTED_EDGE ( 'NONE', *, *, #17825, .F. ) ;
#25406 = VERTEX_POINT ( 'NONE', #15593 ) ;
#25407 = EDGE_CURVE ( 'NONE', #14659, #13886, #17564, .T. ) ;
#25409 =( BOUNDED_SURFACE ( )  B_SPLINE_SURFACE ( 3, 1, ( 
 ( #26449, #7042 ),
 ( #24454, #2119 ),
 ( #11058, #17803 ),
 ( #10791, #15218 ) ),
 .UNSPECIFIED., .F., .F., .F. ) 
 B_SPLINE_SURFACE_WITH_KNOTS ( ( 4, 4 ),
 ( 2, 2 ),
 ( 0.000000000000000000, 1.000000000000000000 ),
 ( 0.000000000000000000, 1.000000000000000000 ),
 .UNSPECIFIED. ) 
 GEOMETRIC_REPRESENTATION_ITEM ( )  RATIONAL_B_SPLINE_SURFACE ( (
 ( 1.000000000000000000, 1.000000000000000000),
 ( 0.9593753223639863714, 0.9995975284513187731),
 ( 0.9593753223639863714, 0.9995975284513187731),
 ( 1.000000000000000000, 1.000000000000000000) ) ) 
 REPRESENTATION_ITEM ( '' )  SURFACE ( )  );
#25408 = VECTOR ( 'NONE', #14452, 999.9999999999998863 ) ;
#25410 = EDGE_CURVE ( 'NONE', #17451, #13981, #21708, .T. ) ;
#25411 = CIRCLE ( 'NONE', #17568, 151.1787379149930359 ) ;
#25412 = CARTESIAN_POINT ( 'NONE',  ( 1.833485406944057594, -141.8265699653869376, 30.69200235378888308 ) ) ;
#25413 = CARTESIAN_POINT ( 'NONE',  ( -25.21435515916043713, -31.17620025257598471, -15.02493970636134613 ) ) ;
#25414 = CARTESIAN_POINT ( 'NONE',  ( 2.430230287190572103, 138.8342928068226172, -43.58368230469245930 ) ) ;
#25415 = LINE ( 'NONE', #20641, #25408 ) ;
#25416 = CARTESIAN_POINT ( 'NONE',  ( -1.323830074806772172, 28.92190886481864709, -35.86387698262922186 ) ) ;
#25417 = B_SPLINE_CURVE_WITH_KNOTS ( 'NONE', 3,
 ( #26975, #13888, #22698, #3103 ),
 .UNSPECIFIED., .F., .F.,
 ( 4, 4 ),
 ( 1.450544195894442722E-16, 0.008383748772659595921 ),
 .UNSPECIFIED. ) ;
#25418 = CARTESIAN_POINT ( 'NONE',  ( 2.433796855181205476, 28.83182736670536528, 142.6247129145649239 ) ) ;
#25420 = CARTESIAN_POINT ( 'NONE',  ( -1.049817751779873687, -13.66628317065018017, -43.71287583013722156 ) ) ;
#25419 = CARTESIAN_POINT ( 'NONE',  ( -20.24419206586952669, 10.37009329716804196, 27.76448493191432476 ) ) ;
#25421 = CARTESIAN_POINT ( 'NONE',  ( -25.21435515916043357, -6.169479169075226643, 34.05351380035340014 ) ) ;
#25422 = ORIENTED_EDGE ( 'NONE', *, *, #5811, .T. ) ;
#25423 = ORIENTED_EDGE ( 'NONE', *, *, #1932, .F. ) ;
#25424 = CARTESIAN_POINT ( 'NONE',  ( 1.833485406944057594, -125.4007332306550921, 73.01664920992921282 ) ) ;
#25426 = LINE ( 'NONE', #23270, #27033 ) ;
#25425 = FACE_OUTER_BOUND ( 'NONE', #28458, .T. ) ;
#25427 = CARTESIAN_POINT ( 'NONE',  ( 10.93730112725971004, 10.89264110825002163, 150.7858122213661147 ) ) ;
#25428 = FACE_OUTER_BOUND ( 'NONE', #2944, .T. ) ;
#25429 = CARTESIAN_POINT ( 'NONE',  ( 2.263178607246638219, 144.7392885066942938, 13.80342482180135022 ) ) ;
#25430 = VERTEX_POINT ( 'NONE', #21065 ) ;
#25431 = CARTESIAN_POINT ( 'NONE',  ( 109.1586900883932856, 0.0008465529156545867481, -0.007088091345232581594 ) ) ;
#25432 = VECTOR ( 'NONE', #7621, 1000.000000000000114 ) ;
#25433 = EDGE_CURVE ( 'NONE', #23751, #16681, #14613, .T. ) ;
#25434 = CARTESIAN_POINT ( 'NONE',  ( -7.078251931573400491, -51.82710018979479116, -5.101176922830485516 ) ) ;
#25435 = CARTESIAN_POINT ( 'NONE',  ( 1.833838850093452821, -15.16809710532158739, 144.3148369740567887 ) ) ;
#25436 = VERTEX_POINT ( 'NONE', #16773 ) ;
#25437 = CARTESIAN_POINT ( 'NONE',  ( 25.64681081121879203, -97.99105938547964456, 56.09509703373309719 ) ) ;
#25438 = EDGE_CURVE ( 'NONE', #8964, #16334, #14247, .T. ) ;
#25439 = CARTESIAN_POINT ( 'NONE',  ( -1.045287976400365970, -37.92705037016778391, -25.66401692419976399 ) ) ;
#25440 = ORIENTED_EDGE ( 'NONE', *, *, #18954, .T. ) ;
#25441 = VERTEX_POINT ( 'NONE', #3095 ) ;
#25442 = EDGE_CURVE ( 'NONE', #20568, #27505, #25415, .T. ) ;
#25443 = CARTESIAN_POINT ( 'NONE',  ( 1.833206310202323941, -85.89457578512735836, -116.9567751109827611 ) ) ;
#25444 =( BOUNDED_SURFACE ( )  B_SPLINE_SURFACE ( 3, 1, ( 
 ( #15399, #2446 ),
 ( #13379, #6649 ),
 ( #26623, #22330 ),
 ( #2592, #8799 ) ),
 .UNSPECIFIED., .F., .F., .F. ) 
 B_SPLINE_SURFACE_WITH_KNOTS ( ( 4, 4 ),
 ( 2, 2 ),
 ( 0.000000000000000000, 1.000000000000000000 ),
 ( 0.000000000000000000, 1.000000000000000000 ),
 .UNSPECIFIED. ) 
 GEOMETRIC_REPRESENTATION_ITEM ( )  RATIONAL_B_SPLINE_SURFACE ( (
 ( 1.000000000000000000, 1.000000000000000000),
 ( 0.7789835883360576307, 0.9689951854195403280),
 ( 0.7789835883360576307, 0.9689951854195403280),
 ( 1.000000000000000000, 1.000000000000000000) ) ) 
 REPRESENTATION_ITEM ( '' )  SURFACE ( )  );
#25445 = ORIENTED_EDGE ( 'NONE', *, *, #23215, .F. ) ;
#25446 = CARTESIAN_POINT ( 'NONE',  ( 109.1586900883932856, 0.006819617742892440312, -0.002109621908824174229 ) ) ;
#25447 = CARTESIAN_POINT ( 'NONE',  ( 28.37603512858358812, -114.7183465482399640, 1.794342805482467496 ) ) ;
#25448 = DIRECTION ( 'NONE',  ( -1.000000000000000000, -2.451419619960044761E-16, -6.977076472649138108E-18 ) ) ;
#25449 = CARTESIAN_POINT ( 'NONE',  ( 1.833485406944043827, -73.01664920992880070, -125.4007332306553195 ) ) ;
#25450 = VECTOR ( 'NONE', #21287, 1000.000000000000000 ) ;
#25451 = CARTESIAN_POINT ( 'NONE',  ( 1.893872463202078027, -59.90695624048775869, 132.2106029832900447 ) ) ;
#25452 = VECTOR ( 'NONE', #23869, 1000.000000000000227 ) ;
#25453 = CARTESIAN_POINT ( 'NONE',  ( 109.1721716018069657, -0.01488186354166052411, -0.008358834333183878806 ) ) ;
#25454 = CARTESIAN_POINT ( 'NONE',  ( -55.24340739397742794, -0.007744344507854267548, 0.006539691034608354631 ) ) ;
#25455 = CARTESIAN_POINT ( 'NONE',  ( 2.433796855181205476, 116.8607839509056561, 86.69855925934011509 ) ) ;
#25456 = CARTESIAN_POINT ( 'NONE',  ( 109.1586900883932856, -0.0001010081143976501722, -0.007137750914550312215 ) ) ;
#25457 = ORIENTED_EDGE ( 'NONE', *, *, #24412, .F. ) ;
#25458 = B_SPLINE_CURVE_WITH_KNOTS ( 'NONE', 3,
 ( #6363, #27950, #1746, #10545, #14571, #21141, #855, #25340, #25493, #20574, #25189, #5765, #3163 ),
 .UNSPECIFIED., .F., .F.,
 ( 4, 3, 3, 3, 4 ),
 ( 1.084202172485504434E-17, 0.0007657099931970561164, 0.001531419946797918721, 0.002296279302920154267, 0.003061450627205758099 ),
 .UNSPECIFIED. ) ;
#25459 = B_SPLINE_CURVE_WITH_KNOTS ( 'NONE', 3,
 ( #22485, #24656, #24215, #11384, #15261, #15690 ),
 .UNSPECIFIED., .F., .F.,
 ( 4, 2, 4 ),
 ( 1.734723475976807094E-18, 0.0004335184443140216969, 0.0008670368886280416590 ),
 .UNSPECIFIED. ) ;
#25460 = CARTESIAN_POINT ( 'NONE',  ( 26.28373643307410035, -4.159810388345511534, -127.4927519498666157 ) ) ;
#25462 = CARTESIAN_POINT ( 'NONE',  ( -1.619063947482194177, -46.30105812165547974, 2.489035965910640247 ) ) ;
#25461 = CARTESIAN_POINT ( 'NONE',  ( 1.833750490713697223, 85.50916867388957598, -117.2391074582364467 ) ) ;
#25463 = CARTESIAN_POINT ( 'NONE',  ( -1.113548883309550153, 28.52482525634944821, -35.91246368318211069 ) ) ;
#25464 = ORIENTED_EDGE ( 'NONE', *, *, #9380, .T. ) ;
#25465 = ORIENTED_EDGE ( 'NONE', *, *, #7740, .T. ) ;
#25466 = EDGE_LOOP ( 'NONE', ( #8969, #17762, #883, #4596, #19651, #27285, #18938, #12435, #7725, #9176, #27398, #11973, #18265, #12759, #2346, #27213, #3931, #5126, #10448, #23532, #2210, #3280, #10941, #3828, #15336, #21743, #1502, #7465, #4842, #11569, #10172, #23176, #2851, #9057, #16425, #21675, #4889, #1758, #28367, #2406, #5324, #15498, #9599, #18151, #25752, #7891, #959, #21520, #91, #24310, #3368, #1548, #25933, #25288, #17466, #3386, #12473, #22042, #2910, #18947, #26707, #21840, #6246, #4705, #22990, #25422, #1791, #13758, #7161, #26637, #21554, #10473, #15219, #6332, #26587, #26265, #13739, #21833, #8245, #17858, #15909, #12612, #11968, #8513, #20314, #17272, #740, #22696, #2241, #3219, #20133, #1596, #28272, #2814, #146, #18038, #16966, #14036, #13531, #8566, #3192, #21909, #23167, #10245, #2171, #25879, #14693, #6261, #16554, #19084, #5763, #24802, #11629, #22145, #27826, #1253, #24647, #14442, #15950, #839, #27859, #8452, #15650, #17756, #21330, #17168, #27828, #7909, #1761, #12148, #24515, #14691, #776, #639, #27898, #7239, #19218, #4111, #9514, #424, #5467, #9747, #67, #26347, #12798, #11356, #22945, #1148, #20895, #19626, #17125, #5149, #19126, #25251, #5334, #19313, #7529, #16022, #689, #15383, #18472, #14586, #19630, #6754, #5308, #12150, #17674, #10980, #5171, #16575, #12544, #11655, #22643, #5377, #22345, #9301, #3698, #4134, #21656, #8940, #6590, #21863, #3767, #279 ) ) ;
#25467 = DIRECTION ( 'NONE',  ( 0.5914120900931444380, 0.7693434820005550234, -0.2415416038592938797 ) ) ;
#25468 = CARTESIAN_POINT ( 'NONE',  ( -22.23226125620943705, -29.33577758406442726, 11.82389163795241593 ) ) ;
#25469 = CARTESIAN_POINT ( 'NONE',  ( 8.186469777911021595, 140.9315935720377411, -49.43817851233925609 ) ) ;
#25470 = CARTESIAN_POINT ( 'NONE',  ( -1.050231094221204753, -43.47885872350344982, 14.39477892760344879 ) ) ;
#25471 = CARTESIAN_POINT ( 'NONE',  ( -1.463510566862832762, -11.94877850058534285, -44.64091840826485935 ) ) ;
#25472 = ORIENTED_EDGE ( 'NONE', *, *, #9074, .T. ) ;
#25473 = CARTESIAN_POINT ( 'NONE',  ( 1.893872463202021184, 71.74819926215178612, 126.1771883101040146 ) ) ;
#25474 = CARTESIAN_POINT ( 'NONE',  ( -55.24390624410018802, 0.01027195578988056128, 0.001811362924362418811 ) ) ;
#25475 = ORIENTED_EDGE ( 'NONE', *, *, #22050, .F. ) ;
#25476 = CARTESIAN_POINT ( 'NONE',  ( -12.94347594948482438, 42.93165645342861581, -23.08810053288705078 ) ) ;
#25477 = CARTESIAN_POINT ( 'NONE',  ( 16.75465622695654844, -25.01894884133755070, -140.0080030360330170 ) ) ;
#25478 = CARTESIAN_POINT ( 'NONE',  ( 9.884929003653626367, 141.8132360130364589, -50.49804566711977571 ) ) ;
#25479 = DIRECTION ( 'NONE',  ( -1.000000000000000000, -0.000000000000000000, -0.000000000000000000 ) ) ;
#25480 = CARTESIAN_POINT ( 'NONE',  ( 25.64703792032469565, 107.4308312803558749, 34.74993974076994618 ) ) ;
#25481 = CARTESIAN_POINT ( 'NONE',  ( -55.24728320129491266, 0.01137345571546872526, -0.009072670231975240793 ) ) ;
#25482 = CARTESIAN_POINT ( 'NONE',  ( -1.045287976400379737, -25.66401692420040703, -37.92705037016734337 ) ) ;
#25483 = EDGE_CURVE ( 'NONE', #24182, #11790, #28310, .T. ) ;
#25484 = VERTEX_POINT ( 'NONE', #9717 ) ;
#25485 = CARTESIAN_POINT ( 'NONE',  ( -10.86508079875781263, -22.20099862734791074, 46.07061504567109012 ) ) ;
#25486 = CARTESIAN_POINT ( 'NONE',  ( 13.36082413113063083, -41.18148072373715962, 147.2768864064166507 ) ) ;
#25487 = ADVANCED_FACE ( 'NONE', ( #14594 ), #11153, .T. ) ;
#25488 = CARTESIAN_POINT ( 'NONE',  ( 13.36082413113063083, 119.8836995922739419, -94.94363694443931934 ) ) ;
#25489 = EDGE_CURVE ( 'NONE', #20246, #13959, #2949, .T. ) ;
#25490 = ORIENTED_EDGE ( 'NONE', *, *, #25925, .F. ) ;
#25491 = CARTESIAN_POINT ( 'NONE',  ( -1.619063947482197729, -2.489035965909835557, 46.30105812165550816 ) ) ;
#25492 = B_SPLINE_CURVE_WITH_KNOTS ( 'NONE', 3,
 ( #3531, #9888, #22995, #5556, #5412, #27567, #25143, #16204, #2979, #25437 ),
 .UNSPECIFIED., .F., .F.,
 ( 4, 3, 3, 4 ),
 ( 1.387778780781445676E-17, 0.0002669560319015820129, 0.0005492286108966361411, 0.0008315040496093414283 ),
 .UNSPECIFIED. ) ;
#25493 = CARTESIAN_POINT ( 'NONE',  ( -1.049817751779888786, 45.79652915392415480, 0.5106138415328438374 ) ) ;
#25494 = CARTESIAN_POINT ( 'NONE',  ( 26.11404676487259024, 76.59696442953192275, 83.38016054979810576 ) ) ;
#25495 = VECTOR ( 'NONE', #12452, 1000.000000000000000 ) ;
#25496 = CARTESIAN_POINT ( 'NONE',  ( 25.64699802086726166, -23.24292564406113470, 110.4930320910559942 ) ) ;
#25497 = CARTESIAN_POINT ( 'NONE',  ( 32.73300124599740002, -110.6325518752271080, -39.98094346392423404 ) ) ;
#25498 = CARTESIAN_POINT ( 'NONE',  ( 1.833809397773845440, 141.9016658667396200, 30.34407330672235048 ) ) ;
#25499 = CARTESIAN_POINT ( 'NONE',  ( -1.619063947482197729, -29.22875152547730337, 35.99532424477411041 ) ) ;
#25500 =( BOUNDED_SURFACE ( )  B_SPLINE_SURFACE ( 3, 1, ( 
 ( #3908, #21031 ),
 ( #16739, #5494 ),
 ( #8237, #18740 ),
 ( #1321, #10117 ) ),
 .UNSPECIFIED., .F., .F., .F. ) 
 B_SPLINE_SURFACE_WITH_KNOTS ( ( 4, 4 ),
 ( 2, 2 ),
 ( 0.000000000000000000, 1.000000000000000000 ),
 ( 0.000000000000000000, 1.000000000000000000 ),
 .UNSPECIFIED. ) 
 GEOMETRIC_REPRESENTATION_ITEM ( )  RATIONAL_B_SPLINE_SURFACE ( (
 ( 1.000000000000000000, 1.000000000000000000),
 ( 0.7789835883360576307, 0.9689951854195403280),
 ( 0.7789835883360576307, 0.9689951854195403280),
 ( 1.000000000000000000, 1.000000000000000000) ) ) 
 REPRESENTATION_ITEM ( '' )  SURFACE ( )  );
#25501 = CARTESIAN_POINT ( 'NONE',  ( 25.64692872815576408, 112.3258062264003740, -11.48248630407163340 ) ) ;
#25502 = CARTESIAN_POINT ( 'NONE',  ( 2.433796855181205476, -16.65276281464661423, 144.5536872373191102 ) ) ;
#25503 = ORIENTED_EDGE ( 'NONE', *, *, #7740, .F. ) ;
#25504 = VERTEX_POINT ( 'NONE', #5389 ) ;
#25505 = CARTESIAN_POINT ( 'NONE',  ( 1.833809397773848993, -30.34407330672281589, 141.9016658667395632 ) ) ;
#25506 = PRODUCT_DEFINITION ( 'UNKNOWN', '', #6152, #1042 ) ;
#25507 = CARTESIAN_POINT ( 'NONE',  ( -1.239374126674604337, -45.98822239537607715, 2.406737988131604666 ) ) ;
#25508 = LINE ( 'NONE', #3461, #10974 ) ;
#25509 = CARTESIAN_POINT ( 'NONE',  ( -25.21435515916025594, 1.749597353048488237E-16, -4.373993382621220594E-17 ) ) ;
#25510 = CARTESIAN_POINT ( 'NONE',  ( -7.733045908741344121, 38.67583825854200086, 35.49239760110631181 ) ) ;
#25511 = CARTESIAN_POINT ( 'NONE',  ( -1.045287976400365970, 28.14015102489882736, 36.12803364096558312 ) ) ;
#25512 = ORIENTED_EDGE ( 'NONE', *, *, #19177, .T. ) ;
#25513 = CARTESIAN_POINT ( 'NONE',  ( 5.340103556456385014, 57.86178752079319310, 135.6222865117683511 ) ) ;
#25514 = CARTESIAN_POINT ( 'NONE',  ( 109.1721716018069515, -0.001583175916617694974, -0.01699510305643761945 ) ) ;
#25515 = DIRECTION ( 'NONE',  ( 0.7563875759206387661, 0.6320336713238499105, -0.1685564395263362270 ) ) ;
#25516 = EDGE_CURVE ( 'NONE', #7819, #27747, #2877, .T. ) ;
#25517 = CARTESIAN_POINT ( 'NONE',  ( 2.108393763691166267, 46.11438684123344700, -137.7805780486501988 ) ) ;
#25518 = CARTESIAN_POINT ( 'NONE',  ( 25.73574536432416693, 65.74844932374649886, 91.86645484851332810 ) ) ;
#25519 = EDGE_LOOP ( 'NONE', ( #20431, #14784, #2108, #11753 ) ) ;
#25520 = CARTESIAN_POINT ( 'NONE',  ( 25.65782528836482257, 22.91156770660802522, 110.5695798068304185 ) ) ;
#25521 = CARTESIAN_POINT ( 'NONE',  ( -1.259972190295293393, -28.82609802125285015, -35.85909728507041194 ) ) ;
#25522 = ORIENTED_EDGE ( 'NONE', *, *, #4933, .F. ) ;
#25523 = EDGE_LOOP ( 'NONE', ( #25044, #24194, #23922, #20628 ) ) ;
#25524 = VERTEX_POINT ( 'NONE', #17980 ) ;
#25525 = CARTESIAN_POINT ( 'NONE',  ( 25.64681081121879203, -107.5125461021405044, 34.49579773461748999 ) ) ;
#25526 = DIRECTION ( 'NONE',  ( 1.000000000000000000, -6.938893903907226837E-18, 1.734723475976806709E-18 ) ) ;
#25527 = DIRECTION ( 'NONE',  ( 0.5946245182733607137, 0.1642747008466135250, 0.7870422510449672782 ) ) ;
#25528 =( BOUNDED_SURFACE ( )  B_SPLINE_SURFACE ( 3, 1, ( 
 ( #13647, #18387 ),
 ( #24759, #24621 ),
 ( #20263, #27170 ),
 ( #26740, #698 ) ),
 .UNSPECIFIED., .F., .F., .F. ) 
 B_SPLINE_SURFACE_WITH_KNOTS ( ( 4, 4 ),
 ( 2, 2 ),
 ( 0.000000000000000000, 1.000000000000000000 ),
 ( 0.000000000000000000, 1.000000000000000000 ),
 .UNSPECIFIED. ) 
 GEOMETRIC_REPRESENTATION_ITEM ( )  RATIONAL_B_SPLINE_SURFACE ( (
 ( 1.000000000000000000, 1.000000000000000000),
 ( 0.9956975270656954757, 0.8568959468854893125),
 ( 0.9956975270656954757, 0.8568959468854893125),
 ( 1.000000000000000000, 1.000000000000000000) ) ) 
 REPRESENTATION_ITEM ( '' )  SURFACE ( )  );
#25529 = CARTESIAN_POINT ( 'NONE',  ( 30.58324630866346538, 77.95273942827475366, -92.47020419020104498 ) ) ;
#25530 = CARTESIAN_POINT ( 'NONE',  ( 10.93730112725932635, 0.000000000000000000, 0.000000000000000000 ) ) ;
#25531 = CARTESIAN_POINT ( 'NONE',  ( -1.539760825549689072, 46.22267384399381740, -2.469813586483248447 ) ) ;
#25532 = EDGE_CURVE ( 'NONE', #20029, #6423, #436, .T. ) ;
#25533 = CARTESIAN_POINT ( 'NONE',  ( 32.73300124599732186, 0.000000000000000000, 0.000000000000000000 ) ) ;
#25534 = CARTESIAN_POINT ( 'NONE',  ( -25.21435515916043357, -15.02493970636125198, 31.17620025257602379 ) ) ;
#25535 = CARTESIAN_POINT ( 'NONE',  ( 25.64708010899965629, -11.74803558238360957, 112.2984447178532719 ) ) ;
#25536 = EDGE_CURVE ( 'NONE', #11759, #6633, #108, .T. ) ;
#25537 = CARTESIAN_POINT ( 'NONE',  ( -7.078251931573400491, 50.86685171665412497, -11.16394717458693897 ) ) ;
#25538 = EDGE_CURVE ( 'NONE', #8126, #21801, #9839, .T. ) ;
#25539 = CARTESIAN_POINT ( 'NONE',  ( -1.323830074806772394, 35.86387698262958423, 28.92190886481825274 ) ) ;
#25540 = CARTESIAN_POINT ( 'NONE',  ( 109.1624594426973118, 0.006066618937910909712, -0.01476644236456991707 ) ) ;
#25541 = CARTESIAN_POINT ( 'NONE',  ( -19.53423201713130197, 1.355459634611817678E-16, -3.388649086529544194E-17 ) ) ;
#25542 = CARTESIAN_POINT ( 'NONE',  ( -20.57838717382308147, -16.28767523336139078, -25.16001208503099917 ) ) ;
#25543 = CARTESIAN_POINT ( 'NONE',  ( 32.73300124599740002, 103.7392577722183660, -55.46353551261898218 ) ) ;
#25544 = ORIENTED_EDGE ( 'NONE', *, *, #25584, .F. ) ;
#25545 = CARTESIAN_POINT ( 'NONE',  ( -1.464342487929852998, 25.15873223207692178, -38.76467504336592640 ) ) ;
#25546 = ORIENTED_EDGE ( 'NONE', *, *, #4414, .F. ) ;
#25547 = CARTESIAN_POINT ( 'NONE',  ( -1.050230346682676785, 43.55772679531850855, -14.15203301556446647 ) ) ;
#25548 = CARTESIAN_POINT ( 'NONE',  ( 109.1624594426973118, -0.01216903288310969451, -0.01033277910989000709 ) ) ;
#25549 = ORIENTED_EDGE ( 'NONE', *, *, #17095, .T. ) ;
#25550 = ORIENTED_EDGE ( 'NONE', *, *, #12383, .T. ) ;
#25551 = ORIENTED_EDGE ( 'NONE', *, *, #4289, .F. ) ;
#25552 = CARTESIAN_POINT ( 'NONE',  ( -20.24419206586952313, 16.36655224501367911, -24.70913649113835930 ) ) ;
#25553 = CARTESIAN_POINT ( 'NONE',  ( -24.53237795827024570, -33.25734978085267102, -6.738475012719991497 ) ) ;
#25554 = EDGE_CURVE ( 'NONE', #12534, #27588, #24933, .T. ) ;
#25555 = CARTESIAN_POINT ( 'NONE',  ( -20.38016308990357928, 1.509191766064626128, 29.73560196176844173 ) ) ;
#25556 = CARTESIAN_POINT ( 'NONE',  ( 25.98107933586723917, 35.99661810151007302, -107.2544904356368534 ) ) ;
#25557 = CARTESIAN_POINT ( 'NONE',  ( 10.93730112726006354, 148.8212007290666747, -26.59437931460595905 ) ) ;
#25558 = CARTESIAN_POINT ( 'NONE',  ( 1.833485406944043827, 138.1714136985314383, -44.33323125129781772 ) ) ;
#25559 = CARTESIAN_POINT ( 'NONE',  ( 25.64708010899966339, 56.50300922386594493, 97.75667227735105769 ) ) ;
#25560 = CARTESIAN_POINT ( 'NONE',  ( -22.23226125620928784, -7.677408153693816573, 30.68305173820434462 ) ) ;
#25561 = EDGE_CURVE ( 'NONE', #25524, #600, #14970, .T. ) ;
#25562 = ORIENTED_EDGE ( 'NONE', *, *, #13875, .T. ) ;
#25563 =( BOUNDED_SURFACE ( )  B_SPLINE_SURFACE ( 3, 1, ( 
 ( #4794, #38 ),
 ( #4360, #8681 ),
 ( #24099, #8833 ),
 ( #15282, #15870 ) ),
 .UNSPECIFIED., .F., .F., .F. ) 
 B_SPLINE_SURFACE_WITH_KNOTS ( ( 4, 4 ),
 ( 2, 2 ),
 ( 0.000000000000000000, 1.000000000000000000 ),
 ( 0.000000000000000000, 1.000000000000000000 ),
 .UNSPECIFIED. ) 
 GEOMETRIC_REPRESENTATION_ITEM ( )  RATIONAL_B_SPLINE_SURFACE ( (
 ( 1.000000000000000000, 1.000000000000000000),
 ( 0.9956975270656955868, 0.8568959468854907557),
 ( 0.9956975270656955868, 0.8568959468854907557),
 ( 1.000000000000000000, 1.000000000000000000) ) ) 
 REPRESENTATION_ITEM ( '' )  SURFACE ( )  );
#25564 = ORIENTED_EDGE ( 'NONE', *, *, #27827, .F. ) ;
#25565 = CARTESIAN_POINT ( 'NONE',  ( 2.430230287190581429, 1.451610819319768764, -145.5073573687466535 ) ) ;
#25567 = LINE ( 'NONE', #19208, #5936 ) ;
#25566 = CARTESIAN_POINT ( 'NONE',  ( -6.574463467970464770, -44.27173031830730565, -25.96726214983177528 ) ) ;
#25568 = LINE ( 'NONE', #5704, #17501 ) ;
#25569 = CARTESIAN_POINT ( 'NONE',  ( 10.93730112725990011, -115.5857507957697976, -97.44200844886394464 ) ) ;
#25570 = FACE_OUTER_BOUND ( 'NONE', #670, .T. ) ;
#25571 = CARTESIAN_POINT ( 'NONE',  ( -55.24271866751342941, 0.004365563123939763222, -0.008433070970614044842 ) ) ;
#25572 = CARTESIAN_POINT ( 'NONE',  ( -1.045287976400362417, -28.14015102489855735, -36.12803364096578207 ) ) ;
#25573 = EDGE_LOOP ( 'NONE', ( #15824, #9159, #7305, #11040 ) ) ;
#25574 = ORIENTED_EDGE ( 'NONE', *, *, #21702, .T. ) ;
#25575 = CARTESIAN_POINT ( 'NONE',  ( 109.1592201516379674, 0.007856029051022768092, -0.0003082430542016078114 ) ) ;
#25576 =( BOUNDED_SURFACE ( )  B_SPLINE_SURFACE ( 3, 1, ( 
 ( #9418, #5080 ),
 ( #9270, #9550 ),
 ( #20339, #11852 ),
 ( #20189, #20622 ) ),
 .UNSPECIFIED., .F., .F., .F. ) 
 B_SPLINE_SURFACE_WITH_KNOTS ( ( 4, 4 ),
 ( 2, 2 ),
 ( 0.000000000000000000, 1.000000000000000000 ),
 ( 0.000000000000000000, 1.000000000000000000 ),
 .UNSPECIFIED. ) 
 GEOMETRIC_REPRESENTATION_ITEM ( )  RATIONAL_B_SPLINE_SURFACE ( (
 ( 1.000000000000000000, 1.000000000000000000),
 ( 0.9593753223639863714, 0.9995975284513187731),
 ( 0.9593753223639863714, 0.9995975284513187731),
 ( 1.000000000000000000, 1.000000000000000000) ) ) 
 REPRESENTATION_ITEM ( '' )  SURFACE ( )  );
#25577 = ORIENTED_EDGE ( 'NONE', *, *, #27973, .T. ) ;
#25578 = EDGE_LOOP ( 'NONE', ( #12249, #2040, #26299, #16271 ) ) ;
#25579 = CARTESIAN_POINT ( 'NONE',  ( 1.833838850855463054, 97.03125735562237253, 107.8971100408353720 ) ) ;
#25580 = ORIENTED_EDGE ( 'NONE', *, *, #852, .F. ) ;
#25581 = CARTESIAN_POINT ( 'NONE',  ( 109.1586059443104944, 0.007068659269321313221, -0.0002768082440289001381 ) ) ;
#25582 = CARTESIAN_POINT ( 'NONE',  ( 109.1586900883932856, -0.007088091345232585064, -0.0008465529156545589925 ) ) ;
#25583 = CARTESIAN_POINT ( 'NONE',  ( -55.25719721206881729, 0.006045473558784871665, -0.009391134844733287426 ) ) ;
#25584 = EDGE_CURVE ( 'NONE', #13097, #12529, #15532, .T. ) ;
#25585 = DIRECTION ( 'NONE',  ( 0.000000000000000000, 0.000000000000000000, 1.000000000000000000 ) ) ;
#25586 = B_SPLINE_CURVE_WITH_KNOTS ( 'NONE', 3,
 ( #16064, #3117, #24865, #5130, #9596, #18356 ),
 .UNSPECIFIED., .F., .F.,
 ( 4, 2, 4 ),
 ( 1.390486644391990834E-17, 0.0006311571484586074154, 0.001262314296917200953 ),
 .UNSPECIFIED. ) ;
#25587 = CARTESIAN_POINT ( 'NONE',  ( 32.73300124599734318, 105.8473486001051072, 51.32617430724947383 ) ) ;
#25588 = DIRECTION ( 'NONE',  ( 0.000000000000000000, 0.000000000000000000, 1.000000000000000000 ) ) ;
#25589 = CARTESIAN_POINT ( 'NONE',  ( 19.66333377628667023, 129.5498775999591317, 46.81583828063135400 ) ) ;
#25590 = EDGE_CURVE ( 'NONE', #19162, #26024, #18369, .T. ) ;
#25591 = B_SPLINE_CURVE_WITH_KNOTS ( 'NONE', 3,
 ( #12274, #12403, #3073, #16303, #21190, #1475, #8115, #9841, #10284, #27526 ),
 .UNSPECIFIED., .F., .F.,
 ( 4, 3, 3, 4 ),
 ( 0.000000000000000000, 0.0002669560319015562089, 0.0005492286108966316959, 0.0008315040496093448977 ),
 .UNSPECIFIED. ) ;
#25592 = EDGE_LOOP ( 'NONE', ( #14923, #5399, #12836, #17981 ) ) ;
#25593 = DIRECTION ( 'NONE',  ( 0.000000000000000000, 5.223019709707975211E-21, -1.000000000000000000 ) ) ;
#25595 = CARTESIAN_POINT ( 'NONE',  ( -1.048172774974303278, 43.23017713506524728, -15.11899685083838030 ) ) ;
#25594 = CARTESIAN_POINT ( 'NONE',  ( 32.73300124599734318, 89.94078864464067635, 75.82012867748514395 ) ) ;
#25596 = LINE ( 'NONE', #8308, #25807 ) ;
#25597 = EDGE_CURVE ( 'NONE', #2611, #2245, #6720, .T. ) ;
#25598 = ORIENTED_EDGE ( 'NONE', *, *, #9667, .T. ) ;
#25599 = ORIENTED_EDGE ( 'NONE', *, *, #780, .T. ) ;
#25600 = CARTESIAN_POINT ( 'NONE',  ( -1.239374126674604337, -2.406737988131443906, -45.98822239537607715 ) ) ;
#25601 = FACE_OUTER_BOUND ( 'NONE', #12287, .T. ) ;
#25603 = CARTESIAN_POINT ( 'NONE',  ( 32.73300124599732186, 0.000000000000000000, 0.000000000000000000 ) ) ;
#25602 = CARTESIAN_POINT ( 'NONE',  ( -20.20700224038492721, 28.44216453106548315, 8.199606986804035103 ) ) ;
#25604 = CARTESIAN_POINT ( 'NONE',  ( 2.433796855181233454, -1.451562450948615135, -145.5024947199069913 ) ) ;
#25605 = CARTESIAN_POINT ( 'NONE',  ( 10.93730112725990367, -125.1380233598473950, -84.82621002473567273 ) ) ;
#25606 = VERTEX_POINT ( 'NONE', #20007 ) ;
#25607 = CARTESIAN_POINT ( 'NONE',  ( -23.79223135445719350, -28.60983116549952143, 16.82181692922848626 ) ) ;
#25609 = EDGE_CURVE ( 'NONE', #3978, #17856, #538, .T. ) ;
#25608 = CARTESIAN_POINT ( 'NONE',  ( 2.433796855181233454, -16.65276281464466024, -144.5536872373193660 ) ) ;
#25610 = ORIENTED_EDGE ( 'NONE', *, *, #22802, .T. ) ;
#25611 = DIRECTION ( 'NONE',  ( -1.000000000000000000, -0.000000000000000000, -0.000000000000000000 ) ) ;
#25612 = CARTESIAN_POINT ( 'NONE',  ( -1.031422197589716205, 15.60268798220698017, 43.06660437151292342 ) ) ;
#25613 = CARTESIAN_POINT ( 'NONE',  ( 25.73574536432416338, -67.05280231777561539, 90.91878692682003305 ) ) ;
#25614 = CARTESIAN_POINT ( 'NONE',  ( 10.93730112725978287, -140.0398180619114896, 56.95489579269701608 ) ) ;
#25615 = B_SPLINE_CURVE_WITH_KNOTS ( 'NONE', 3,
 ( #17321, #19491, #10218, #6397, #1134, #6543, #10066, #27598 ),
 .UNSPECIFIED., .F., .F.,
 ( 4, 2, 2, 4 ),
 ( 2.211348276820754320E-16, 0.002761568181852864200, 0.005523136363705507222, 0.01104627272741079066 ),
 .UNSPECIFIED. ) ;
#25616 = CARTESIAN_POINT ( 'NONE',  ( -55.24728320129491266, -0.0006547948648734058493, -0.01453410071985278100 ) ) ;
#25617 = CARTESIAN_POINT ( 'NONE',  ( -25.21435515916025594, 1.749597353048488237E-16, -4.373993382621220594E-17 ) ) ;
#25618 = CARTESIAN_POINT ( 'NONE',  ( 26.11404676487257603, -84.89295829319442532, -74.91683232331061504 ) ) ;
#25619 = VERTEX_POINT ( 'NONE', #27445 ) ;
#25620 = CARTESIAN_POINT ( 'NONE',  ( -1.583189561560256253, -29.24830400313190637, -36.01941156322777715 ) ) ;
#25621 =( BOUNDED_SURFACE ( )  B_SPLINE_SURFACE ( 3, 1, ( 
 ( #26599, #26462 ),
 ( #19988, #19700 ),
 ( #6624, #4876 ),
 ( #11353, #19845 ) ),
 .UNSPECIFIED., .F., .F., .F. ) 
 B_SPLINE_SURFACE_WITH_KNOTS ( ( 4, 4 ),
 ( 2, 2 ),
 ( 0.000000000000000000, 1.000000000000000000 ),
 ( 0.000000000000000000, 1.000000000000000000 ),
 .UNSPECIFIED. ) 
 GEOMETRIC_REPRESENTATION_ITEM ( )  RATIONAL_B_SPLINE_SURFACE ( (
 ( 1.000000000000000000, 1.000000000000000000),
 ( 0.7789835883360578528, 0.9689951854195403280),
 ( 0.7789835883360578528, 0.9689951854195403280),
 ( 1.000000000000000000, 1.000000000000000000) ) ) 
 REPRESENTATION_ITEM ( '' )  SURFACE ( )  );
#25622 = CARTESIAN_POINT ( 'NONE',  ( -5.986830583229487246, 49.46736940480273859, 11.27873876172089851 ) ) ;
#25623 = ORIENTED_EDGE ( 'NONE', *, *, #19778, .F. ) ;
#25624 = CARTESIAN_POINT ( 'NONE',  ( 119.2224693531408803, 0.000000000000000000, -19.99999999999998934 ) ) ;
#25625 = ORIENTED_EDGE ( 'NONE', *, *, #4323, .T. ) ;
#25626 = CARTESIAN_POINT ( 'NONE',  ( 55.49584447822657296, 7.849835876629293274, -72.12568090333334681 ) ) ;
#25627 = CARTESIAN_POINT ( 'NONE',  ( 109.1592201516379674, -0.001127733110579631293, 0.007780772729118876421 ) ) ;
#25628 = CARTESIAN_POINT ( 'NONE',  ( -55.24198130335446422, 0.001516807524708540730, -0.009170435128245290474 ) ) ;
#25629 = CARTESIAN_POINT ( 'NONE',  ( -4.780792508754330150, 48.13366140756558309, -11.68149851467477340 ) ) ;
#25630 = CARTESIAN_POINT ( 'NONE',  ( 30.58324630866343341, 57.02364853894626862, -106.6567942264190663 ) ) ;
#25631 = CARTESIAN_POINT ( 'NONE',  ( 25.81918753295379432, 74.93271318951838111, -84.61657260023565641 ) ) ;
#25632 = ADVANCED_FACE ( 'NONE', ( #14192 ), #12233, .F. ) ;
#25633 = B_SPLINE_CURVE_WITH_KNOTS ( 'NONE', 3,
 ( #12082, #20857, #1139, #18695, #8064, #3571 ),
 .UNSPECIFIED., .F., .F.,
 ( 4, 2, 4 ),
 ( 3.469446951953614189E-18, 0.0006311636237756678520, 0.001262327247551332235 ),
 .UNSPECIFIED. ) ;
#25634 = CARTESIAN_POINT ( 'NONE',  ( 1.833750490713671244, -59.26520711749956405, 132.4555075118566378 ) ) ;
#25635 = DIRECTION ( 'NONE',  ( -1.000000000000000000, -0.000000000000000000, -0.000000000000000000 ) ) ;
#25636 = CARTESIAN_POINT ( 'NONE',  ( -1.058473599757817185, 28.32531354681336566, 35.99997772736180224 ) ) ;
#25637 = ORIENTED_EDGE ( 'NONE', *, *, #22408, .T. ) ;
#25638 = EDGE_CURVE ( 'NONE', #7509, #4222, #20779, .T. ) ;
#25639 = ORIENTED_EDGE ( 'NONE', *, *, #23569, .T. ) ;
#25640 = CARTESIAN_POINT ( 'NONE',  ( 30.59138290137873284, 88.14703743378230172, 75.73279410806755152 ) ) ;
#25641 = CARTESIAN_POINT ( 'NONE',  ( 26.28373643307408614, -71.57300207276453818, 105.5888781856748011 ) ) ;
#25642 = CARTESIAN_POINT ( 'NONE',  ( 32.73300124599732186, 0.000000000000000000, 0.000000000000000000 ) ) ;
#25643 = DIRECTION ( 'NONE',  ( -0.7071067811865485719, 4.906538933386790339E-16, 0.7071067811865465735 ) ) ;
#25644 = CARTESIAN_POINT ( 'NONE',  ( -55.24300891470648622, 0.009225237711098475957, 0.003362556190414738716 ) ) ;
#25645 = CARTESIAN_POINT ( 'NONE',  ( 32.73300124599738581, -114.2056417606545864, -28.19767303745721065 ) ) ;
#25646 = CARTESIAN_POINT ( 'NONE',  ( -20.57838717382308147, -23.26537097894118133, -18.89542499756491978 ) ) ;
#25647 = ORIENTED_EDGE ( 'NONE', *, *, #2038, .F. ) ;
#25648 = CARTESIAN_POINT ( 'NONE',  ( 26.11404676487259024, -12.95861723607377414, -112.4785329405483338 ) ) ;
#25649 = CARTESIAN_POINT ( 'NONE',  ( -55.24271866751342941, 0.006757859501010503658, -0.006671293903668132526 ) ) ;
#25650 = CARTESIAN_POINT ( 'NONE',  ( 28.37603512858454735, -75.42810021528147502, 86.45299531409429505 ) ) ;
#25651 = CARTESIAN_POINT ( 'NONE',  ( -7.078251931573406708, 50.86685171665428840, 11.16394717458623731 ) ) ;
#25652 = CARTESIAN_POINT ( 'NONE',  ( 26.11404676487259024, -57.58742681967517285, 97.48350837663589630 ) ) ;
#25653 = CARTESIAN_POINT ( 'NONE',  ( 32.73300124599736449, -115.8010721414085253, 20.69176323058589162 ) ) ;
#25654 = ORIENTED_EDGE ( 'NONE', *, *, #3303, .T. ) ;
#25655 = CARTESIAN_POINT ( 'NONE',  ( 1.832998868059890096, 45.34898734666050046, 137.8420662456171897 ) ) ;
#25657 = CARTESIAN_POINT ( 'NONE',  ( 25.64708228042122329, -11.76327187353738246, -112.2968511928420554 ) ) ;
#25656 = B_SPLINE_CURVE_WITH_KNOTS ( 'NONE', 3,
 ( #27512, #7821, #10676, #1561, #2144, #19582 ),
 .UNSPECIFIED., .F., .F.,
 ( 4, 2, 4 ),
 ( 1.607967956875964627E-16, 0.003570751334075640028, 0.007141502668151118727 ),
 .UNSPECIFIED. ) ;
#25658 = EDGE_LOOP ( 'NONE', ( #11375, #9515, #2503, #17804 ) ) ;
#25659 = B_SPLINE_CURVE_WITH_KNOTS ( 'NONE', 3,
 ( #4806, #766, #26663, #22666, #22812, #9549, #15729, #2935, #11712, #18306, #27087, #24543, #7396 ),
 .UNSPECIFIED., .F., .F.,
 ( 4, 3, 3, 3, 4 ),
 ( 1.551583845779545699E-17, 0.0007657099931970551407, 0.001531419946797920239, 0.002296279302920158170, 0.003061450627205758099 ),
 .UNSPECIFIED. ) ;
#25660 = B_SPLINE_CURVE_WITH_KNOTS ( 'NONE', 3,
 ( #6719, #4835, #4401, #363, #13462, #9150, #657, #22260 ),
 .UNSPECIFIED., .F., .F.,
 ( 4, 2, 2, 4 ),
 ( 0.000000000000000000, 0.002761524886576657151, 0.005523049773153314301, 0.01104609954630661819 ),
 .UNSPECIFIED. ) ;
#25661 = ORIENTED_EDGE ( 'NONE', *, *, #2121, .F. ) ;
#25662 = ORIENTED_EDGE ( 'NONE', *, *, #9207, .F. ) ;
#25663 =( BOUNDED_SURFACE ( )  B_SPLINE_SURFACE ( 3, 1, ( 
 ( #18603, #7536 ),
 ( #13987, #7109 ),
 ( #27374, #20608 ),
 ( #16442, #25228 ) ),
 .UNSPECIFIED., .F., .F., .F. ) 
 B_SPLINE_SURFACE_WITH_KNOTS ( ( 4, 4 ),
 ( 2, 2 ),
 ( 0.000000000000000000, 1.000000000000000000 ),
 ( 0.000000000000000000, 1.000000000000000000 ),
 .UNSPECIFIED. ) 
 GEOMETRIC_REPRESENTATION_ITEM ( )  RATIONAL_B_SPLINE_SURFACE ( (
 ( 1.000000000000000000, 1.000000000000000000),
 ( 0.6386103224230316178, 0.9954351624131538845),
 ( 0.6386103224230316178, 0.9954351624131538845),
 ( 1.000000000000000000, 1.000000000000000000) ) ) 
 REPRESENTATION_ITEM ( '' )  SURFACE ( )  );
#25664 = CARTESIAN_POINT ( 'NONE',  ( -55.24728320129491266, 0.01362040845703093098, -0.005114031043466513160 ) ) ;
#25665 = CARTESIAN_POINT ( 'NONE',  ( -9.156249394959706578, -24.29252099376457608, 48.78605533024762764 ) ) ;
#25666 = CARTESIAN_POINT ( 'NONE',  ( 1.833603222531972277, 30.60504697399407092, -141.8454679205784146 ) ) ;
#25667 = EDGE_CURVE ( 'NONE', #7268, #9431, #3247, .T. ) ;
#25668 = CARTESIAN_POINT ( 'NONE',  ( -15.02187109954785527, 32.04062513125116141, -33.49412687891580021 ) ) ;
#25669 = ORIENTED_EDGE ( 'NONE', *, *, #27802, .T. ) ;
#25670 = EDGE_CURVE ( 'NONE', #23219, #11589, #16515, .T. ) ;
#25671 = FACE_OUTER_BOUND ( 'NONE', #977, .T. ) ;
#25672 = CARTESIAN_POINT ( 'NONE',  ( 1.832998868059890096, 132.3466930259793912, 59.50898020732553562 ) ) ;
#25673 = EDGE_CURVE ( 'NONE', #19718, #27068, #3548, .T. ) ;
#25674 = B_SPLINE_CURVE_WITH_KNOTS ( 'NONE', 3,
 ( #25006, #11747, #7288, #22988, #13892, #660 ),
 .UNSPECIFIED., .F., .F.,
 ( 4, 2, 4 ),
 ( 1.301042606982605321E-18, 0.0006311636237756746825, 0.001262327247551348064 ),
 .UNSPECIFIED. ) ;
#25675 = B_SPLINE_CURVE_WITH_KNOTS ( 'NONE', 3,
 ( #26427, #23744, #6726, #22116 ),
 .UNSPECIFIED., .F., .F.,
 ( 4, 4 ),
 ( 2.081668171172168513E-17, 0.008383748772659474491 ),
 .UNSPECIFIED. ) ;
#25676 = CARTESIAN_POINT ( 'NONE',  ( -20.47566338032530808, 25.06314818626709240, 16.24827550219793437 ) ) ;
#25677 = CARTESIAN_POINT ( 'NONE',  ( 2.263178113027038307, -138.7064940342181387, 43.59477710889679258 ) ) ;
#25678 = CARTESIAN_POINT ( 'NONE',  ( -24.53239521893651442, 16.68574937151015192, 29.54733954334095358 ) ) ;
#25679 = CARTESIAN_POINT ( 'NONE',  ( 109.1592201516379674, -0.003661068210032719476, 0.006957642258155058955 ) ) ;
#25680 = CARTESIAN_POINT ( 'NONE',  ( -20.21097721712958872, -28.05863618200116250, -9.464413111084637009 ) ) ;
#25681 = CARTESIAN_POINT ( 'NONE',  ( -1.058197053496177764, -44.07533330186778642, 12.47644286888561105 ) ) ;
#25682 = CARTESIAN_POINT ( 'NONE',  ( 2.430230287190589422, 133.5180086894991121, 57.85706160874191539 ) ) ;
#25683 = CARTESIAN_POINT ( 'NONE',  ( 109.1592201516379674, -0.006957642258146943919, 0.003661068210037270957 ) ) ;
#25684 = CARTESIAN_POINT ( 'NONE',  ( 25.64670758986457599, 12.29747533046116104, -112.2393466678476699 ) ) ;
#25685 = EDGE_LOOP ( 'NONE', ( #22729, #4820, #5411, #19468 ) ) ;
#25686 = VERTEX_POINT ( 'NONE', #8046 ) ;
#25687 = CARTESIAN_POINT ( 'NONE',  ( 1.834118845439484335, -141.9019470378989638, 30.34413640949651736 ) ) ;
#25688 = CARTESIAN_POINT ( 'NONE',  ( 109.1587776205901861, -0.005880209827414154510, 0.004375189885423086227 ) ) ;
#25689 = VERTEX_POINT ( 'NONE', #27876 ) ;
#25690 = ORIENTED_EDGE ( 'NONE', *, *, #18333, .T. ) ;
#25691 = ORIENTED_EDGE ( 'NONE', *, *, #4573, .T. ) ;
#25692 = EDGE_CURVE ( 'NONE', #21703, #7846, #19705, .T. ) ;
#25693 = CARTESIAN_POINT ( 'NONE',  ( -20.57838717382308147, 16.28767523336121315, -25.16001208503110931 ) ) ;
#25694 = EDGE_CURVE ( 'NONE', #19089, #11885, #27583, .T. ) ;
#25695 = LINE ( 'NONE', #21217, #1524 ) ;
#25696 = CARTESIAN_POINT ( 'NONE',  ( -20.24419206586952313, 7.929973069813410547, -28.55732805495818383 ) ) ;
#25697 = CARTESIAN_POINT ( 'NONE',  ( -12.82751273423880356, -6.573887447703164355, -48.43568301531138331 ) ) ;
#25698 = CARTESIAN_POINT ( 'NONE',  ( 109.1586059443104944, 0.003930911098393215057, 0.005881369279875419721 ) ) ;
#25699 = CARTESIAN_POINT ( 'NONE',  ( -1.155031165708891860, -44.25214473648919977, -12.20332162035446366 ) ) ;
#25700 = CARTESIAN_POINT ( 'NONE',  ( 55.49584447822657296, -29.26468316696729488, -66.38758986585143873 ) ) ;
#25701 = ORIENTED_EDGE ( 'NONE', *, *, #24787, .T. ) ;
#25702 = VERTEX_POINT ( 'NONE', #6017 ) ;
#25703 = CARTESIAN_POINT ( 'NONE',  ( 25.64703792032473828, -107.4308312803555339, -34.74993974077065673 ) ) ;
#25704 = CARTESIAN_POINT ( 'NONE',  ( -21.81686047589428057, -26.62923599424948407, 27.83628745321478704 ) ) ;
#25705 = CARTESIAN_POINT ( 'NONE',  ( -8.786685647604890903, -52.67761315067279781, 9.545808661481174795 ) ) ;
#25706 = CARTESIAN_POINT ( 'NONE',  ( 25.64681081121879203, 91.59071981940661544, -66.03065707438841514 ) ) ;
#25707 = ORIENTED_EDGE ( 'NONE', *, *, #25112, .T. ) ;
#25708 = CARTESIAN_POINT ( 'NONE',  ( -55.24728320129491266, -0.01402509393918509838, 0.003868537197316900683 ) ) ;
#25709 = DIRECTION ( 'NONE',  ( -0.7563875759206388771, -0.6320336713238522419, -0.1685564395263275950 ) ) ;
#25710 = CARTESIAN_POINT ( 'NONE',  ( 8.186469777910813761, -118.7566730872907499, 90.56875928602684667 ) ) ;
#25711 = VERTEX_POINT ( 'NONE', #1391 ) ;
#25712 = B_SPLINE_CURVE_WITH_KNOTS ( 'NONE', 3,
 ( #22653, #1043, #16001, #22500, #14120, #5062, #22941, #3063 ),
 .UNSPECIFIED., .F., .F.,
 ( 4, 2, 2, 4 ),
 ( 2.169948783056603995E-16, 0.002761568181852859429, 0.005523136363705502018, 0.01104627272741079240 ),
 .UNSPECIFIED. ) ;
#25713 = ORIENTED_EDGE ( 'NONE', *, *, #13205, .F. ) ;
#25714 = LINE ( 'NONE', #27722, #25495 ) ;
#25715 = ORIENTED_EDGE ( 'NONE', *, *, #9044, .T. ) ;
#25716 = ORIENTED_EDGE ( 'NONE', *, *, #14428, .F. ) ;
#25717 = CARTESIAN_POINT ( 'NONE',  ( 109.1592201516379674, -0.003476928926125439582, 0.007051465909551701133 ) ) ;
#25718 = EDGE_CURVE ( 'NONE', #20262, #14585, #10807, .T. ) ;
#25719 = EDGE_CURVE ( 'NONE', #13141, #3154, #2895, .T. ) ;
#25720 = EDGE_LOOP ( 'NONE', ( #13902, #17650, #25423, #6295 ) ) ;
#25721 = ITEM_DEFINED_TRANSFORMATION ( 'NONE', 'NONE', #21322,  #27263 ) ;
#25722 = CARTESIAN_POINT ( 'NONE',  ( 55.79472521941428198, 42.17269936297718402, -59.28412330436260191 ) ) ;
#25723 = CARTESIAN_POINT ( 'NONE',  ( 10.93730112725972425, -79.81734490845995822, 128.3908183996588264 ) ) ;
#25724 = CARTESIAN_POINT ( 'NONE',  ( 10.93730112726005999, 136.0306644680993600, -65.95960219662998725 ) ) ;
#25725 = DIRECTION ( 'NONE',  ( 1.000000000000000000, -6.938893903907226837E-18, 1.734723475976806709E-18 ) ) ;
#25726 = CARTESIAN_POINT ( 'NONE',  ( -28.13707043255157103, 14.07296284901332761, -18.06394523322457957 ) ) ;
#25727 = CARTESIAN_POINT ( 'NONE',  ( -24.53237795827033807, 22.94498492516385468, 24.99972053297880947 ) ) ;
#25728 = DIRECTION ( 'NONE',  ( -1.000000000000000000, -0.000000000000000000, -0.000000000000000000 ) ) ;
#25730 = CARTESIAN_POINT ( 'NONE',  ( -20.57838717382308147, -25.16001208503117326, -16.28767523336112433 ) ) ;
#25729 = DIRECTION ( 'NONE',  ( 0.5946245182733607137, 0.6521823330503020433, -0.4701913299128754331 ) ) ;
#25731 = LINE ( 'NONE', #3846, #10182 ) ;
#25732 = ORIENTED_EDGE ( 'NONE', *, *, #10839, .F. ) ;
#25733 = CARTESIAN_POINT ( 'NONE',  ( -1.583189561560256253, -2.490696082060189109, -46.33203782964460515 ) ) ;
#25734 = CARTESIAN_POINT ( 'NONE',  ( 109.1586900883932856, -0.0006456433529162976378, -0.007109207791181751390 ) ) ;
#25735 = DIRECTION ( 'NONE',  ( 0.000000000000000000, 0.000000000000000000, 1.000000000000000000 ) ) ;
#25736 = CARTESIAN_POINT ( 'NONE',  ( -8.786685647604898008, 48.22796981442802178, 23.24040270374343464 ) ) ;
#25737 = CARTESIAN_POINT ( 'NONE',  ( 2.063896406836609909, -126.4736179849642923, -71.46753739786147719 ) ) ;
#25738 = ORIENTED_EDGE ( 'NONE', *, *, #17788, .T. ) ;
#25739 = FACE_OUTER_BOUND ( 'NONE', #56, .T. ) ;
#25740 = CARTESIAN_POINT ( 'NONE',  ( -1.259920593601976613, -44.39818421957808425, 12.06711544331609609 ) ) ;
#25741 = EDGE_LOOP ( 'NONE', ( #2587, #1220, #2279, #25647 ) ) ;
#25742 = DIRECTION ( 'NONE',  ( -0.5914120900931443270, -0.3206367055789489662, 0.7398809652417994709 ) ) ;
#25743 = CARTESIAN_POINT ( 'NONE',  ( 180.4657679828686980, -1.252232817320263489E-15, 3.130582043300658722E-16 ) ) ;
#25744 = CARTESIAN_POINT ( 'NONE',  ( 25.64681081121879203, 75.24277141833491100, 84.18689316040072868 ) ) ;
#25745 = FACE_OUTER_BOUND ( 'NONE', #20813, .T. ) ;
#25746 = CARTESIAN_POINT ( 'NONE',  ( 8.186469829614448912, 113.2805153378652250, -97.33125097511772594 ) ) ;
#25747 = ORIENTED_EDGE ( 'NONE', *, *, #21882, .T. ) ;
#25748 = CARTESIAN_POINT ( 'NONE',  ( -9.156249394959713683, -53.90509764945124971, 8.027840202794504165 ) ) ;
#25749 = ADVANCED_FACE ( 'NONE', ( #1668 ), #14226, .F. ) ;
#25750 = CARTESIAN_POINT ( 'NONE',  ( 13.36082413113061307, -152.7944199136426846, -6.345145185219647210 ) ) ;
#25751 = EDGE_CURVE ( 'NONE', #13659, #8222, #8073, .T. ) ;
#25752 = ORIENTED_EDGE ( 'NONE', *, *, #13443, .T. ) ;
#25753 = CARTESIAN_POINT ( 'NONE',  ( -1.323830074806772839, 38.58891736138533446, -25.17121255494489418 ) ) ;
#25754 = B_SPLINE_CURVE_WITH_KNOTS ( 'NONE', 3,
 ( #1515, #12445, #1229, #23137, #16489, #16637, #21235, #21510 ),
 .UNSPECIFIED., .F., .F.,
 ( 4, 2, 2, 4 ),
 ( 2.214340075454938295E-16, 0.002761568181852865067, 0.005523136363705508090, 0.01104627272741079587 ),
 .UNSPECIFIED. ) ;
#25755 = ORIENTED_EDGE ( 'NONE', *, *, #13698, .T. ) ;
#25756 = EDGE_CURVE ( 'NONE', #19, #5056, #15041, .T. ) ;
#25757 = CARTESIAN_POINT ( 'NONE',  ( 28.37599760073042887, -91.75439000741646112, -68.88138253892495300 ) ) ;
#25758 = CARTESIAN_POINT ( 'NONE',  ( -20.37983603106074426, -7.753708011498764208, -28.74620395171560006 ) ) ;
#25759 = CARTESIAN_POINT ( 'NONE',  ( 13.36082413113063083, -67.94366799842725868, -137.0038452127807034 ) ) ;
#25760 = ADVANCED_FACE ( 'NONE', ( #2365 ), #20114, .F. ) ;
#25761 = CARTESIAN_POINT ( 'NONE',  ( -55.24198130335446422, -0.001516807524703878444, -0.009170435128245257514 ) ) ;
#25762 = CARTESIAN_POINT ( 'NONE',  ( -20.57838717382308147, 18.89542499756500149, -23.26537097894111383 ) ) ;
#25763 = CARTESIAN_POINT ( 'NONE',  ( -1.583189561560252701, 38.94740041318296164, -25.21827308671245760 ) ) ;
#25764 = CARTESIAN_POINT ( 'NONE',  ( 5.340103556456395673, 43.36842540065497786, 140.9275371673309110 ) ) ;
#25765 = CARTESIAN_POINT ( 'NONE',  ( -1.113548883309548376, -28.52482525634917820, 35.91246368318234516 ) ) ;
#25766 = CARTESIAN_POINT ( 'NONE',  ( 25.64708228042121618, 112.2968511928421123, -11.76327187353699344 ) ) ;
#25767 = CARTESIAN_POINT ( 'NONE',  ( 25.64704443564076541, 35.01840413910274208, -107.3436266109709862 ) ) ;
#25768 = ORIENTED_EDGE ( 'NONE', *, *, #19090, .F. ) ;
#25769 = CONICAL_SURFACE ( 'NONE', #23536, 117.6351876552689504, 0.9945805576725580410 ) ;
#25770 = ORIENTED_EDGE ( 'NONE', *, *, #15644, .T. ) ;
#25771 = DIRECTION ( 'NONE',  ( -1.000000000000000000, -0.000000000000000000, -0.000000000000000000 ) ) ;
#25772 = CARTESIAN_POINT ( 'NONE',  ( -1.044556982611269502, 15.70482750345296452, 43.01635920718332784 ) ) ;
#25773 = DIRECTION ( 'NONE',  ( 0.000000000000000000, 5.223019709708233256E-21, -1.000000000000000000 ) ) ;
#25774 = VECTOR ( 'NONE', #9720, 999.9999999999998863 ) ;
#25775 = DIRECTION ( 'NONE',  ( -0.7637818620346800147, -0.1788995134688828315, 0.6201872550346662072 ) ) ;
#25776 = CARTESIAN_POINT ( 'NONE',  ( -1.259920593601965066, 43.01175804832032412, 16.33409644610508238 ) ) ;
#25777 = CARTESIAN_POINT ( 'NONE',  ( 2.433796855181233454, 46.34326152018744693, 137.9325382748286870 ) ) ;
#25778 = CARTESIAN_POINT ( 'NONE',  ( 10.93730112725985926, -150.7858122213662853, 10.89264110824944609 ) ) ;
#25779 = ORIENTED_EDGE ( 'NONE', *, *, #8610, .T. ) ;
#25780 = CARTESIAN_POINT ( 'NONE',  ( 25.64681081121879203, -97.57530875170564855, -56.81519825470856944 ) ) ;
#25781 = CARTESIAN_POINT ( 'NONE',  ( 30.58324630866349736, -52.76949945162314748, -108.8243914523534812 ) ) ;
#25782 = VECTOR ( 'NONE', #27543, 1000.000000000000114 ) ;
#25783 = DIRECTION ( 'NONE',  ( 1.000000000000000000, -6.938893903907226837E-18, 1.734723475976806709E-18 ) ) ;
#25784 = DIRECTION ( 'NONE',  ( 1.000000000000000000, -6.938893903907226837E-18, 1.734723475976806709E-18 ) ) ;
#25785 = ORIENTED_EDGE ( 'NONE', *, *, #20372, .F. ) ;
#25786 = CARTESIAN_POINT ( 'NONE',  ( 25.64692872815576408, -46.21877827526630966, 103.0182448446672367 ) ) ;
#25787 = CARTESIAN_POINT ( 'NONE',  ( -5.986830583229484581, -11.27873876172107437, 49.46736940480268174 ) ) ;
#25788 = VERTEX_POINT ( 'NONE', #24135 ) ;
#25789 = EDGE_CURVE ( 'NONE', #27426, #8723, #28419, .T. ) ;
#25790 = ORIENTED_EDGE ( 'NONE', *, *, #14257, .T. ) ;
#25791 = VERTEX_POINT ( 'NONE', #11735 ) ;
#25792 = ADVANCED_FACE ( 'NONE', ( #17901 ), #2632, .F. ) ;
#25793 = CIRCLE ( 'NONE', #16580, 34.60786435723138510 ) ;
#25794 = CARTESIAN_POINT ( 'NONE',  ( 25.73574536432414206, -107.6875787074509105, 34.14219540448098655 ) ) ;
#25795 = VECTOR ( 'NONE', #4555, 1000.000000000000000 ) ;
#25796 = CARTESIAN_POINT ( 'NONE',  ( -55.25719721206881729, 0.01079965405819524257, -0.002847566758684156023 ) ) ;
#25797 = CARTESIAN_POINT ( 'NONE',  ( 109.1778270068192853, -0.007323887274071854900, -0.005755170886745502971 ) ) ;
#25798 = ORIENTED_EDGE ( 'NONE', *, *, #23852, .F. ) ;
#25799 = CARTESIAN_POINT ( 'NONE',  ( 2.063896406836605024, -43.61045647697596905, -138.5688025270883088 ) ) ;
#25800 = CARTESIAN_POINT ( 'NONE',  ( 32.73300124599732186, 0.000000000000000000, 0.000000000000000000 ) ) ;
#25801 = CARTESIAN_POINT ( 'NONE',  ( 0.000000000000000000, 0.000000000000000000, 0.000000000000000000 ) ) ;
#25802 = B_SPLINE_CURVE_WITH_KNOTS ( 'NONE', 3,
 ( #10854, #27977, #17312, #27843, #28246, #8141 ),
 .UNSPECIFIED., .F., .F.,
 ( 4, 2, 4 ),
 ( 4.679414566804424472E-16, 0.003576372551511269784, 0.007152745103022071192 ),
 .UNSPECIFIED. ) ;
#25803 = CARTESIAN_POINT ( 'NONE',  ( -8.786685647604896232, 52.67761315067299677, 9.545808661480061019 ) ) ;
#25804 = CARTESIAN_POINT ( 'NONE',  ( 8.186469829614019034, 127.5731248499976402, 77.65916164626368356 ) ) ;
#25805 = CARTESIAN_POINT ( 'NONE',  ( 9.884929003653626367, 85.04731144912678076, -124.2095058357569144 ) ) ;
#25806 = CIRCLE ( 'NONE', #18902, 34.60786435723138510 ) ;
#25807 = VECTOR ( 'NONE', #1393, 1000.000000000000000 ) ;
#25808 = CARTESIAN_POINT ( 'NONE',  ( 32.73300124599732186, 0.000000000000000000, 0.000000000000000000 ) ) ;
#25809 = DIRECTION ( 'NONE',  ( 1.000000000000000000, -0.000000000000000000, -0.000000000000000000 ) ) ;
#25810 = CARTESIAN_POINT ( 'NONE',  ( -21.41430102051752016, 28.68859753627394582, -11.22990201072285466 ) ) ;
#25811 = CARTESIAN_POINT ( 'NONE',  ( 16.05277956358200342, -141.0713346807233677, -25.20902801311519781 ) ) ;
#25812 = ORIENTED_EDGE ( 'NONE', *, *, #4246, .T. ) ;
#25813 = AXIS2_PLACEMENT_3D ( 'NONE', #25801, #8112, #14267 ) ;
#25814 = VERTEX_POINT ( 'NONE', #14454 ) ;
#25815 = CARTESIAN_POINT ( 'NONE',  ( -1.058473599757810746, 38.06357893967467731, 25.48501014712358881 ) ) ;
#25816 = DIRECTION ( 'NONE',  ( 0.5946245182733607137, 0.5357871896547409252, 0.5994612328333236428 ) ) ;
#25817 = ORIENTED_EDGE ( 'NONE', *, *, #18889, .F. ) ;
#25818 = EDGE_CURVE ( 'NONE', #2997, #15661, #4614, .T. ) ;
#25819 =( BOUNDED_SURFACE ( )  B_SPLINE_SURFACE ( 3, 1, ( 
 ( #12183, #20666 ),
 ( #5565, #5132 ),
 ( #9746, #24735 ),
 ( #7599, #18516 ) ),
 .UNSPECIFIED., .F., .F., .F. ) 
 B_SPLINE_SURFACE_WITH_KNOTS ( ( 4, 4 ),
 ( 2, 2 ),
 ( 0.000000000000000000, 1.000000000000000000 ),
 ( 0.000000000000000000, 1.000000000000000000 ),
 .UNSPECIFIED. ) 
 GEOMETRIC_REPRESENTATION_ITEM ( )  RATIONAL_B_SPLINE_SURFACE ( (
 ( 1.000000000000000000, 1.000000000000000000),
 ( 0.9934239774497838349, 0.8357310067453913582),
 ( 0.9934239774497838349, 0.8357310067453913582),
 ( 1.000000000000000000, 1.000000000000000000) ) ) 
 REPRESENTATION_ITEM ( '' )  SURFACE ( )  );
#25820 = ORIENTED_EDGE ( 'NONE', *, *, #21812, .T. ) ;
#25821 = ORIENTED_EDGE ( 'NONE', *, *, #1018, .T. ) ;
#25822 = EDGE_CURVE ( 'NONE', #7920, #23443, #1508, .T. ) ;
#25823 = EDGE_CURVE ( 'NONE', #14162, #7747, #21075, .T. ) ;
#25824 = CARTESIAN_POINT ( 'NONE',  ( 25.64670758986458310, -83.57526425215448285, -75.92149922855281829 ) ) ;
#25825 = VECTOR ( 'NONE', #27125, 1000.000000000000000 ) ;
#25826 = CARTESIAN_POINT ( 'NONE',  ( -20.90916690077961704, -27.35210456531395451, -28.59207721780137135 ) ) ;
#25827 = AXIS2_PLACEMENT_3D ( 'NONE', #1027, #25211, #24932 ) ;
#25828 = CARTESIAN_POINT ( 'NONE',  ( -20.38016308990359349, 27.81387210821422329, -10.62413300760995583 ) ) ;
#25829 = CARTESIAN_POINT ( 'NONE',  ( 30.59141879584292312, -84.53180090073624342, -79.74795589902120696 ) ) ;
#25830 = CARTESIAN_POINT ( 'NONE',  ( 26.11404676487259024, 45.01677474591551942, -103.8885755249565079 ) ) ;
#25831 = EDGE_CURVE ( 'NONE', #11014, #1503, #3605, .T. ) ;
#25832 = CARTESIAN_POINT ( 'NONE',  ( 25.87036335909427009, 102.8789780196095478, -46.88819766600006034 ) ) ;
#25833 = CARTESIAN_POINT ( 'NONE',  ( 25.69398547355839924, 112.9401428107247369, -0.7422864227369042611 ) ) ;
#25834 = ORIENTED_EDGE ( 'NONE', *, *, #7236, .F. ) ;
#25835 = ORIENTED_EDGE ( 'NONE', *, *, #3227, .T. ) ;
#25837 = CARTESIAN_POINT ( 'NONE',  ( -20.20700224038492721, -24.51628800869059432, -16.58740185276701951 ) ) ;
#25836 = CARTESIAN_POINT ( 'NONE',  ( 25.64703792032469920, 112.9111140735909373, -0.1487959541345440784 ) ) ;
#25838 = PRODUCT_RELATED_PRODUCT_CATEGORY ( 'part', '', ( #16651 ) ) ;
#25839 = CARTESIAN_POINT ( 'NONE',  ( -55.24198130335446422, -0.009190321388309828296, 0.001391250620101365347 ) ) ;
#25840 = CARTESIAN_POINT ( 'NONE',  ( 2.433796855181233454, -109.1007109081219539, -96.28145139437795308 ) ) ;
#25841 = CARTESIAN_POINT ( 'NONE',  ( -4.473127245936434626, 31.51789735524247504, 37.94261489385684882 ) ) ;
#25842 = EDGE_CURVE ( 'NONE', #14776, #14092, #1863, .T. ) ;
#25843 = ORIENTED_EDGE ( 'NONE', *, *, #13326, .T. ) ;
#25844 = CARTESIAN_POINT ( 'NONE',  ( 25.64681081121879203, 91.59071981940661544, -66.03065707438841514 ) ) ;
#25845 = CARTESIAN_POINT ( 'NONE',  ( 2.433796855181205476, -144.5536872373190818, -16.65276281464712582 ) ) ;
#25846 = CARTESIAN_POINT ( 'NONE',  ( 10.93730112725990367, -104.7670965581004054, -108.9902118373752842 ) ) ;
#25847 = ORIENTED_EDGE ( 'NONE', *, *, #28266, .T. ) ;
#25848 = ORIENTED_EDGE ( 'NONE', *, *, #2318, .T. ) ;
#25849 = ADVANCED_FACE ( 'NONE', ( #24382 ), #787, .F. ) ;
#25850 = DIRECTION ( 'NONE',  ( 0.000000000000000000, -5.223019709708190374E-21, 1.000000000000000000 ) ) ;
#25851 = AXIS2_PLACEMENT_3D ( 'NONE', #16748, #9686, #22950 ) ;
#25852 = ORIENTED_EDGE ( 'NONE', *, *, #4443, .T. ) ;
#25853 = VECTOR ( 'NONE', #15534, 1000.000000000000000 ) ;
#25854 = ORIENTED_EDGE ( 'NONE', *, *, #8850, .F. ) ;
#25855 = CARTESIAN_POINT ( 'NONE',  ( 1.893872463202057155, -14.22435552397911351, -144.4512189534318622 ) ) ;
#25856 = ORIENTED_EDGE ( 'NONE', *, *, #13514, .F. ) ;
#25857 = CARTESIAN_POINT ( 'NONE',  ( -23.77929240705206482, 31.93650644494365309, 17.17389748746929001 ) ) ;
#25858 = LINE ( 'NONE', #2212, #13838 ) ;
#25859 = CARTESIAN_POINT ( 'NONE',  ( -1.048994561756786625, 13.42228657661184954, 43.78680886990926524 ) ) ;
#25860 = CARTESIAN_POINT ( 'NONE',  ( 25.64681081121879203, 83.63051021305903987, 75.86069728269016821 ) ) ;
#25861 = CARTESIAN_POINT ( 'NONE',  ( 25.64681081121879203, 56.09509703373343115, 97.99105938547943140 ) ) ;
#25862 = CARTESIAN_POINT ( 'NONE',  ( 2.063896406836605024, -132.1577797566301911, -60.31174178979941303 ) ) ;
#25863 = VECTOR ( 'NONE', #23397, 1000.000000000000000 ) ;
#25864 = CARTESIAN_POINT ( 'NONE',  ( -55.24271866751342941, -0.006757859501009785483, 0.006671293903667892267 ) ) ;
#25865 = CARTESIAN_POINT ( 'NONE',  ( -1.045287976400365970, 45.76855895860943235, -1.530335034934267258 ) ) ;
#25866 = DIRECTION ( 'NONE',  ( 0.000000000000000000, 0.000000000000000000, 1.000000000000000000 ) ) ;
#25867 = CIRCLE ( 'NONE', #27695, 117.6351876552689504 ) ;
#25868 = EDGE_LOOP ( 'NONE', ( #2054, #11512, #26198, #16121 ) ) ;
#25869 = ORIENTED_EDGE ( 'NONE', *, *, #17505, .F. ) ;
#25870 = CARTESIAN_POINT ( 'NONE',  ( -8.786685647604889127, 9.545808661480615243, -52.67761315067287597 ) ) ;
#25871 = DIRECTION ( 'NONE',  ( 0.000000000000000000, 1.000000000000000000, 3.469446951953603342E-16 ) ) ;
#25872 = DIRECTION ( 'NONE',  ( -0.7637818620346801257, 0.3965875333584876761, 0.5092696688508626668 ) ) ;
#25873 = FACE_OUTER_BOUND ( 'NONE', #11118, .T. ) ;
#25874 = CARTESIAN_POINT ( 'NONE',  ( 8.186469777910586387, 102.4860666868860761, 108.6390983781759729 ) ) ;
#25875 = ORIENTED_EDGE ( 'NONE', *, *, #25831, .T. ) ;
#25876 = CARTESIAN_POINT ( 'NONE',  ( -21.41430102051751305, -19.54553566814603016, -23.81424706376357392 ) ) ;
#25877 = DIRECTION ( 'NONE',  ( 0.5946245182733608248, 0.3994439555666180475, 0.6977579871484577145 ) ) ;
#25878 = ADVANCED_FACE ( 'NONE', ( #26810 ), #5598, .F. ) ;
#25879 = ORIENTED_EDGE ( 'NONE', *, *, #13577, .T. ) ;
#25880 = CARTESIAN_POINT ( 'NONE',  ( 25.64700659047698039, -112.3162501909139905, 11.57609179463922899 ) ) ;
#25881 = CARTESIAN_POINT ( 'NONE',  ( 109.1586900883932856, -0.007137750914552287197, -0.0001010081143883916684 ) ) ;
#25882 = ADVANCED_FACE ( 'NONE', ( #20043 ), #23581, .T. ) ;
#25883 = CARTESIAN_POINT ( 'NONE',  ( 1.833485406944043827, 45.34878176254417070, -137.8414413349080974 ) ) ;
#25884 = CARTESIAN_POINT ( 'NONE',  ( 25.98107933586709350, -110.8834224379717597, 22.45325949158445411 ) ) ;
#25885 = CARTESIAN_POINT ( 'NONE',  ( 25.81918753295378011, -55.70247894228241137, 98.34688456803380063 ) ) ;
#25887 = ORIENTED_EDGE ( 'NONE', *, *, #6372, .F. ) ;
#25886 = ADVANCED_FACE ( 'NONE', ( #11554 ), #8533, .F. ) ;
#25888 = CARTESIAN_POINT ( 'NONE',  ( 6.224689322667630975, 28.26953958630619823, 145.3353551538642137 ) ) ;
#25889 = VECTOR ( 'NONE', #23939, 999.9999999999998863 ) ;
#25890 = CONICAL_SURFACE ( 'NONE', #21738, 34.60786435723138510, 0.8559913436420825139 ) ;
#25891 = CARTESIAN_POINT ( 'NONE',  ( 26.28373643307400087, 114.7784771129682895, -55.65614982951183265 ) ) ;
#25892 = B_SPLINE_CURVE_WITH_KNOTS ( 'NONE', 3,
 ( #3482, #1324, #7540, #16742, #4461, #16117 ),
 .UNSPECIFIED., .F., .F.,
 ( 4, 2, 4 ),
 ( 6.505213034913026604E-19, 0.0004335151646191473464, 0.0008670303292382940423 ),
 .UNSPECIFIED. ) ;
#25893 = ORIENTED_EDGE ( 'NONE', *, *, #6076, .T. ) ;
#25894 = CARTESIAN_POINT ( 'NONE',  ( -1.619063947482201282, 38.92136151114908671, -25.20140673341387227 ) ) ;
#25895 = AXIS2_PLACEMENT_3D ( 'NONE', #26357, #24216, #994 ) ;
#25896 = CARTESIAN_POINT ( 'NONE',  ( -18.41936578851710493, -5.707900577127883679, 42.05131332928132082 ) ) ;
#25897 = B_SPLINE_CURVE_WITH_KNOTS ( 'NONE', 3,
 ( #6795, #7087, #4616, #7227 ),
 .UNSPECIFIED., .F., .F.,
 ( 4, 4 ),
 ( 6.315918300066952003E-16, 0.008383748772660097257 ),
 .UNSPECIFIED. ) ;
#25898 = CARTESIAN_POINT ( 'NONE',  ( 25.64681081121880624, 102.9795863647034935, -46.30456157731225630 ) ) ;
#25899 = DIRECTION ( 'NONE',  ( -1.000000000000000000, -0.000000000000000000, -0.000000000000000000 ) ) ;
#25900 = CARTESIAN_POINT ( 'NONE',  ( -8.786685647604890903, -47.14957014837335691, 25.35688121747554291 ) ) ;
#25901 = B_SPLINE_CURVE_WITH_KNOTS ( 'NONE', 3,
 ( #6240, #3787, #23382, #23807, #27823, #8530, #16757 ),
 .UNSPECIFIED., .F., .F.,
 ( 4, 3, 4 ),
 ( 0.000000000000000000, 0.02398743853561357761, 0.04000277880656222251 ),
 .UNSPECIFIED. ) ;
#25902 = CARTESIAN_POINT ( 'NONE',  ( 55.79472521941428198, 63.36760613016223687, 35.74479459808869564 ) ) ;
#25903 = CARTESIAN_POINT ( 'NONE',  ( 28.37599760073043242, -108.5491283158099520, -37.15642189426513653 ) ) ;
#25904 = CARTESIAN_POINT ( 'NONE',  ( 30.58324630866338012, 21.27395054437408461, -119.0579156359856512 ) ) ;
#25905 = CARTESIAN_POINT ( 'NONE',  ( -4.473127245936434626, 45.82513704981544578, -18.25038884639885950 ) ) ;
#25906 = VECTOR ( 'NONE', #1727, 1000.000000000000114 ) ;
#25907 = CARTESIAN_POINT ( 'NONE',  ( -55.25719721206881729, 0.007063345920777610795, -0.008651607285660192076 ) ) ;
#25908 = CARTESIAN_POINT ( 'NONE',  ( 25.64660436782567032, -46.45435812945166987, -102.9120797476510774 ) ) ;
#25909 = CARTESIAN_POINT ( 'NONE',  ( -1.619063947482197729, -46.30105812165550105, -2.489035965909997206 ) ) ;
#25910 = VERTEX_POINT ( 'NONE', #6823 ) ;
#25911 = ADVANCED_FACE ( 'NONE', ( #15721 ), #12394, .F. ) ;
#25912 = ORIENTED_EDGE ( 'NONE', *, *, #26374, .F. ) ;
#25913 = CARTESIAN_POINT ( 'NONE',  ( -20.90916690077961348, 38.93431874629082756, 7.054312691028585824 ) ) ;
#25914 = CARTESIAN_POINT ( 'NONE',  ( -22.34422965417126861, 34.15536449444089584, -16.46028608106120572 ) ) ;
#25915 = CARTESIAN_POINT ( 'NONE',  ( -1.619063947482201282, 35.99532424477380488, -29.22875152547769062 ) ) ;
#25916 = CARTESIAN_POINT ( 'NONE',  ( 119.2224693531408803, -69.99999999999998579, 40.00000000000003553 ) ) ;
#25917 = CARTESIAN_POINT ( 'NONE',  ( -8.786685647604887350, 53.04920435127183254, -7.199674155859138835 ) ) ;
#25918 = CARTESIAN_POINT ( 'NONE',  ( -20.20700224038492365, 23.35150625415685255, 18.19058640100197977 ) ) ;
#25919 = CARTESIAN_POINT ( 'NONE',  ( -55.25297051322618813, -0.006313402748432862636, 0.01354497706059893877 ) ) ;
#25920 = ORIENTED_EDGE ( 'NONE', *, *, #17666, .T. ) ;
#25921 = CARTESIAN_POINT ( 'NONE',  ( 109.1587776205901577, -0.006729130500857921811, 0.002904816147418899739 ) ) ;
#25922 = CARTESIAN_POINT ( 'NONE',  ( 28.43349137099840718, -54.21282462801698188, -111.8014342888391184 ) ) ;
#25923 = VECTOR ( 'NONE', #24390, 1000.000000000000000 ) ;
#25924 = CARTESIAN_POINT ( 'NONE',  ( -1.046935749539995353, -36.28605774377782467, -27.93995161054682441 ) ) ;
#25925 = EDGE_CURVE ( 'NONE', #22173, #27786, #18317, .T. ) ;
#25926 = CARTESIAN_POINT ( 'NONE',  ( -20.20700224038492721, -28.44216453106542986, -8.199606986804219844 ) ) ;
#25927 = EDGE_CURVE ( 'NONE', #23545, #10869, #14564, .T. ) ;
#25928 = VERTEX_POINT ( 'NONE', #761 ) ;
#25929 = CARTESIAN_POINT ( 'NONE',  ( 25.64700659047696263, -112.2686754657454316, -12.02873506870284537 ) ) ;
#25930 = CARTESIAN_POINT ( 'NONE',  ( 94.22246935314088034, -151.1871800109700246, -6.938893903907228378E-15 ) ) ;
#25931 = ORIENTED_EDGE ( 'NONE', *, *, #25442, .F. ) ;
#25932 = ORIENTED_EDGE ( 'NONE', *, *, #26734, .F. ) ;
#25933 = ORIENTED_EDGE ( 'NONE', *, *, #3005, .T. ) ;
#25934 = CARTESIAN_POINT ( 'NONE',  ( 109.1592201516379674, -0.001331853079201447297, 0.007748443302134876837 ) ) ;
#25935 = CARTESIAN_POINT ( 'NONE',  ( 2.430230287190572103, 137.9371479820462696, 46.34481016236872364 ) ) ;
#25936 = CARTESIAN_POINT ( 'NONE',  ( 25.64681081121879203, -97.99105938547884875, -56.09509703373446854 ) ) ;
#25937 = CARTESIAN_POINT ( 'NONE',  ( 109.1592201516379674, -0.004194960840980736620, 0.006649399203953376171 ) ) ;
#25938 = ORIENTED_EDGE ( 'NONE', *, *, #19841, .T. ) ;
#25939 = CARTESIAN_POINT ( 'NONE',  ( -1.019300379054419725, 35.83762006677400791, -28.53917295602911253 ) ) ;
#25940 = EDGE_CURVE ( 'NONE', #7024, #26408, #6670, .T. ) ;
#25941 = B_SPLINE_CURVE_WITH_KNOTS ( 'NONE', 3,
 ( #4275, #26569, #2383, #6871, #15616, #9162, #20091, #6448, #17921, #24589 ),
 .UNSPECIFIED., .F., .F.,
 ( 4, 2, 2, 2, 4 ),
 ( 0.000000000000000000, 0.0003346267210630928380, 0.0006692534421261856761, 0.001003880163189278460, 0.001338506884252371352 ),
 .UNSPECIFIED. ) ;
#25942 = CARTESIAN_POINT ( 'NONE',  ( 109.1624594426973260, 0.01531968460305923631, -0.004489871836309145513 ) ) ;
#25943 = EDGE_CURVE ( 'NONE', #8211, #4083, #16593, .T. ) ;
#25944 = B_SPLINE_CURVE_WITH_KNOTS ( 'NONE', 3,
 ( #14767, #7607, #967, #9754, #5424, #14187, #3273, #19367, #28001, #25859, #2214, #17484, #21526 ),
 .UNSPECIFIED., .F., .F.,
 ( 4, 3, 3, 3, 4 ),
 ( 1.868354362588067661E-17, 0.0007657099931970537312, 0.001531419946797914168, 0.002296279302920151665, 0.003061450627205758099 ),
 .UNSPECIFIED. ) ;
#25945 = CARTESIAN_POINT ( 'NONE',  ( -1.583189561560253589, -29.24830400313191348, -36.01941156322777005 ) ) ;
#25946 = CARTESIAN_POINT ( 'NONE',  ( -1.046936909428679563, -1.275306677858562221, -45.77873603877005593 ) ) ;
#25947 = CARTESIAN_POINT ( 'NONE',  ( -4.178947244162647401, 41.47292084251672151, 25.96944194166747621 ) ) ;
#25948 = CARTESIAN_POINT ( 'NONE',  ( 1.833603222531972499, -141.8454679205784998, -30.60504697399356999 ) ) ;
#25949 = EDGE_CURVE ( 'NONE', #14622, #12565, #6015, .T. ) ;
#25950 = CARTESIAN_POINT ( 'NONE',  ( -20.20612091757422135, -10.22177757278296184, 27.77903622052264865 ) ) ;
#25951 = CARTESIAN_POINT ( 'NONE',  ( -22.23226125620943705, 29.33577758406451252, -11.82389163795220455 ) ) ;
#25952 = EDGE_CURVE ( 'NONE', #16681, #25814, #3797, .T. ) ;
#25953 = VERTEX_POINT ( 'NONE', #901 ) ;
#25954 = VERTEX_POINT ( 'NONE', #9989 ) ;
#25955 = CARTESIAN_POINT ( 'NONE',  ( -1.045287976400362417, 37.92705037016796155, 25.66401692419947977 ) ) ;
#25957 = EDGE_LOOP ( 'NONE', ( #27757, #6838 ) ) ;
#25956 = CARTESIAN_POINT ( 'NONE',  ( 28.37644542392847313, -34.54617949428011769, -119.4444529625693008 ) ) ;
#25958 = EDGE_LOOP ( 'NONE', ( #22619, #11766, #13505, #18586 ) ) ;
#25959 = VERTEX_POINT ( 'NONE', #18750 ) ;
#25960 = ORIENTED_EDGE ( 'NONE', *, *, #8578, .F. ) ;
#25961 = CARTESIAN_POINT ( 'NONE',  ( -1.056502255334264895, -26.51074901220476576, 37.35734037467662461 ) ) ;
#25962 = CARTESIAN_POINT ( 'NONE',  ( 28.37603512858445498, 75.42810021528217135, -86.45299531409385452 ) ) ;
#25963 = CARTESIAN_POINT ( 'NONE',  ( 32.73300124599738581, 84.80615050150476009, -81.52272205837115848 ) ) ;
#25964 = EDGE_CURVE ( 'NONE', #16059, #457, #15556, .T. ) ;
#25965 = CARTESIAN_POINT ( 'NONE',  ( 25.64681081121879203, -110.3564950173083474, 23.88203588908045916 ) ) ;
#25966 = CARTESIAN_POINT ( 'NONE',  ( -55.24390624410018802, -0.004572280736702649152, 0.009374879212966917563 ) ) ;
#25967 = CARTESIAN_POINT ( 'NONE',  ( 2.433796855181205476, -57.85512797797802165, -133.5135467655523769 ) ) ;
#25968 = CARTESIAN_POINT ( 'NONE',  ( 109.1586900883932856, 0.006130969560687363727, -0.003656351050331872743 ) ) ;
#25970 = ORIENTED_EDGE ( 'NONE', *, *, #13482, .T. ) ;
#25969 = EDGE_CURVE ( 'NONE', #24442, #14145, #25591, .T. ) ;
#25971 = VERTEX_POINT ( 'NONE', #7836 ) ;
#25973 = DIRECTION ( 'NONE',  ( 5.541455922705464902E-20, -5.223019709708320524E-21, 1.000000000000000000 ) ) ;
#25972 = CARTESIAN_POINT ( 'NONE',  ( 25.64681081121879203, 112.9102952884414464, -0.4157506337731811663 ) ) ;
#25974 = ADVANCED_FACE ( 'NONE', ( #25098 ), #21215, .F. ) ;
#25975 = CARTESIAN_POINT ( 'NONE',  ( -1.056502255334264895, 43.40574022158773460, -14.64009593116116292 ) ) ;
#25976 = CARTESIAN_POINT ( 'NONE',  ( 25.81918753295379432, 10.88546493099006618, -112.5005889664127494 ) ) ;
#25977 = CARTESIAN_POINT ( 'NONE',  ( 1.833485406944043827, 137.8414413349092058, -45.34878176254091642 ) ) ;
#25978 =( BOUNDED_SURFACE ( )  B_SPLINE_SURFACE ( 3, 1, ( 
 ( #9435, #22538 ),
 ( #16183, #16325 ),
 ( #27105, #24990 ),
 ( #18325, #2805 ) ),
 .UNSPECIFIED., .F., .F., .F. ) 
 B_SPLINE_SURFACE_WITH_KNOTS ( ( 4, 4 ),
 ( 2, 2 ),
 ( 0.000000000000000000, 1.000000000000000000 ),
 ( 0.000000000000000000, 1.000000000000000000 ),
 .UNSPECIFIED. ) 
 GEOMETRIC_REPRESENTATION_ITEM ( )  RATIONAL_B_SPLINE_SURFACE ( (
 ( 1.000000000000000000, 1.000000000000000000),
 ( 0.7789835883360576307, 0.9689951854195403280),
 ( 0.7789835883360576307, 0.9689951854195403280),
 ( 1.000000000000000000, 1.000000000000000000) ) ) 
 REPRESENTATION_ITEM ( '' )  SURFACE ( )  );
#25979 = ORIENTED_EDGE ( 'NONE', *, *, #23285, .F. ) ;
#25980 = CARTESIAN_POINT ( 'NONE',  ( 25.64692872815574987, 97.94438212068907035, -56.17679456083698142 ) ) ;
#25981 = CARTESIAN_POINT ( 'NONE',  ( -8.259864102781673267, -25.58601832199047266, 46.42816643551597622 ) ) ;
#25982 = CARTESIAN_POINT ( 'NONE',  ( 32.73300124599740002, -81.52272205837138586, -84.80615050150450429 ) ) ;
#25983 = ORIENTED_EDGE ( 'NONE', *, *, #21152, .T. ) ;
#25984 = VERTEX_POINT ( 'NONE', #5663 ) ;
#25985 = CARTESIAN_POINT ( 'NONE',  ( -2.904412668506660911, -11.97478724945543860, -46.12477647685269488 ) ) ;
#25986 = ORIENTED_EDGE ( 'NONE', *, *, #4413, .T. ) ;
#25987 = CARTESIAN_POINT ( 'NONE',  ( -20.90916690077964546, -35.64494649500671386, 17.17795951644694341 ) ) ;
#25988 = VERTEX_POINT ( 'NONE', #18611 ) ;
#25989 = B_SPLINE_CURVE_WITH_KNOTS ( 'NONE', 3,
 ( #17376, #20067, #2506, #26684 ),
 .UNSPECIFIED., .F., .F.,
 ( 4, 4 ),
 ( 0.000000000000000000, 0.01077107196513875376 ),
 .UNSPECIFIED. ) ;
#25990 = CARTESIAN_POINT ( 'NONE',  ( -6.574463467970655728, 34.08059230520098737, 38.37705091668339463 ) ) ;
#25991 = ORIENTED_EDGE ( 'NONE', *, *, #14506, .F. ) ;
#25992 = CARTESIAN_POINT ( 'NONE',  ( 109.1589550718174877, -0.002126635388725514868, -0.007270618150629025271 ) ) ;
#25993 = DIRECTION ( 'NONE',  ( -1.000000000000000000, -0.000000000000000000, -0.000000000000000000 ) ) ;
#25994 = CARTESIAN_POINT ( 'NONE',  ( 25.64660436782556374, -110.5628080555244708, -22.90783756890965961 ) ) ;
#25995 = CARTESIAN_POINT ( 'NONE',  ( 1.833485406944057594, 138.1714136985308699, 44.33323125129973619 ) ) ;
#25996 = CARTESIAN_POINT ( 'NONE',  ( -1.050231094221210082, 13.91061116148191878, -43.63617436699743024 ) ) ;
#25997 = CARTESIAN_POINT ( 'NONE',  ( 25.64670758986457955, -112.2393466678476983, -12.29747533046081998 ) ) ;
#25998 = EDGE_CURVE ( 'NONE', #17616, #8222, #27381, .T. ) ;
#25999 = CARTESIAN_POINT ( 'NONE',  ( -20.24399999263415140, 7.930419334766598993, 28.55700515887712854 ) ) ;
#26001 = CARTESIAN_POINT ( 'NONE',  ( -20.20700224038492721, 24.51628800869048419, -16.58740185276719359 ) ) ;
#26000 = CARTESIAN_POINT ( 'NONE',  ( 1.833838850093516770, 0.1779693352087572122, 145.1097630783160923 ) ) ;
#26002 = CARTESIAN_POINT ( 'NONE',  ( -1.619063947482197729, -2.489035965910479486, -46.30105812165547974 ) ) ;
#26004 = VERTEX_POINT ( 'NONE', #12141 ) ;
#26003 = EDGE_CURVE ( 'NONE', #14092, #987, #3915, .T. ) ;
#26005 = EDGE_LOOP ( 'NONE', ( #6982, #14424, #21483, #5647 ) ) ;
#26006 = CARTESIAN_POINT ( 'NONE',  ( 109.1589550718175161, -0.006445391216541674316, 0.003980125429509196594 ) ) ;
#26007 = CARTESIAN_POINT ( 'NONE',  ( 1.833750490713686787, -72.78591676344051109, 125.5350013574267649 ) ) ;
#26008 = CARTESIAN_POINT ( 'NONE',  ( -10.86508079875781263, 45.04061326950873223, -24.22249093393315533 ) ) ;
#26009 = ADVANCED_FACE ( 'NONE', ( #20907 ), #26749, .T. ) ;
#26010 = B_SPLINE_CURVE_WITH_KNOTS ( 'NONE', 3,
 ( #13003, #15427, #19906, #19753, #21642, #1915, #45, #19483, #21499, #17447, #24241, #4496, #15010 ),
 .UNSPECIFIED., .F., .F.,
 ( 4, 3, 3, 3, 4 ),
 ( 1.250926888277100149E-17, 0.0007657099931970565501, 0.001531419946797910915, 0.002296279302920149062, 0.003061450627205762869 ),
 .UNSPECIFIED. ) ;
#26011 = DIRECTION ( 'NONE',  ( 0.000000000000000000, 0.000000000000000000, -1.000000000000000000 ) ) ;
#26012 = CARTESIAN_POINT ( 'NONE',  ( 2.433796855181205476, 84.34988187690927930, 118.5671979538059730 ) ) ;
#26013 = CARTESIAN_POINT ( 'NONE',  ( -22.23342874802668234, -26.81018246605525590, 16.78332232459670337 ) ) ;
#26014 = VERTEX_POINT ( 'NONE', #22699 ) ;
#26015 = CARTESIAN_POINT ( 'NONE',  ( 32.73300124599736449, -117.3295799645430435, 8.473903470905730373 ) ) ;
#26016 =( BOUNDED_SURFACE ( )  B_SPLINE_SURFACE ( 3, 1, ( 
 ( #17739, #28383 ),
 ( #11272, #11131 ),
 ( #6531, #19903 ),
 ( #188, #8977 ) ),
 .UNSPECIFIED., .F., .F., .F. ) 
 B_SPLINE_SURFACE_WITH_KNOTS ( ( 4, 4 ),
 ( 2, 2 ),
 ( 0.000000000000000000, 1.000000000000000000 ),
 ( 0.000000000000000000, 1.000000000000000000 ),
 .UNSPECIFIED. ) 
 GEOMETRIC_REPRESENTATION_ITEM ( )  RATIONAL_B_SPLINE_SURFACE ( (
 ( 1.000000000000000000, 1.000000000000000000),
 ( 0.6386103224230316178, 0.9954351624131538845),
 ( 0.6386103224230316178, 0.9954351624131538845),
 ( 1.000000000000000000, 1.000000000000000000) ) ) 
 REPRESENTATION_ITEM ( '' )  SURFACE ( )  );
#26017 = CARTESIAN_POINT ( 'NONE',  ( -2.911734481061372115, -36.84482841982624990, 30.23325065583398441 ) ) ;
#26018 = CARTESIAN_POINT ( 'NONE',  ( 25.73574536432414561, -91.86645484851345600, 65.74844932374622886 ) ) ;
#26019 = CARTESIAN_POINT ( 'NONE',  ( 26.11404676487257603, -90.92995828888153653, -67.46175819463459788 ) ) ;
#26020 = ORIENTED_EDGE ( 'NONE', *, *, #992, .T. ) ;
#26021 = CARTESIAN_POINT ( 'NONE',  ( -55.25719721206881729, -0.01079965405819840671, -0.002847566758682798602 ) ) ;
#26022 = CARTESIAN_POINT ( 'NONE',  ( -8.259864102781675044, 52.06232470801727885, 9.986657004933084281 ) ) ;
#26023 = B_SPLINE_CURVE_WITH_KNOTS ( 'NONE', 3,
 ( #8910, #12928, #21720, #13076 ),
 .UNSPECIFIED., .F., .F.,
 ( 4, 4 ),
 ( 0.000000000000000000, 0.01077107196513875723 ),
 .UNSPECIFIED. ) ;
#26024 = VERTEX_POINT ( 'NONE', #9444 ) ;
#26025 = FACE_OUTER_BOUND ( 'NONE', #8631, .T. ) ;
#26026 = ORIENTED_EDGE ( 'NONE', *, *, #22788, .F. ) ;
#26027 = DIRECTION ( 'NONE',  ( 0.000000000000000000, 5.223019709707975211E-21, -1.000000000000000000 ) ) ;
#26028 = CARTESIAN_POINT ( 'NONE',  ( -7.762687761849950397E-17, 3.022826910523253725E-17, 44.74884827092600403 ) ) ;
#26029 = CARTESIAN_POINT ( 'NONE',  ( -90.83090735639699176, 0.000000000000000000, -37.50000000000001421 ) ) ;
#26030 = CARTESIAN_POINT ( 'NONE',  ( 109.1586059443104944, -0.001921075557418409560, 0.006808232911146182807 ) ) ;
#26031 = EDGE_CURVE ( 'NONE', #3338, #7920, #5279, .T. ) ;
#26032 = CARTESIAN_POINT ( 'NONE',  ( 8.186469777910859946, -145.3272523831805074, 34.43598809570094943 ) ) ;
#26033 = CARTESIAN_POINT ( 'NONE',  ( 119.2224693531408803, 70.00000000000004263, 39.99999999999999289 ) ) ;
#26034 = CARTESIAN_POINT ( 'NONE',  ( -20.20700224038492010, 27.82980252387833886, 10.08426345511560207 ) ) ;
#26035 = CARTESIAN_POINT ( 'NONE',  ( -1.050230347360791017, -0.0004630652115286125773, 45.79907861464602092 ) ) ;
#26036 = EDGE_CURVE ( 'NONE', #1993, #14040, #2967, .T. ) ;
#26037 = DIRECTION ( 'NONE',  ( -1.000000000000000000, -0.000000000000000000, -0.000000000000000000 ) ) ;
#26038 = DIRECTION ( 'NONE',  ( 1.000000000000000000, -6.938893903907226837E-18, 1.734723475976806709E-18 ) ) ;
#26039 = CARTESIAN_POINT ( 'NONE',  ( 10.93730112725996229, -20.69552240458240888, -149.7554878793151545 ) ) ;
#26040 = CARTESIAN_POINT ( 'NONE',  ( 25.64692232868534205, 34.58055111992187136, -107.4854307433083704 ) ) ;
#26041 = EDGE_LOOP ( 'NONE', ( #4059, #18133, #16986, #4485 ) ) ;
#26042 = ORIENTED_EDGE ( 'NONE', *, *, #22744, .T. ) ;
#26043 = ORIENTED_EDGE ( 'NONE', *, *, #8167, .T. ) ;
#26044 = CARTESIAN_POINT ( 'NONE',  ( 25.64708228042119842, 103.1335618347711574, 45.96113332231374926 ) ) ;
#26045 = B_SPLINE_CURVE_WITH_KNOTS ( 'NONE', 3,
 ( #21674, #10600, #1946, #26132, #19643, #10467, #6422 ),
 .UNSPECIFIED., .F., .F.,
 ( 4, 3, 4 ),
 ( 0.000000000000000000, 0.02398743853561336251, 0.04000277880656219476 ),
 .UNSPECIFIED. ) ;
#26046 = CARTESIAN_POINT ( 'NONE',  ( -20.37983603106073716, 1.508851015062576462, -29.73529213200292176 ) ) ;
#26047 = CARTESIAN_POINT ( 'NONE',  ( 109.1586059443104944, 0.004524147648825563653, -0.005438258427231146795 ) ) ;
#26048 = CARTESIAN_POINT ( 'NONE',  ( -1.045287976400351981, 43.05558670614237116, -15.59869763335110449 ) ) ;
#26049 = FACE_OUTER_BOUND ( 'NONE', #18931, .T. ) ;
#26050 = CARTESIAN_POINT ( 'NONE',  ( 28.43349137099831481, -46.80919715692979111, 115.0977416143055621 ) ) ;
#26051 = ORIENTED_EDGE ( 'NONE', *, *, #385, .F. ) ;
#26052 = CARTESIAN_POINT ( 'NONE',  ( 28.37603512858359522, 1.794342805482873171, 114.7183465482399640 ) ) ;
#26053 = CARTESIAN_POINT ( 'NONE',  ( 10.93730112725992676, -65.95960219663038515, -136.0306644680990473 ) ) ;
#26054 = CARTESIAN_POINT ( 'NONE',  ( 1.833721034905662295, 117.1867194831490480, -85.58110185769974976 ) ) ;
#26055 = DIRECTION ( 'NONE',  ( -0.7071067818211357325, 4.902845705138444274E-18, 0.7071067805519594129 ) ) ;
#26056 = ORIENTED_EDGE ( 'NONE', *, *, #2684, .F. ) ;
#26057 = CARTESIAN_POINT ( 'NONE',  ( 25.64708010899965274, -112.2984447178532577, -11.74803558238400036 ) ) ;
#26058 = LINE ( 'NONE', #23360, #1926 ) ;
#26059 = EDGE_LOOP ( 'NONE', ( #366, #27245, #1935, #28213 ) ) ;
#26060 = B_SPLINE_CURVE_WITH_KNOTS ( 'NONE', 3,
 ( #27178, #7487, #16251, #5166, #13943, #14083 ),
 .UNSPECIFIED., .F., .F.,
 ( 4, 2, 4 ),
 ( 0.000000000000000000, 0.0004335151646191536890, 0.0008670303292383073780 ),
 .UNSPECIFIED. ) ;
#26061 = VERTEX_POINT ( 'NONE', #18200 ) ;
#26062 = ORIENTED_EDGE ( 'NONE', *, *, #13679, .T. ) ;
#26063 = EDGE_CURVE ( 'NONE', #5582, #19356, #3246, .T. ) ;
#26064 = CARTESIAN_POINT ( 'NONE',  ( 2.063896406836609909, 96.20114399516543813, -108.8509294491455108 ) ) ;
#26065 = EDGE_CURVE ( 'NONE', #21162, #3526, #18011, .T. ) ;
#26066 = CARTESIAN_POINT ( 'NONE',  ( 28.37603512858451182, 65.97809844506251409, -93.86378016273907576 ) ) ;
#26067 = ADVANCED_FACE ( 'NONE', ( #20801 ), #6350, .F. ) ;
#26068 = DIRECTION ( 'NONE',  ( -1.000000000000000000, 6.938893903907226837E-18, -1.734723475976806709E-18 ) ) ;
#26069 = CARTESIAN_POINT ( 'NONE',  ( -55.24340739397742794, -0.008612749836242414997, -0.005344433640974251970 ) ) ;
#26070 = VERTEX_POINT ( 'NONE', #4968 ) ;
#26071 = CARTESIAN_POINT ( 'NONE',  ( 55.79472521941426777, 43.35047097963528273, -58.42842213658284578 ) ) ;
#26072 = CARTESIAN_POINT ( 'NONE',  ( -55.24198130335446422, 0.001391250620101877958, 0.009190321388310107587 ) ) ;
#26073 = B_SPLINE_CURVE_WITH_KNOTS ( 'NONE', 3,
 ( #12271, #9838, #14125, #9542, #22801, #1192, #27377, #3347 ),
 .UNSPECIFIED., .F., .F.,
 ( 4, 2, 2, 4 ),
 ( 0.000000000000000000, 0.0002429588503611127296, 0.0004859177007222254593, 0.0009718354014444932024 ),
 .UNSPECIFIED. ) ;
#26074 = CARTESIAN_POINT ( 'NONE',  ( 55.49584447822657296, 36.04376091928543246, 62.96491934286007108 ) ) ;
#26075 = DIRECTION ( 'NONE',  ( 0.5946245182733607137, -0.5955128528260776877, -0.5401723099040898202 ) ) ;
#26076 = CARTESIAN_POINT ( 'NONE',  ( 1.833838848569427027, 96.96512505224374934, -107.9566558236566749 ) ) ;
#26077 = CARTESIAN_POINT ( 'NONE',  ( 1.833750490713672132, -141.8829662951650903, -30.43107162406015576 ) ) ;
#26078 = CARTESIAN_POINT ( 'NONE',  ( 10.93730112725972070, -4.928439153521261495, 151.0983828010090804 ) ) ;
#26079 = LINE ( 'NONE', #21341, #25889 ) ;
#26080 = CARTESIAN_POINT ( 'NONE',  ( -20.57838717382308147, -16.28767523336139078, -25.16001208503099917 ) ) ;
#26081 = ORIENTED_EDGE ( 'NONE', *, *, #4351, .T. ) ;
#26082 = VERTEX_POINT ( 'NONE', #5401 ) ;
#26083 = CARTESIAN_POINT ( 'NONE',  ( 1.834118845439484335, 15.34511559672872671, -144.2964192726480519 ) ) ;
#26084 = DIRECTION ( 'NONE',  ( 0.7563875759206388771, -0.5490129373055229189, 0.3556158456312960015 ) ) ;
#26085 = VERTEX_POINT ( 'NONE', #18338 ) ;
#26086 = ORIENTED_EDGE ( 'NONE', *, *, #1632, .F. ) ;
#26087 = ORIENTED_EDGE ( 'NONE', *, *, #193, .F. ) ;
#26088 = EDGE_CURVE ( 'NONE', #10527, #12534, #5656, .T. ) ;
#26089 = EDGE_CURVE ( 'NONE', #4782, #16696, #22842, .T. ) ;
#26090 = ADVANCED_BREP_SHAPE_REPRESENTATION ( '', ( #8673, #27263 ), #16248 ) ;
#26091 = B_SPLINE_CURVE_WITH_KNOTS ( 'NONE', 3,
 ( #2641, #18033, #15885, #9850 ),
 .UNSPECIFIED., .F., .F.,
 ( 4, 4 ),
 ( 1.906343156168367839E-16, 0.0009910334943225120648 ),
 .UNSPECIFIED. ) ;
#26092 = CARTESIAN_POINT ( 'NONE',  ( 14.74894986621300141, -1.023413983156987271E-16, 2.558534957892468177E-17 ) ) ;
#26093 = EDGE_CURVE ( 'NONE', #25791, #17323, #22099, .T. ) ;
#26094 = CARTESIAN_POINT ( 'NONE',  ( -23.79223135445720771, 28.60983116549966354, -16.82181692922826599 ) ) ;
#26095 = CARTESIAN_POINT ( 'NONE',  ( 109.1721716018069515, 0.01157047143378738159, -0.01254847260354039276 ) ) ;
#26096 = EDGE_CURVE ( 'NONE', #14998, #7877, #25229, .T. ) ;
#26097 = CARTESIAN_POINT ( 'NONE',  ( 55.79472521941428198, -69.41463258328498398, -21.78881894124774732 ) ) ;
#26098 = CARTESIAN_POINT ( 'NONE',  ( 8.186469777910478030, 149.3111477498015631, -3.468244369822261142 ) ) ;
#26099 = CARTESIAN_POINT ( 'NONE',  ( -18.41936578851706230, 42.05131332928132082, 5.707900577128324215 ) ) ;
#26100 = CARTESIAN_POINT ( 'NONE',  ( -20.90916690077963125, 18.74041620980169043, -34.84883504600955462 ) ) ;
#26101 = CARTESIAN_POINT ( 'NONE',  ( 25.64660436782576625, 102.9120797476511626, -46.45435812945127196 ) ) ;
#26102 = CARTESIAN_POINT ( 'NONE',  ( 28.37644542392849800, -65.64862111872122341, 105.5967537682339668 ) ) ;
#26103 = CIRCLE ( 'NONE', #6824, 53.53553390275978785 ) ;
#26104 = VERTEX_POINT ( 'NONE', #26843 ) ;
#26105 = EDGE_LOOP ( 'NONE', ( #16317, #16898, #19417, #10354 ) ) ;
#26106 = CARTESIAN_POINT ( 'NONE',  ( 25.64681081121879203, 91.59071981940572016, 66.03065707438965148 ) ) ;
#26107 = CARTESIAN_POINT ( 'NONE',  ( -55.24271866751342941, -0.006671293903668846365, 0.006757859501006202411 ) ) ;
#26108 = B_SPLINE_CURVE_WITH_KNOTS ( 'NONE', 3,
 ( #8865, #23991, #19224, #6010, #6563, #4244 ),
 .UNSPECIFIED., .F., .F.,
 ( 4, 2, 4 ),
 ( 0.000000000000000000, 0.0006311636237756768509, 0.001262327247551353702 ),
 .UNSPECIFIED. ) ;
#26109 = CARTESIAN_POINT ( 'NONE',  ( -9.156249394959706578, 38.89149400288462033, 38.17928057391947760 ) ) ;
#26110 = CARTESIAN_POINT ( 'NONE',  ( 109.1624594426973118, 0.002129375066974254459, 0.01582142368019177209 ) ) ;
#26111 = CARTESIAN_POINT ( 'NONE',  ( -20.57838717382308147, -25.16001208503093522, 16.28767523336148315 ) ) ;
#26112 = ORIENTED_EDGE ( 'NONE', *, *, #4099, .T. ) ;
#26113 = CARTESIAN_POINT ( 'NONE',  ( -8.786685647604889127, 9.545808661480615243, -52.67761315067287597 ) ) ;
#26114 = DIRECTION ( 'NONE',  ( -0.5946245182733608248, 0.7870422510449656128, 0.1642747008466218794 ) ) ;
#26115 = CARTESIAN_POINT ( 'NONE',  ( 1.833485406944043827, -108.1939177044932592, 96.69979900902130510 ) ) ;
#26116 = VERTEX_POINT ( 'NONE', #7152 ) ;
#26117 = ORIENTED_EDGE ( 'NONE', *, *, #15791, .T. ) ;
#26118 = CARTESIAN_POINT ( 'NONE',  ( -1.031422197589716205, 12.69107518035502835, -44.01264471863851924 ) ) ;
#26119 = CARTESIAN_POINT ( 'NONE',  ( -21.41427618760446094, -1.815001260755626733, 30.75468365310880259 ) ) ;
#26120 = EDGE_LOOP ( 'NONE', ( #19191, #3887, #13802, #4853 ) ) ;
#26121 = EDGE_CURVE ( 'NONE', #20961, #17579, #7028, .T. ) ;
#26122 = CARTESIAN_POINT ( 'NONE',  ( -23.79248802219730052, 16.82188324679482605, -28.61009539422389381 ) ) ;
#26123 = CIRCLE ( 'NONE', #8234, 34.60786435723138510 ) ;
#26124 = EDGE_LOOP ( 'NONE', ( #23423, #507 ) ) ;
#26125 = EDGE_CURVE ( 'NONE', #3474, #12622, #27246, .T. ) ;
#26126 = CARTESIAN_POINT ( 'NONE',  ( 24.01988960052053201, 127.2243989116375076, 31.41104197353366345 ) ) ;
#26127 = CARTESIAN_POINT ( 'NONE',  ( 2.433796855181205476, 142.6247129145651797, -28.83182736670396196 ) ) ;
#26128 = CARTESIAN_POINT ( 'NONE',  ( 2.078045971014549723E-18, -1.958632391140620919E-19, 37.50000000000001421 ) ) ;
#26129 = FACE_OUTER_BOUND ( 'NONE', #19357, .T. ) ;
#26130 = CARTESIAN_POINT ( 'NONE',  ( -8.786685647604720373, -47.14957014837338534, -25.35688121747513435 ) ) ;
#26131 = CARTESIAN_POINT ( 'NONE',  ( -1.046936909428696882, 12.93351869073272908, -43.93225665392618851 ) ) ;
#26132 = CARTESIAN_POINT ( 'NONE',  ( 19.66333377628716050, -9.924285918885514590, -137.3914191246404357 ) ) ;
#26133 =( BOUNDED_SURFACE ( )  B_SPLINE_SURFACE ( 3, 1, ( 
 ( #24159, #17372 ),
 ( #28173, #4419 ),
 ( #24441, #21705 ),
 ( #2244, #28308 ) ),
 .UNSPECIFIED., .F., .F., .F. ) 
 B_SPLINE_SURFACE_WITH_KNOTS ( ( 4, 4 ),
 ( 2, 2 ),
 ( 0.000000000000000000, 1.000000000000000000 ),
 ( 0.000000000000000000, 1.000000000000000000 ),
 .UNSPECIFIED. ) 
 GEOMETRIC_REPRESENTATION_ITEM ( )  RATIONAL_B_SPLINE_SURFACE ( (
 ( 1.000000000000000000, 1.000000000000000000),
 ( 0.9956975270656954757, 0.8568959468854893125),
 ( 0.9956975270656954757, 0.8568959468854893125),
 ( 1.000000000000000000, 1.000000000000000000) ) ) 
 REPRESENTATION_ITEM ( '' )  SURFACE ( )  );
#26134 = CARTESIAN_POINT ( 'NONE',  ( 1.833721034905647418, 125.8463597577927118, 72.24642519953816588 ) ) ;
#26136 = CARTESIAN_POINT ( 'NONE',  ( -22.23342874802670011, -31.55488258420090375, -2.180636882146402833 ) ) ;
#26135 = CARTESIAN_POINT ( 'NONE',  ( 1.831572820252008738, -14.18623102066671038, -144.4165162501764428 ) ) ;
#26137 = CARTESIAN_POINT ( 'NONE',  ( 25.81918753295380142, -112.3053965977762374, 12.74259626488116126 ) ) ;
#26138 = ORIENTED_EDGE ( 'NONE', *, *, #23226, .T. ) ;
#26139 = ORIENTED_EDGE ( 'NONE', *, *, #1745, .F. ) ;
#26140 = CARTESIAN_POINT ( 'NONE',  ( 32.73300124599734318, 113.0038235389602477, 32.68291970228275289 ) ) ;
#26141 = CARTESIAN_POINT ( 'NONE',  ( 2.108985857320944124, 118.2933707022557570, 84.36123201973842356 ) ) ;
#26142 = CARTESIAN_POINT ( 'NONE',  ( 26.11404676487257603, 84.89295829319495112, 74.91683232331003239 ) ) ;
#26143 = CARTESIAN_POINT ( 'NONE',  ( 8.186469829614438254, 102.4860667297611769, -108.6390983847740301 ) ) ;
#26144 = B_SPLINE_CURVE_WITH_KNOTS ( 'NONE', 3,
 ( #16937, #19514, #2082, #25999, #3843, #1803 ),
 .UNSPECIFIED., .F., .F.,
 ( 4, 2, 4 ),
 ( 4.906538933386797396E-18, 0.0004335151646191504906, 0.0008670303292382959938 ),
 .UNSPECIFIED. ) ;
#26145 = DIRECTION ( 'NONE',  ( 0.000000000000000000, 1.000000000000000000, 0.000000000000000000 ) ) ;
#26146 = CARTESIAN_POINT ( 'NONE',  ( 2.433796855181205476, -137.9325382748282038, -46.34326152018883249 ) ) ;
#26147 = B_SPLINE_CURVE_WITH_KNOTS ( 'NONE', 3,
 ( #5302, #27017, #18550, #27317, #22891, #27171, #16384, #14076 ),
 .UNSPECIFIED., .F., .F.,
 ( 4, 2, 2, 4 ),
 ( 2.196627850418165012E-16, 0.002761568181852864633, 0.005523136363705508957, 0.01104627272741078546 ),
 .UNSPECIFIED. ) ;
#26148 = ORIENTED_EDGE ( 'NONE', *, *, #18065, .F. ) ;
#26149 = CARTESIAN_POINT ( 'NONE',  ( -1.031422197589711764, -1.530725436377143867, 45.78027046666444022 ) ) ;
#26150 = CARTESIAN_POINT ( 'NONE',  ( 2.063896406836605024, 31.51663808384751775, -141.8093313989357682 ) ) ;
#26151 = FACE_OUTER_BOUND ( 'NONE', #17295, .T. ) ;
#26152 = CARTESIAN_POINT ( 'NONE',  ( 55.49584447822657296, 72.18163437663939419, 7.317474139115872411 ) ) ;
#26153 = CARTESIAN_POINT ( 'NONE',  ( 1.833206308920094285, -45.54896581797555655, 137.7753864329223745 ) ) ;
#26154 = VERTEX_POINT ( 'NONE', #21646 ) ;
#26155 = CARTESIAN_POINT ( 'NONE',  ( 2.063896406836605024, 28.88716984836320023, 142.3682421260908484 ) ) ;
#26156 = CARTESIAN_POINT ( 'NONE',  ( 1.833838850093465700, 15.16809710532252886, -144.3148369740566181 ) ) ;
#26157 = EDGE_CURVE ( 'NONE', #2848, #9399, #14460, .T. ) ;
#26158 = ORIENTED_EDGE ( 'NONE', *, *, #17337, .T. ) ;
#26159 = CARTESIAN_POINT ( 'NONE',  ( 25.64660436782546427, 112.2303901742709797, -12.37913844082926573 ) ) ;
#26160 = ADVANCED_FACE ( 'NONE', ( #4085 ), #1554, .F. ) ;
#26161 = LINE ( 'NONE', #11047, #7401 ) ;
#26162 = DIRECTION ( 'NONE',  ( 1.000000000000000000, 0.000000000000000000, 0.000000000000000000 ) ) ;
#26163 = ADVANCED_FACE ( 'NONE', ( #25425 ), #5640, .T. ) ;
#26164 = CARTESIAN_POINT ( 'NONE',  ( -1.539760825549682632, -11.93465943778483584, 44.72358953107743673 ) ) ;
#26165 = FACE_OUTER_BOUND ( 'NONE', #12716, .T. ) ;
#26166 = CARTESIAN_POINT ( 'NONE',  ( -20.57838717382308147, -10.78122205916981358, 27.96569011373096814 ) ) ;
#26167 = CARTESIAN_POINT ( 'NONE',  ( 25.73574536432416693, 46.68445899255630849, -102.8730547980545538 ) ) ;
#26168 = CARTESIAN_POINT ( 'NONE',  ( 2.433796855181233454, -138.8296532063085351, -43.58222566461785163 ) ) ;
#26169 = CARTESIAN_POINT ( 'NONE',  ( 10.93730112725943471, 119.3442956573271516, 92.80059208661684522 ) ) ;
#26170 = CARTESIAN_POINT ( 'NONE',  ( -1.050230347699840694, -0.0002315326057593219944, 45.79907861674081460 ) ) ;
#26171 = CARTESIAN_POINT ( 'NONE',  ( 25.87036335909426654, 110.7910326764402953, 22.53739730344084080 ) ) ;
#26172 = CARTESIAN_POINT ( 'NONE',  ( -23.77929240705206126, -6.464423883190137055, 35.68044874544703049 ) ) ;
#26173 = CARTESIAN_POINT ( 'NONE',  ( 13.36082413113061307, -6.345145185219113415, 152.7944199136427130 ) ) ;
#26174 = CARTESIAN_POINT ( 'NONE',  ( 109.1592201516379674, 0.001127733110588118211, 0.007780772729122761334 ) ) ;
#26175 = VERTEX_POINT ( 'NONE', #12718 ) ;
#26176 =( BOUNDED_SURFACE ( )  B_SPLINE_SURFACE ( 3, 1, ( 
 ( #20143, #430 ),
 ( #17973, #24641 ),
 ( #4894, #22617 ),
 ( #11661, #26904 ) ),
 .UNSPECIFIED., .F., .F., .F. ) 
 B_SPLINE_SURFACE_WITH_KNOTS ( ( 4, 4 ),
 ( 2, 2 ),
 ( 0.000000000000000000, 1.000000000000000000 ),
 ( 0.000000000000000000, 1.000000000000000000 ),
 .UNSPECIFIED. ) 
 GEOMETRIC_REPRESENTATION_ITEM ( )  RATIONAL_B_SPLINE_SURFACE ( (
 ( 1.000000000000000000, 1.000000000000000000),
 ( 0.9956975270656954757, 0.8568959468854893125),
 ( 0.9956975270656954757, 0.8568959468854893125),
 ( 1.000000000000000000, 1.000000000000000000) ) ) 
 REPRESENTATION_ITEM ( '' )  SURFACE ( )  );
#26177 = ORIENTED_EDGE ( 'NONE', *, *, #19438, .T. ) ;
#26178 = CARTESIAN_POINT ( 'NONE',  ( -20.20612092514784308, -29.57813644637189299, 1.137292630518367265 ) ) ;
#26179 = CARTESIAN_POINT ( 'NONE',  ( 26.28373643307404706, -114.7784771129677637, 55.65614982951248635 ) ) ;
#26180 = CARTESIAN_POINT ( 'NONE',  ( 109.1586900883932856, -0.006819617742893414360, -0.002109621908814778967 ) ) ;
#26181 = CARTESIAN_POINT ( 'NONE',  ( 2.433796855181205476, -142.0211193075553524, -31.67151202413115385 ) ) ;
#26182 = CARTESIAN_POINT ( 'NONE',  ( 30.58324630866342986, -41.10517620771124570, -113.7441547345751616 ) ) ;
#26183 = DIRECTION ( 'NONE',  ( -0.5914120900931443270, -0.5938529060132696769, 0.5455001977188030926 ) ) ;
#26184 = CARTESIAN_POINT ( 'NONE',  ( -1.048994561756802391, 27.53485040342894408, -36.59609844253136401 ) ) ;
#26185 = ORIENTED_EDGE ( 'NONE', *, *, #27846, .T. ) ;
#26186 = CARTESIAN_POINT ( 'NONE',  ( 25.86096068574579476, -33.98552076022123458, -107.8247115223745283 ) ) ;
#26187 = CARTESIAN_POINT ( 'NONE',  ( 2.430230287190572103, 57.85706160874143933, 133.5180086894993110 ) ) ;
#26188 = CARTESIAN_POINT ( 'NONE',  ( 1.833809397773872307, 117.5007887865419320, -85.14934054436353961 ) ) ;
#26189 = CARTESIAN_POINT ( 'NONE',  ( -20.21097721650788159, -28.26295598655178765, -8.835581399095051580 ) ) ;
#26190 = CARTESIAN_POINT ( 'NONE',  ( 9.884929003653608603, -78.87917189085001723, 128.2151425008039212 ) ) ;
#26191 = EDGE_CURVE ( 'NONE', #20564, #12449, #22481, .T. ) ;
#26192 = EDGE_LOOP ( 'NONE', ( #11261, #4179, #13635, #9365 ) ) ;
#26193 = CARTESIAN_POINT ( 'NONE',  ( 1.894214914920961057, -45.75988301372547085, -137.7482714433628530 ) ) ;
#26194 = CARTESIAN_POINT ( 'NONE',  ( 1.833838850093440387, -117.3962664098817754, -85.29337590730665397 ) ) ;
#26195 = VERTEX_POINT ( 'NONE', #21073 ) ;
#26196 = EDGE_CURVE ( 'NONE', #18732, #12739, #15930, .T. ) ;
#26197 = ORIENTED_EDGE ( 'NONE', *, *, #5315, .T. ) ;
#26198 = ORIENTED_EDGE ( 'NONE', *, *, #140, .T. ) ;
#26199 = CARTESIAN_POINT ( 'NONE',  ( 30.58324630866342630, -33.60235057864056074, 116.1819705588612095 ) ) ;
#26200 = CARTESIAN_POINT ( 'NONE',  ( -9.156249394959706578, -8.027840202793560920, 53.90509764945136340 ) ) ;
#26201 = CARTESIAN_POINT ( 'NONE',  ( -4.473127245936431073, -37.94261489385741015, -31.51789735524179648 ) ) ;
#26202 = AXIS2_PLACEMENT_3D ( 'NONE', #4182, #6353, #8942 ) ;
#26203 = CARTESIAN_POINT ( 'NONE',  ( 109.1592201516379674, -0.006957642258146943919, 0.003661068210037270957 ) ) ;
#26204 = ORIENTED_EDGE ( 'NONE', *, *, #11938, .T. ) ;
#26205 = CARTESIAN_POINT ( 'NONE',  ( -1.048996300304493978, -43.78665266739846373, -13.42280206896960060 ) ) ;
#26206 = B_SPLINE_CURVE_WITH_KNOTS ( 'NONE', 3,
 ( #28288, #17219, #28152, #26141, #6297, #14779 ),
 .UNSPECIFIED., .F., .F.,
 ( 4, 2, 4 ),
 ( 1.388456241783856658E-17, 0.0006311571484586121859, 0.001262314296917210711 ),
 .UNSPECIFIED. ) ;
#26207 = CARTESIAN_POINT ( 'NONE',  ( -55.24390624410018802, -0.001811362924362171613, 0.01027195578988007209 ) ) ;
#26208 = CARTESIAN_POINT ( 'NONE',  ( 1.832998868059858122, -144.3700883710216090, -14.63705790014155816 ) ) ;
#26209 = CARTESIAN_POINT ( 'NONE',  ( 26.11404676487257603, 113.2169081140373947, 1.130420376097532653 ) ) ;
#26210 = CARTESIAN_POINT ( 'NONE',  ( 6.224689322667630975, -84.93872395422891941, -121.2721959030546657 ) ) ;
#26211 = CARTESIAN_POINT ( 'NONE',  ( 119.2224693531408803, -69.99999999999998579, 40.00000000000003553 ) ) ;
#26212 = CARTESIAN_POINT ( 'NONE',  ( -1.239374126674604337, -38.61989855450958231, -25.08410696974230092 ) ) ;
#26213 =( BOUNDED_SURFACE ( )  B_SPLINE_SURFACE ( 3, 1, ( 
 ( #23924, #24201 ),
 ( #24337, #26064 ),
 ( #4044, #19300 ),
 ( #17555, #2017 ) ),
 .UNSPECIFIED., .F., .F., .F. ) 
 B_SPLINE_SURFACE_WITH_KNOTS ( ( 4, 4 ),
 ( 2, 2 ),
 ( 0.000000000000000000, 1.000000000000000000 ),
 ( 0.000000000000000000, 1.000000000000000000 ),
 .UNSPECIFIED. ) 
 GEOMETRIC_REPRESENTATION_ITEM ( )  RATIONAL_B_SPLINE_SURFACE ( (
 ( 1.000000000000000000, 1.000000000000000000),
 ( 0.9956975270656954757, 0.8568959468854893125),
 ( 0.9956975270656954757, 0.8568959468854893125),
 ( 1.000000000000000000, 1.000000000000000000) ) ) 
 REPRESENTATION_ITEM ( '' )  SURFACE ( )  );
#26214 = EDGE_CURVE ( 'NONE', #12942, #7524, #17660, .T. ) ;
#26215 = ORIENTED_EDGE ( 'NONE', *, *, #9009, .T. ) ;
#26216 = EDGE_CURVE ( 'NONE', #26384, #12090, #4952, .T. ) ;
#26217 = ORIENTED_EDGE ( 'NONE', *, *, #5174, .F. ) ;
#26218 = CARTESIAN_POINT ( 'NONE',  ( -2.911734481061388990, -47.57875121082950898, 2.802366807346684308 ) ) ;
#26219 = CIRCLE ( 'NONE', #18408, 117.6351876552689504 ) ;
#26220 = CARTESIAN_POINT ( 'NONE',  ( 25.64681081121880624, 35.28660243342550729, 107.2555980796242494 ) ) ;
#26221 = VERTEX_POINT ( 'NONE', #13568 ) ;
#26222 = CONICAL_SURFACE ( 'NONE', #21177, 117.6351876552689504, 0.9945805576725580410 ) ;
#26223 = VERTEX_POINT ( 'NONE', #17603 ) ;
#26224 = ORIENTED_EDGE ( 'NONE', *, *, #15387, .T. ) ;
#26225 = CIRCLE ( 'NONE', #13817, 53.53553390275978785 ) ;
#26226 = B_SPLINE_CURVE_WITH_KNOTS ( 'NONE', 3,
 ( #7567, #9166, #15483, #6874 ),
 .UNSPECIFIED., .F., .F.,
 ( 4, 4 ),
 ( 6.938893903907227607E-18, 0.008383560773332725952 ),
 .UNSPECIFIED. ) ;
#26227 = PRODUCT_DEFINITION_SHAPE ( 'NONE', 'NONE',  #28439 ) ;
#26228 = DIRECTION ( 'NONE',  ( -0.5914120900931443270, 0.3206367055789539067, -0.7398809652417974725 ) ) ;
#26229 = CARTESIAN_POINT ( 'NONE',  ( 2.433796855181233454, -144.8571464219888298, -13.76554153471842312 ) ) ;
#26230 = DIRECTION ( 'NONE',  ( 0.000000000000000000, 5.223019709708233256E-21, -1.000000000000000000 ) ) ;
#26231 = CARTESIAN_POINT ( 'NONE',  ( -55.24728320129491266, 0.01402509393918179546, 0.003868537197316780987 ) ) ;
#26232 = CIRCLE ( 'NONE', #15637, 53.53553390275978785 ) ;
#26233 = CARTESIAN_POINT ( 'NONE',  ( -23.77929240705206126, 25.06639637888459404, 26.20227034809527211 ) ) ;
#26234 = VECTOR ( 'NONE', #4768, 1000.000000000000227 ) ;
#26235 = CARTESIAN_POINT ( 'NONE',  ( -55.25719721206881729, 0.006045473558784881206, 0.009391134844728978373 ) ) ;
#26236 = CARTESIAN_POINT ( 'NONE',  ( -20.24399999263414429, -23.20123049637379253, -18.44171895251388094 ) ) ;
#26237 = CONICAL_SURFACE ( 'NONE', #1878, 34.60786435723138510, 0.8559913436420825139 ) ;
#26238 = EDGE_CURVE ( 'NONE', #12584, #25403, #14342, .T. ) ;
#26239 = ORIENTED_EDGE ( 'NONE', *, *, #1749, .F. ) ;
#26240 = EDGE_LOOP ( 'NONE', ( #27066, #3554, #16795, #16811 ) ) ;
#26241 = ADVANCED_FACE ( 'NONE', ( #4655 ), #9288, .F. ) ;
#26243 = CARTESIAN_POINT ( 'NONE',  ( -22.23342874802668234, 7.677086057585391643, 30.68433055777672180 ) ) ;
#26242 = DIRECTION ( 'NONE',  ( 1.000000000000000000, -6.938893903907226837E-18, 1.734723475976806709E-18 ) ) ;
#26244 = CARTESIAN_POINT ( 'NONE',  ( -55.24271866751342941, -0.009369360294295350430, -0.001545935011630812216 ) ) ;
#26245 = CARTESIAN_POINT ( 'NONE',  ( -55.24728320129491266, -0.01137345571546789259, 0.009072670231975133240 ) ) ;
#26246 = CARTESIAN_POINT ( 'NONE',  ( -20.47566262905010248, -29.82700878811085232, -1.586617686065453725 ) ) ;
#26247 = CARTESIAN_POINT ( 'NONE',  ( 1.832998868059858122, -72.09222286251171852, 125.9352106559981621 ) ) ;
#26248 = VERTEX_POINT ( 'NONE', #196 ) ;
#26249 = CARTESIAN_POINT ( 'NONE',  ( -55.24728320129491266, 0.009072670231975488858, 0.01137345571546827770 ) ) ;
#26250 =( BOUNDED_SURFACE ( )  B_SPLINE_SURFACE ( 3, 1, ( 
 ( #5958, #21616 ),
 ( #1620, #1894 ),
 ( #14710, #10696 ),
 ( #28229, #23524 ) ),
 .UNSPECIFIED., .F., .F., .F. ) 
 B_SPLINE_SURFACE_WITH_KNOTS ( ( 4, 4 ),
 ( 2, 2 ),
 ( 0.000000000000000000, 1.000000000000000000 ),
 ( 0.000000000000000000, 1.000000000000000000 ),
 .UNSPECIFIED. ) 
 GEOMETRIC_REPRESENTATION_ITEM ( )  RATIONAL_B_SPLINE_SURFACE ( (
 ( 1.000000000000000000, 1.000000000000000000),
 ( 0.9956975270656954757, 0.8568959468854893125),
 ( 0.9956975270656954757, 0.8568959468854893125),
 ( 1.000000000000000000, 1.000000000000000000) ) ) 
 REPRESENTATION_ITEM ( '' )  SURFACE ( )  );
#26251 = EDGE_CURVE ( 'NONE', #24022, #18945, #13422, .T. ) ;
#26252 = CARTESIAN_POINT ( 'NONE',  ( -6.574463467970649511, 25.96726214983191383, -44.27173031830743355 ) ) ;
#26253 = CARTESIAN_POINT ( 'NONE',  ( 55.79472521941428198, 72.75035398477136539, -0.7279028900796159496 ) ) ;
#26254 = ORIENTED_EDGE ( 'NONE', *, *, #13068, .F. ) ;
#26255 = ORIENTED_EDGE ( 'NONE', *, *, #8240, .T. ) ;
#26256 = CARTESIAN_POINT ( 'NONE',  ( -1.045287976400362417, -28.14015102489855735, -36.12803364096578207 ) ) ;
#26257 = EDGE_CURVE ( 'NONE', #26024, #7427, #10125, .T. ) ;
#26258 = ORIENTED_EDGE ( 'NONE', *, *, #26901, .T. ) ;
#26259 = DIRECTION ( 'NONE',  ( 0.7637818620346800147, 0.3965875333584841234, -0.5092696688508654423 ) ) ;
#26260 = ORIENTED_EDGE ( 'NONE', *, *, #23549, .F. ) ;
#26261 = CIRCLE ( 'NONE', #5120, 151.1787379149930359 ) ;
#26262 = VECTOR ( 'NONE', #5419, 1000.000000000000000 ) ;
#26263 = CARTESIAN_POINT ( 'NONE',  ( -1.031422197589711987, 43.06660437151308685, -15.60268798220652720 ) ) ;
#26264 = CONICAL_SURFACE ( 'NONE', #12013, 34.60786435723138510, 0.8559913436420825139 ) ;
#26265 = ORIENTED_EDGE ( 'NONE', *, *, #25084, .T. ) ;
#26266 = CARTESIAN_POINT ( 'NONE',  ( 9.884929003653626367, -124.2095058357571702, -85.04731144912641128 ) ) ;
#26267 = CARTESIAN_POINT ( 'NONE',  ( 10.93730112725972781, -92.80059208661754155, 119.3442956573269100 ) ) ;
#26268 = CARTESIAN_POINT ( 'NONE',  ( 109.1624594426973118, 0.01551217196237750923, -0.003771499231554137181 ) ) ;
#26269 = LINE ( 'NONE', #26547, #7418 ) ;
#26270 = CARTESIAN_POINT ( 'NONE',  ( 55.79472521941428198, 69.41463258328512609, 21.78881894124727836 ) ) ;
#26271 = CARTESIAN_POINT ( 'NONE',  ( 25.64681081121879203, 103.3177883989779531, 45.54494737132259274 ) ) ;
#26272 = CARTESIAN_POINT ( 'NONE',  ( 1.893872463202013856, -117.9862474593102633, 84.54426271294393302 ) ) ;
#26273 = DIRECTION ( 'NONE',  ( 0.000000000000000000, 5.223019709707975211E-21, -1.000000000000000000 ) ) ;
#26274 = EDGE_CURVE ( 'NONE', #25406, #16728, #24521, .T. ) ;
#26275 = ORIENTED_EDGE ( 'NONE', *, *, #261, .F. ) ;
#26277 = ORIENTED_EDGE ( 'NONE', *, *, #455, .T. ) ;
#26276 = B_SPLINE_CURVE_WITH_KNOTS ( 'NONE', 3,
 ( #1297, #9815, #14678, #23482, #10098, #27638 ),
 .UNSPECIFIED., .F., .F.,
 ( 4, 2, 4 ),
 ( 0.000000000000000000, 0.0006311636237756806456, 0.001262327247551361291 ),
 .UNSPECIFIED. ) ;
#26278 = CARTESIAN_POINT ( 'NONE',  ( 25.81918753295378011, 83.36706424720549080, -76.32043280377732231 ) ) ;
#26279 = B_SPLINE_CURVE_WITH_KNOTS ( 'NONE', 3,
 ( #8136, #16900, #25552, #1494, #10561, #25693 ),
 .UNSPECIFIED., .F., .F.,
 ( 4, 2, 4 ),
 ( 0.000000000000000000, 0.0004335184443140274431, 0.0008670368886280548863 ),
 .UNSPECIFIED. ) ;
#26280 = CARTESIAN_POINT ( 'NONE',  ( 2.063896406836609909, -86.47093297168922277, -116.7302989755746268 ) ) ;
#26281 = EDGE_CURVE ( 'NONE', #26365, #5798, #15258, .T. ) ;
#26282 = CARTESIAN_POINT ( 'NONE',  ( -1.048171036023500369, -27.73816396939538009, 36.44209502233739073 ) ) ;
#26283 = CARTESIAN_POINT ( 'NONE',  ( -25.21435515916043713, 16.39063784838786475, 30.48034229288620622 ) ) ;
#26284 = CARTESIAN_POINT ( 'NONE',  ( 1.833206308920068972, 84.68961866583003939, 117.8322276971139075 ) ) ;
#26285 = CARTESIAN_POINT ( 'NONE',  ( 28.37599760073042887, 111.8383885143455387, 25.60640155549204877 ) ) ;
#26286 = ORIENTED_EDGE ( 'NONE', *, *, #10196, .T. ) ;
#26287 = CARTESIAN_POINT ( 'NONE',  ( 25.64708010899963142, -34.94352788466213866, -107.3680906278375886 ) ) ;
#26288 = CIRCLE ( 'NONE', #16178, 53.53553390275978785 ) ;
#26289 = EDGE_CURVE ( 'NONE', #5379, #1423, #2055, .T. ) ;
#26290 = CARTESIAN_POINT ( 'NONE',  ( -1.583189561560255143, -38.94740041318274848, 25.21827308671275247 ) ) ;
#26291 = DIRECTION ( 'NONE',  ( -0.5946245182733607137, 0.7999021332774024495, 0.08110646981859331861 ) ) ;
#26292 = CARTESIAN_POINT ( 'NONE',  ( -5.986830583229479252, 33.39046620690970002, 38.20088153919464702 ) ) ;
#26293 = ORIENTED_EDGE ( 'NONE', *, *, #672, .F. ) ;
#26294 = CARTESIAN_POINT ( 'NONE',  ( 9.884929003653608603, -139.1775604444707710, 57.36421526887111355 ) ) ;
#26295 =( BOUNDED_SURFACE ( )  B_SPLINE_SURFACE ( 3, 1, ( 
 ( #25864, #13168 ),
 ( #23729, #23862 ),
 ( #21958, #3974 ),
 ( #8447, #83 ) ),
 .UNSPECIFIED., .F., .F., .F. ) 
 B_SPLINE_SURFACE_WITH_KNOTS ( ( 4, 4 ),
 ( 2, 2 ),
 ( 0.000000000000000000, 1.000000000000000000 ),
 ( 0.000000000000000000, 1.000000000000000000 ),
 .UNSPECIFIED. ) 
 GEOMETRIC_REPRESENTATION_ITEM ( )  RATIONAL_B_SPLINE_SURFACE ( (
 ( 1.000000000000000000, 1.000000000000000000),
 ( 0.9934239774497838349, 0.8357310067453913582),
 ( 0.9934239774497838349, 0.8357310067453913582),
 ( 1.000000000000000000, 1.000000000000000000) ) ) 
 REPRESENTATION_ITEM ( '' )  SURFACE ( )  );
#26296 = CARTESIAN_POINT ( 'NONE',  ( 2.430230287190572103, -96.28466919684024106, -109.1043569252024241 ) ) ;
#26297 = DIRECTION ( 'NONE',  ( 0.000000000000000000, 5.223019709708233256E-21, -1.000000000000000000 ) ) ;
#26298 = CARTESIAN_POINT ( 'NONE',  ( 26.04756280548352620, 65.62256188141849123, -92.21166514879033116 ) ) ;
#26299 = ORIENTED_EDGE ( 'NONE', *, *, #18252, .T. ) ;
#26300 = DIRECTION ( 'NONE',  ( 0.000000000000000000, 5.223019709708116647E-21, -1.000000000000000000 ) ) ;
#26302 =( BOUNDED_SURFACE ( )  B_SPLINE_SURFACE ( 3, 1, ( 
 ( #15519, #9205 ),
 ( #24331, #4593 ),
 ( #15663, #19852 ),
 ( #11081, #11222 ) ),
 .UNSPECIFIED., .F., .F., .F. ) 
 B_SPLINE_SURFACE_WITH_KNOTS ( ( 4, 4 ),
 ( 2, 2 ),
 ( 0.000000000000000000, 1.000000000000000000 ),
 ( 0.000000000000000000, 1.000000000000000000 ),
 .UNSPECIFIED. ) 
 GEOMETRIC_REPRESENTATION_ITEM ( )  RATIONAL_B_SPLINE_SURFACE ( (
 ( 1.000000000000000000, 1.000000000000000000),
 ( 0.7789835883360576307, 0.9689951854195403280),
 ( 0.7789835883360576307, 0.9689951854195403280),
 ( 1.000000000000000000, 1.000000000000000000) ) ) 
 REPRESENTATION_ITEM ( '' )  SURFACE ( )  );
#26301 = AXIS2_PLACEMENT_3D ( 'NONE', #21818, #12878, #3970 ) ;
#26303 = CARTESIAN_POINT ( 'NONE',  ( -55.24390624410018802, -0.004572280736701530256, -0.009374879212970928244 ) ) ;
#26304 = CIRCLE ( 'NONE', #7964, 28.92774122539760384 ) ;
#26305 = CARTESIAN_POINT ( 'NONE',  ( 30.59141879584313983, -9.457572341075664468, -115.8270959620730736 ) ) ;
#26306 = CARTESIAN_POINT ( 'NONE',  ( 8.186469829613956861, 148.1306754360699074, 19.05650981809850819 ) ) ;
#26307 = CARTESIAN_POINT ( 'NONE',  ( 32.73300124599737870, 20.69176323058787759, -115.8010721414081132 ) ) ;
#26308 = CARTESIAN_POINT ( 'NONE',  ( 32.73300124599732186, 0.000000000000000000, 0.000000000000000000 ) ) ;
#26309 = CARTESIAN_POINT ( 'NONE',  ( 32.73300124599741423, -97.37344512919810313, -66.00340565729437969 ) ) ;
#26310 = CARTESIAN_POINT ( 'NONE',  ( 28.37599760073042532, 68.88138253892522300, -91.75439000741624795 ) ) ;
#26311 = CARTESIAN_POINT ( 'NONE',  ( -28.13707043255157103, 14.07296284901359051, 18.06394523322437706 ) ) ;
#26312 = LINE ( 'NONE', #6889, #23334 ) ;
#26313 = EDGE_LOOP ( 'NONE', ( #24118, #9623, #1175, #15697 ) ) ;
#26314 = ORIENTED_EDGE ( 'NONE', *, *, #19090, .T. ) ;
#26315 = CARTESIAN_POINT ( 'NONE',  ( 25.64681081121879203, 103.3177883989779531, 45.54494737132259274 ) ) ;
#26316 = CARTESIAN_POINT ( 'NONE',  ( -20.20700224038492721, 0.9908225410478516126, -29.58392382092673145 ) ) ;
#26317 = ADVANCED_FACE ( 'NONE', ( #9117 ), #11415, .F. ) ;
#26318 = CARTESIAN_POINT ( 'NONE',  ( 1.831572820252009626, 144.4165162501763007, 14.18623102066816166 ) ) ;
#26319 = CARTESIAN_POINT ( 'NONE',  ( 109.1624594426973260, -0.0004639210235576873820, 0.01595733256931099880 ) ) ;
#26320 = CARTESIAN_POINT ( 'NONE',  ( 24.22246935314087324, 90.00000000000005684, 39.99999999999999289 ) ) ;
#26321 = CARTESIAN_POINT ( 'NONE',  ( 109.1589550718175161, -0.006257602293702388060, -0.004269295012381895196 ) ) ;
#26322 = ORIENTED_EDGE ( 'NONE', *, *, #8267, .T. ) ;
#26323 = CARTESIAN_POINT ( 'NONE',  ( -1.031422197589716205, -43.06660437151320053, -15.60268798220621633 ) ) ;
#26324 = CARTESIAN_POINT ( 'NONE',  ( -1.583189561560253589, -46.33203782964459805, 2.490696082060356531 ) ) ;
#26325 = CARTESIAN_POINT ( 'NONE',  ( 25.64681081121880624, 23.88203588908233499, -110.3564950173079353 ) ) ;
#26326 = CARTESIAN_POINT ( 'NONE',  ( 109.1592201516379674, 0.0003082430542015802727, 0.007856029051022768092 ) ) ;
#26327 = ADVANCED_FACE ( 'NONE', ( #15726 ), #24057, .T. ) ;
#26328 = EDGE_CURVE ( 'NONE', #11017, #5935, #4592, .T. ) ;
#26329 = CARTESIAN_POINT ( 'NONE',  ( 109.1778270068192853, -0.009220257877180833977, 0.001322180554001369359 ) ) ;
#26330 = AXIS2_PLACEMENT_3D ( 'NONE', #20462, #11539, #608 ) ;
#26331 = CONICAL_SURFACE ( 'NONE', #8003, 34.60786435723138510, 0.8559913436420825139 ) ;
#26332 = CARTESIAN_POINT ( 'NONE',  ( -20.20700224038492721, 29.58392382092673500, -0.9908225410479557516 ) ) ;
#26333 = CARTESIAN_POINT ( 'NONE',  ( 25.64681081121879203, 110.3564950173081769, 23.88203588908119457 ) ) ;
#26334 = ORIENTED_EDGE ( 'NONE', *, *, #2462, .T. ) ;
#26335 = ORIENTED_EDGE ( 'NONE', *, *, #26901, .F. ) ;
#26336 = VERTEX_POINT ( 'NONE', #7258 ) ;
#26337 = CARTESIAN_POINT ( 'NONE',  ( -20.47566262905009538, -18.81547655725230328, 23.19796652405694459 ) ) ;
#26338 = FACE_OUTER_BOUND ( 'NONE', #26541, .T. ) ;
#26339 = AXIS2_PLACEMENT_3D ( 'NONE', #15150, #25611, #23973 ) ;
#26340 = CARTESIAN_POINT ( 'NONE',  ( -1.583189561560255143, -36.01941156322808979, -29.24830400313152623 ) ) ;
#26341 =( BOUNDED_SURFACE ( )  B_SPLINE_SURFACE ( 3, 1, ( 
 ( #28021, #21275 ),
 ( #10358, #8321 ),
 ( #21546, #14789 ),
 ( #17087, #25612 ) ),
 .UNSPECIFIED., .F., .F., .F. ) 
 B_SPLINE_SURFACE_WITH_KNOTS ( ( 4, 4 ),
 ( 2, 2 ),
 ( 0.000000000000000000, 1.000000000000000000 ),
 ( 0.000000000000000000, 1.000000000000000000 ),
 .UNSPECIFIED. ) 
 GEOMETRIC_REPRESENTATION_ITEM ( )  RATIONAL_B_SPLINE_SURFACE ( (
 ( 1.000000000000000000, 1.000000000000000000),
 ( 0.9593753223639863714, 0.9995975284513187731),
 ( 0.9593753223639863714, 0.9995975284513187731),
 ( 1.000000000000000000, 1.000000000000000000) ) ) 
 REPRESENTATION_ITEM ( '' )  SURFACE ( )  );
#26342 = ORIENTED_EDGE ( 'NONE', *, *, #5092, .F. ) ;
#26343 = CARTESIAN_POINT ( 'NONE',  ( -28.41354790283022069, 8.345538364877077342, -21.64275480268750940 ) ) ;
#26344 = VECTOR ( 'NONE', #791, 1000.000000000000000 ) ;
#26345 = AXIS2_PLACEMENT_3D ( 'NONE', #27495, #1169, #27202 ) ;
#26346 = CARTESIAN_POINT ( 'NONE',  ( -1.050230347699840694, -0.0002315326057593219944, 45.79907861674081460 ) ) ;
#26347 = ORIENTED_EDGE ( 'NONE', *, *, #22704, .T. ) ;
#26348 = ORIENTED_EDGE ( 'NONE', *, *, #12357, .F. ) ;
#26349 = CARTESIAN_POINT ( 'NONE',  ( 1.833838848569445679, 141.9017642089168589, -30.34409872482092752 ) ) ;
#26350 = CARTESIAN_POINT ( 'NONE',  ( 1.833838848569444790, -45.01064392477834986, -137.9525894882061721 ) ) ;
#26351 = EDGE_CURVE ( 'NONE', #23299, #13256, #22512, .T. ) ;
#26352 = CARTESIAN_POINT ( 'NONE',  ( -55.24271866751342941, 0.009369360294296127586, 0.001545935011630553526 ) ) ;
#26353 = CARTESIAN_POINT ( 'NONE',  ( -2.911734481061415636, 25.69892591260268588, -40.13920818157085080 ) ) ;
#26354 = CARTESIAN_POINT ( 'NONE',  ( -7.078251931573406708, 5.101176922831390570, 51.82710018979469879 ) ) ;
#26355 = CARTESIAN_POINT ( 'NONE',  ( -20.47566262905009538, -25.06314747784824348, 16.24827521404678521 ) ) ;
#26356 = CARTESIAN_POINT ( 'NONE',  ( 1.832998868059890096, -73.01698022778442976, 125.4013017422228558 ) ) ;
#26357 = CARTESIAN_POINT ( 'NONE',  ( 119.2224693531408803, -90.00000000000005684, 39.99999999999997158 ) ) ;
#26358 = CARTESIAN_POINT ( 'NONE',  ( -55.24198130335446422, 0.006617369590169233477, 0.006527480770975859110 ) ) ;
#26359 = CARTESIAN_POINT ( 'NONE',  ( 32.73300124599735028, -8.473903470906931190, 117.3295799645429156 ) ) ;
#26360 = EDGE_LOOP ( 'NONE', ( #23560, #20025, #6429, #7754 ) ) ;
#26361 = ORIENTED_EDGE ( 'NONE', *, *, #21511, .T. ) ;
#26362 = CARTESIAN_POINT ( 'NONE',  ( 1.833485406944043827, -125.9346397303440455, 72.09189602597663793 ) ) ;
#26363 = CARTESIAN_POINT ( 'NONE',  ( 24.01988960052069899, -36.40943914739808918, -125.8850824254502641 ) ) ;
#26364 = ORIENTED_EDGE ( 'NONE', *, *, #26031, .T. ) ;
#26365 = VERTEX_POINT ( 'NONE', #2778 ) ;
#26366 = ORIENTED_EDGE ( 'NONE', *, *, #5810, .F. ) ;
#26367 = CARTESIAN_POINT ( 'NONE',  ( -20.20700224038492010, -0.9908225410480588913, -29.58392382092672435 ) ) ;
#26368 = B_SPLINE_CURVE_WITH_KNOTS ( 'NONE', 3,
 ( #2036, #21347, #17019, #10426, #23946, #15125 ),
 .UNSPECIFIED., .F., .F.,
 ( 4, 2, 4 ),
 ( 3.525929482785130599E-16, 0.003576372551511158761, 0.007152745103021965374 ),
 .UNSPECIFIED. ) ;
#26369 = CARTESIAN_POINT ( 'NONE',  ( 109.1586900883932856, 0.006130969560687363727, -0.003656351050331872743 ) ) ;
#26370 = CARTESIAN_POINT ( 'NONE',  ( 25.70243777736191149, 11.07690056740865714, 112.4037002646848009 ) ) ;
#26371 = CARTESIAN_POINT ( 'NONE',  ( -1.539763995773681726, -25.17088606276573515, -38.84665165401054310 ) ) ;
#26372 = ADVANCED_FACE ( 'NONE', ( #27234 ), #20419, .F. ) ;
#26373 = CARTESIAN_POINT ( 'NONE',  ( -55.24340739397742084, -0.002421372372453905585, -0.009842732675352267036 ) ) ;
#26374 = EDGE_CURVE ( 'NONE', #12467, #9726, #25892, .T. ) ;
#26375 = CARTESIAN_POINT ( 'NONE',  ( 25.64704443564076541, 66.25951665433285598, 91.42548471394218268 ) ) ;
#26376 = CARTESIAN_POINT ( 'NONE',  ( -24.53239521893627995, 33.25736993155740606, -6.738460611583019677 ) ) ;
#26377 = CARTESIAN_POINT ( 'NONE',  ( 25.64700659047693421, -110.4909389345861115, 23.25292178500328077 ) ) ;
#26378 = EDGE_CURVE ( 'NONE', #11237, #7653, #19036, .T. ) ;
#26379 =( BOUNDED_SURFACE ( )  B_SPLINE_SURFACE ( 3, 1, ( 
 ( #9434, #5098 ),
 ( #26967, #16033 ),
 ( #13878, #2954 ),
 ( #11727, #9007 ) ),
 .UNSPECIFIED., .F., .F., .F. ) 
 B_SPLINE_SURFACE_WITH_KNOTS ( ( 4, 4 ),
 ( 2, 2 ),
 ( 0.000000000000000000, 1.000000000000000000 ),
 ( 0.000000000000000000, 1.000000000000000000 ),
 .UNSPECIFIED. ) 
 GEOMETRIC_REPRESENTATION_ITEM ( )  RATIONAL_B_SPLINE_SURFACE ( (
 ( 1.000000000000000000, 1.000000000000000000),
 ( 0.9960225298536222738, 0.9999952330161893110),
 ( 0.9960225298536222738, 0.9999952330161893110),
 ( 1.000000000000000000, 1.000000000000000000) ) ) 
 REPRESENTATION_ITEM ( '' )  SURFACE ( )  );
#26380 = CARTESIAN_POINT ( 'NONE',  ( -1.323439229708141429, 12.01475235539445485, -44.47813215539048315 ) ) ;
#26381 = CARTESIAN_POINT ( 'NONE',  ( 25.98552792386800903, 113.1317367103340246, -1.078856412011222288 ) ) ;
#26382 = CARTESIAN_POINT ( 'NONE',  ( 26.11404676487259024, 103.8885755249575453, -45.01677474591305383 ) ) ;
#26383 = VERTEX_POINT ( 'NONE', #23172 ) ;
#26384 = VERTEX_POINT ( 'NONE', #12206 ) ;
#26386 = CARTESIAN_POINT ( 'NONE',  ( 13.36082413113063083, -152.6206443696327995, -9.660980093456263518 ) ) ;
#26385 = CARTESIAN_POINT ( 'NONE',  ( 1.832998868059858122, 108.1944082009170245, -96.70023740551016544 ) ) ;
#26387 = CARTESIAN_POINT ( 'NONE',  ( 26.11404676487257603, -22.43340081644687345, -110.9778746459749499 ) ) ;
#26388 = CARTESIAN_POINT ( 'NONE',  ( -1.044557008772707407, 37.98985164565329598, -25.56990300676994821 ) ) ;
#26389 = B_SPLINE_CURVE_WITH_KNOTS ( 'NONE', 3,
 ( #22954, #904, #14274, #11710, #26948, #16013 ),
 .UNSPECIFIED., .F., .F.,
 ( 4, 2, 4 ),
 ( 1.552747097607904257E-16, 0.003570751334075639161, 0.007141502668151123064 ),
 .UNSPECIFIED. ) ;
#26390 = CARTESIAN_POINT ( 'NONE',  ( -1.031422197589716205, -45.78027046666443312, 1.530725436377931237 ) ) ;
#26391 = CARTESIAN_POINT ( 'NONE',  ( 25.65782528836479059, 0.5778133093793608177, -112.9169519833626794 ) ) ;
#26392 = CARTESIAN_POINT ( 'NONE',  ( 21.16825799904904315, -87.29264348877902080, 103.5479404090032745 ) ) ;
#26393 = B_SPLINE_CURVE_WITH_KNOTS ( 'NONE', 3,
 ( #13200, #6463, #2401, #13074, #17668, #24035, #4149 ),
 .UNSPECIFIED., .F., .F.,
 ( 4, 3, 4 ),
 ( 0.000000000000000000, 0.006568092053401791003, 0.02506242213020846987 ),
 .UNSPECIFIED. ) ;
#26394 = ORIENTED_EDGE ( 'NONE', *, *, #1493, .T. ) ;
#26395 = CARTESIAN_POINT ( 'NONE',  ( 25.64708228042122329, 97.80372460135754409, -56.42152786924399521 ) ) ;
#26396 = VERTEX_POINT ( 'NONE', #11633 ) ;
#26397 = CARTESIAN_POINT ( 'NONE',  ( -55.24390624410018802, 0.007503127514282199352, -0.007245494385991655198 ) ) ;
#26398 = CARTESIAN_POINT ( 'NONE',  ( -1.048172774974297949, -37.64158596421231096, -26.08722459372772562 ) ) ;
#26399 = ORIENTED_EDGE ( 'NONE', *, *, #13703, .T. ) ;
#26400 = EDGE_LOOP ( 'NONE', ( #17529, #24585, #24922, #25328 ) ) ;
#26401 = CARTESIAN_POINT ( 'NONE',  ( 2.433796855181233454, -126.7346379669250780, -71.49415740225209959 ) ) ;
#26402 = ORIENTED_EDGE ( 'NONE', *, *, #4999, .T. ) ;
#26403 = CARTESIAN_POINT ( 'NONE',  ( 109.1721716018069515, 0.01550977894511844715, 0.007126480965768039466 ) ) ;
#26404 = ORIENTED_EDGE ( 'NONE', *, *, #13341, .T. ) ;
#26405 = B_SPLINE_CURVE_WITH_KNOTS ( 'NONE', 3,
 ( #24941, #7674, #11831, #884, #9670, #8637, #14966 ),
 .UNSPECIFIED., .F., .F.,
 ( 4, 3, 4 ),
 ( 5.724587470723463412E-16, 0.02816610861753240935, 0.04000277880656283314 ),
 .UNSPECIFIED. ) ;
#26406 = LINE ( 'NONE', #13022, #21604 ) ;
#26407 = EDGE_CURVE ( 'NONE', #771, #15935, #7709, .T. ) ;
#26408 = VERTEX_POINT ( 'NONE', #20550 ) ;
#26409 = ADVANCED_FACE ( 'NONE', ( #27591 ), #11582, .F. ) ;
#26410 = DIRECTION ( 'NONE',  ( -0.7637818620346801257, -0.3965875333584914508, -0.5092696688508597802 ) ) ;
#26411 = EDGE_CURVE ( 'NONE', #20545, #24427, #22823, .T. ) ;
#26412 = CARTESIAN_POINT ( 'NONE',  ( 25.69398547355840634, -110.6264597420658049, -22.75551036952039041 ) ) ;
#26413 = CARTESIAN_POINT ( 'NONE',  ( 2.263178607246658647, 144.4462811785179213, -16.59120332982995549 ) ) ;
#26414 = CARTESIAN_POINT ( 'NONE',  ( -28.41354790283022069, 23.16239616762931064, 1.249099604787156981 ) ) ;
#26415 = DIRECTION ( 'NONE',  ( 1.000000000000000000, -0.000000000000000000, -0.000000000000000000 ) ) ;
#26416 = CARTESIAN_POINT ( 'NONE',  ( -20.37983603106074426, -29.73529213200290400, -1.508851015062473211 ) ) ;
#26417 = FACE_OUTER_BOUND ( 'NONE', #9854, .T. ) ;
#26418 =( BOUNDED_SURFACE ( )  B_SPLINE_SURFACE ( 3, 1, ( 
 ( #16087, #20409 ),
 ( #693, #26733 ),
 ( #13929, #11920 ),
 ( #12339, #18682 ) ),
 .UNSPECIFIED., .F., .F., .F. ) 
 B_SPLINE_SURFACE_WITH_KNOTS ( ( 4, 4 ),
 ( 2, 2 ),
 ( 0.000000000000000000, 1.000000000000000000 ),
 ( 0.000000000000000000, 1.000000000000000000 ),
 .UNSPECIFIED. ) 
 GEOMETRIC_REPRESENTATION_ITEM ( )  RATIONAL_B_SPLINE_SURFACE ( (
 ( 1.000000000000000000, 1.000000000000000000),
 ( 0.9593753223639863714, 0.9995975284513187731),
 ( 0.9593753223639863714, 0.9995975284513187731),
 ( 1.000000000000000000, 1.000000000000000000) ) ) 
 REPRESENTATION_ITEM ( '' )  SURFACE ( )  );
#26419 = EDGE_LOOP ( 'NONE', ( #19709, #6046, #28371, #19465 ) ) ;
#26420 = DIRECTION ( 'NONE',  ( 0.000000000000000000, 0.000000000000000000, 1.000000000000000000 ) ) ;
#26421 = CARTESIAN_POINT ( 'NONE',  ( -1.045287976400386842, -28.14015102489780062, 36.12803364096639314 ) ) ;
#26422 = CARTESIAN_POINT ( 'NONE',  ( -21.41430102051751305, -19.54553566814603016, -23.81424706376357392 ) ) ;
#26423 = CARTESIAN_POINT ( 'NONE',  ( 24.01988960052057465, 121.3896480498357704, -49.36855864442009079 ) ) ;
#26424 = CARTESIAN_POINT ( 'NONE',  ( -20.57838717382308147, 25.16001208503129760, 16.28767523336092893 ) ) ;
#26425 = ORIENTED_EDGE ( 'NONE', *, *, #19618, .F. ) ;
#26426 = CARTESIAN_POINT ( 'NONE',  ( 1.893872463202055156, -107.2274879309820932, -97.83022426232074054 ) ) ;
#26427 = CARTESIAN_POINT ( 'NONE',  ( 32.73300124599731475, 117.5726003567930036, -3.836798148479248827 ) ) ;
#26428 = CARTESIAN_POINT ( 'NONE',  ( 25.65782528836480836, -91.69136324939144345, 65.90345832277442639 ) ) ;
#26429 = FACE_OUTER_BOUND ( 'NONE', #20274, .T. ) ;
#26430 = ORIENTED_EDGE ( 'NONE', *, *, #25789, .F. ) ;
#26431 = CARTESIAN_POINT ( 'NONE',  ( -1.583189561560252701, 25.21827308671288392, 38.94740041318267032 ) ) ;
#26432 = CARTESIAN_POINT ( 'NONE',  ( -25.21435515916043713, -34.29329011225952684, 4.655591116594705703 ) ) ;
#26433 = ORIENTED_EDGE ( 'NONE', *, *, #3462, .T. ) ;
#26434 = CARTESIAN_POINT ( 'NONE',  ( 26.11404676487257603, 97.48350837663606683, 57.58742681967482469 ) ) ;
#26435 = ADVANCED_FACE ( 'NONE', ( #22738 ), #12512, .F. ) ;
#26436 = CARTESIAN_POINT ( 'NONE',  ( 2.433796855181233454, 109.1007109081226076, 96.28145139437721411 ) ) ;
#26437 = EDGE_CURVE ( 'NONE', #414, #2795, #14068, .T. ) ;
#26438 = ORIENTED_EDGE ( 'NONE', *, *, #8244, .T. ) ;
#26439 = EDGE_CURVE ( 'NONE', #25441, #18255, #9753, .T. ) ;
#26440 = CARTESIAN_POINT ( 'NONE',  ( 26.11404676487257603, 47.08215554553657256, -102.9690087468796662 ) ) ;
#26441 = CARTESIAN_POINT ( 'NONE',  ( -20.38016308990357928, 28.74660391518355951, 7.753479680700641197 ) ) ;
#26442 = CARTESIAN_POINT ( 'NONE',  ( 28.43349137099832191, 21.85613782299149221, -122.3147591366314373 ) ) ;
#26443 = CARTESIAN_POINT ( 'NONE',  ( -1.619063947482197729, 43.26576862488456499, 16.67502769180516964 ) ) ;
#26444 = ORIENTED_EDGE ( 'NONE', *, *, #9123, .F. ) ;
#26445 = FACE_OUTER_BOUND ( 'NONE', #6961, .T. ) ;
#26446 = EDGE_CURVE ( 'NONE', #9428, #24314, #21741, .T. ) ;
#26447 = CARTESIAN_POINT ( 'NONE',  ( -55.24390624410018802, 0.009374879212967415429, 0.004572280736702902422 ) ) ;
#26448 = CARTESIAN_POINT ( 'NONE',  ( 26.11404676487259024, -47.08215554553450488, -102.9690087468806325 ) ) ;
#26449 = CARTESIAN_POINT ( 'NONE',  ( -55.24271866751342941, 0.006671293903669565407, -0.006757859501006440936 ) ) ;
#26450 = ORIENTED_EDGE ( 'NONE', *, *, #16694, .F. ) ;
#26451 = ORIENTED_EDGE ( 'NONE', *, *, #778, .F. ) ;
#26452 = ORIENTED_EDGE ( 'NONE', *, *, #491, .T. ) ;
#26453 = VERTEX_POINT ( 'NONE', #5587 ) ;
#26454 = CARTESIAN_POINT ( 'NONE',  ( -16.86833981943413363, 43.82216161736224791, -5.948101187261743306 ) ) ;
#26455 = CARTESIAN_POINT ( 'NONE',  ( -55.25297051322618813, -0.01019003092403448357, -0.01093108995494832154 ) ) ;
#26456 = CARTESIAN_POINT ( 'NONE',  ( 25.64681081121879203, 75.24277141833491100, 84.18689316040072868 ) ) ;
#26457 = CARTESIAN_POINT ( 'NONE',  ( 109.1586900883932856, -0.001582822706032874097, -0.006960773163852184385 ) ) ;
#26458 = CARTESIAN_POINT ( 'NONE',  ( 1.833809397773803251, 72.70895493223548556, -125.5796696653631273 ) ) ;
#26459 = CARTESIAN_POINT ( 'NONE',  ( 19.66333377628745893, -114.0223162644903567, 77.29039328249557173 ) ) ;
#26460 = ORIENTED_EDGE ( 'NONE', *, *, #5525, .F. ) ;
#26461 = CARTESIAN_POINT ( 'NONE',  ( -8.259864102781671491, 52.60025989855203221, -6.590267880897108022 ) ) ;
#26462 = CARTESIAN_POINT ( 'NONE',  ( -9.156249394959706578, -53.74753343182696597, 9.022661520478342467 ) ) ;
#26463 = CARTESIAN_POINT ( 'NONE',  ( 25.64707127832796019, 1.378041109049876443E-14, 112.9112343549835487 ) ) ;
#26464 = CARTESIAN_POINT ( 'NONE',  ( -55.24271866751342941, 0.009388511352200529583, -0.001425019990779194824 ) ) ;
#26465 =( BOUNDED_SURFACE ( )  B_SPLINE_SURFACE ( 3, 1, ( 
 ( #4569, #7315 ),
 ( #11624, #7462 ),
 ( #20541, #22578 ),
 ( #13342, #4861 ) ),
 .UNSPECIFIED., .F., .F., .F. ) 
 B_SPLINE_SURFACE_WITH_KNOTS ( ( 4, 4 ),
 ( 2, 2 ),
 ( 0.000000000000000000, 1.000000000000000000 ),
 ( 0.000000000000000000, 1.000000000000000000 ),
 .UNSPECIFIED. ) 
 GEOMETRIC_REPRESENTATION_ITEM ( )  RATIONAL_B_SPLINE_SURFACE ( (
 ( 1.000000000000000000, 1.000000000000000000),
 ( 0.6386103224230302855, 0.9954351624131538845),
 ( 0.6386103224230302855, 0.9954351624131538845),
 ( 1.000000000000000000, 1.000000000000000000) ) ) 
 REPRESENTATION_ITEM ( '' )  SURFACE ( )  );
#26466 = CARTESIAN_POINT ( 'NONE',  ( 25.64681081121880624, -75.24277141833435678, -84.18689316040122606 ) ) ;
#26468 = CARTESIAN_POINT ( 'NONE',  ( 28.37599760073042887, 48.29934869928308672, -104.0705811520809192 ) ) ;
#26467 = B_SPLINE_CURVE_WITH_KNOTS ( 'NONE', 3,
 ( #15035, #23855, #12873, #10747, #28275, #17338 ),
 .UNSPECIFIED., .F., .F.,
 ( 4, 2, 4 ),
 ( 4.296969928001729735E-16, 0.003576372551511233788, 0.007152745103022037365 ),
 .UNSPECIFIED. ) ;
#26469 = CARTESIAN_POINT ( 'NONE',  ( -21.81686047589415622, 38.17230180719270294, 5.181745222995608025 ) ) ;
#26470 = FACE_OUTER_BOUND ( 'NONE', #661, .T. ) ;
#26471 = ORIENTED_EDGE ( 'NONE', *, *, #18461, .F. ) ;
#26472 =( BOUNDED_SURFACE ( )  B_SPLINE_SURFACE ( 3, 1, ( 
 ( #14518, #25488 ),
 ( #10626, #7932 ),
 ( #5762, #23324 ),
 ( #5898, #17097 ) ),
 .UNSPECIFIED., .F., .F., .F. ) 
 B_SPLINE_SURFACE_WITH_KNOTS ( ( 4, 4 ),
 ( 2, 2 ),
 ( 0.000000000000000000, 1.000000000000000000 ),
 ( 0.000000000000000000, 1.000000000000000000 ),
 .UNSPECIFIED. ) 
 GEOMETRIC_REPRESENTATION_ITEM ( )  RATIONAL_B_SPLINE_SURFACE ( (
 ( 1.000000000000000000, 1.000000000000000000),
 ( 0.6386103224230316178, 0.9954351624131538845),
 ( 0.6386103224230316178, 0.9954351624131538845),
 ( 1.000000000000000000, 1.000000000000000000) ) ) 
 REPRESENTATION_ITEM ( '' )  SURFACE ( )  );
#26473 = ORIENTED_EDGE ( 'NONE', *, *, #14324, .T. ) ;
#26474 = ORIENTED_EDGE ( 'NONE', *, *, #17781, .T. ) ;
#26475 = EDGE_CURVE ( 'NONE', #18704, #28095, #21754, .T. ) ;
#26476 = CARTESIAN_POINT ( 'NONE',  ( -55.24271866751342941, 0.009369360294294836952, -0.001545935011626992572 ) ) ;
#26477 = CARTESIAN_POINT ( 'NONE',  ( 109.1586059443104944, 0.005983234375914148369, -0.003774052605966652253 ) ) ;
#26478 = EDGE_CURVE ( 'NONE', #1807, #23985, #28144, .T. ) ;
#26479 = ORIENTED_EDGE ( 'NONE', *, *, #17339, .F. ) ;
#26480 = CARTESIAN_POINT ( 'NONE',  ( -15.02187109954798316, -40.82269973458204504, 21.95370994985608704 ) ) ;
#26481 = CARTESIAN_POINT ( 'NONE',  ( -1.259920593601969729, -12.06711544331594865, -44.39818421957811978 ) ) ;
#26482 = ORIENTED_EDGE ( 'NONE', *, *, #20403, .T. ) ;
#26483 = CARTESIAN_POINT ( 'NONE',  ( -20.20612091757421069, 10.22177757278315191, -27.77903622052259536 ) ) ;
#26484 = ORIENTED_EDGE ( 'NONE', *, *, #21224, .F. ) ;
#26485 = CARTESIAN_POINT ( 'NONE',  ( 1.893872463202055156, 31.10971550360780213, -141.7768406633801135 ) ) ;
#26486 = CARTESIAN_POINT ( 'NONE',  ( 1.833721034905619218, -45.17977675814218230, -137.8972080590636722 ) ) ;
#26487 = FACE_OUTER_BOUND ( 'NONE', #13434, .T. ) ;
#26488 = CARTESIAN_POINT ( 'NONE',  ( -1.619063947482197729, 16.67502769180622835, 43.26576862488415287 ) ) ;
#26489 = CARTESIAN_POINT ( 'NONE',  ( 109.1592201516379674, 0.004194960840990064228, 0.006649399203953477652 ) ) ;
#26490 = CARTESIAN_POINT ( 'NONE',  ( -9.156249394959706578, -53.90509764945135629, -8.027840202793747437 ) ) ;
#26491 = CARTESIAN_POINT ( 'NONE',  ( 32.73300124599737160, -89.94078864464117373, 75.82012867748450446 ) ) ;
#26492 = CARTESIAN_POINT ( 'NONE',  ( -1.583189561560253589, -43.29471907393730135, 16.68617981233748537 ) ) ;
#26493 = CARTESIAN_POINT ( 'NONE',  ( 1.833809397773859873, 14.99109763364144854, 144.3333383260367384 ) ) ;
#26494 = CARTESIAN_POINT ( 'NONE',  ( -8.786685647604885574, 6.096987947571466530E-17, -1.524246986892866633E-17 ) ) ;
#26495 = CARTESIAN_POINT ( 'NONE',  ( -23.77929240705206482, -4.877832571065186862, -35.93174012244169546 ) ) ;
#26496 = CARTESIAN_POINT ( 'NONE',  ( 26.04756280548353686, -1.110889087301714317, -113.1727782765314174 ) ) ;
#26497 = ORIENTED_EDGE ( 'NONE', *, *, #28261, .T. ) ;
#26498 = ORIENTED_EDGE ( 'NONE', *, *, #9684, .F. ) ;
#26499 = CARTESIAN_POINT ( 'NONE',  ( -21.41430102051752016, 23.81424706376365918, -19.54553566814595200 ) ) ;
#26500 = CARTESIAN_POINT ( 'NONE',  ( -55.24390624410018802, -0.001811362924359030029, -0.01027195578987783083 ) ) ;
#26501 = ORIENTED_EDGE ( 'NONE', *, *, #3720, .T. ) ;
#26502 = ORIENTED_EDGE ( 'NONE', *, *, #12036, .T. ) ;
#26503 = VERTEX_POINT ( 'NONE', #18821 ) ;
#26504 =( BOUNDED_SURFACE ( )  B_SPLINE_SURFACE ( 3, 1, ( 
 ( #4267, #28432 ),
 ( #24282, #13316 ),
 ( #8885, #6585 ),
 ( #11314, #17646 ) ),
 .UNSPECIFIED., .F., .F., .F. ) 
 B_SPLINE_SURFACE_WITH_KNOTS ( ( 4, 4 ),
 ( 2, 2 ),
 ( 0.000000000000000000, 1.000000000000000000 ),
 ( 0.000000000000000000, 1.000000000000000000 ),
 .UNSPECIFIED. ) 
 GEOMETRIC_REPRESENTATION_ITEM ( )  RATIONAL_B_SPLINE_SURFACE ( (
 ( 1.000000000000000000, 1.000000000000000000),
 ( 0.9956975270656955868, 0.8568959468854907557),
 ( 0.9956975270656955868, 0.8568959468854907557),
 ( 1.000000000000000000, 1.000000000000000000) ) ) 
 REPRESENTATION_ITEM ( '' )  SURFACE ( )  );
#26505 = CARTESIAN_POINT ( 'NONE',  ( -20.47566338032517663, -1.586617869344095322, -29.82700953060487592 ) ) ;
#26506 = ADVANCED_FACE ( 'NONE', ( #1544 ), #27223, .T. ) ;
#26507 = DIRECTION ( 'NONE',  ( 1.000000000000000000, 0.000000000000000000, 0.000000000000000000 ) ) ;
#26508 = B_SPLINE_CURVE_WITH_KNOTS ( 'NONE', 3,
 ( #12819, #8386, #21757, #3916, #21606, #25529, #1881 ),
 .UNSPECIFIED., .F., .F.,
 ( 4, 3, 4 ),
 ( 6.214185311943901542E-16, 0.02816610861753243017, 0.04000277880656280538 ),
 .UNSPECIFIED. ) ;
#26509 = ADVANCED_FACE ( 'NONE', ( #5880 ), #2584, .F. ) ;
#26510 = CARTESIAN_POINT ( 'NONE',  ( -20.57838717382308147, -18.89542499756516847, -23.26537097894098594 ) ) ;
#26511 = ADVANCED_FACE ( 'NONE', ( #16821 ), #1824, .F. ) ;
#26512 = CARTESIAN_POINT ( 'NONE',  ( -1.619063947482197729, -25.20140673341401438, -38.92136151114898723 ) ) ;
#26513 = CARTESIAN_POINT ( 'NONE',  ( -1.048171036023507474, 43.23005599774320729, 15.11933492062782847 ) ) ;
#26514 = FACE_OUTER_BOUND ( 'NONE', #8159, .T. ) ;
#26515 = CARTESIAN_POINT ( 'NONE',  ( -1.155001620486242553, 42.97366440495935080, 16.13799328198379257 ) ) ;
#26516 = CARTESIAN_POINT ( 'NONE',  ( -1.619063947482197729, 43.26576862488456499, 16.67502769180516964 ) ) ;
#26517 = CARTESIAN_POINT ( 'NONE',  ( -1.058473599757823180, 12.47539220917862934, -44.07591602137159725 ) ) ;
#26518 = CARTESIAN_POINT ( 'NONE',  ( -55.25719721206881729, -0.009391134844732829459, -0.006045473558784549006 ) ) ;
#26519 = EDGE_LOOP ( 'NONE', ( #20890, #8961, #9911, #3281, #17064, #23866, #881, #2368, #27936, #26158, #14815, #10020, #25875, #14378, #24068, #9827, #26680, #13004, #18344, #865, #24105, #10391, #2037, #22632, #23829, #1344, #19022, #5558, #13329, #16196, #27249, #19890, #641, #950, #13012, #20836, #9561, #17700, #13769, #4566, #10164, #20712, #10912, #26404, #3337, #6687, #5278, #7075, #16874, #17929, #9887, #9906, #15222, #27303, #8640, #27855, #23251, #4654, #202, #5988, #18209, #20531, #23650, #4155 ) ) ;
#26520 = ORIENTED_EDGE ( 'NONE', *, *, #25407, .F. ) ;
#26521 = B_SPLINE_CURVE_WITH_KNOTS ( 'NONE', 3,
 ( #12777, #2542, #17932, #9467, #20240, #24599 ),
 .UNSPECIFIED., .F., .F.,
 ( 4, 2, 4 ),
 ( 4.055692965608002806E-16, 0.003576372551511211671, 0.007152745103022018283 ),
 .UNSPECIFIED. ) ;
#26523 = CARTESIAN_POINT ( 'NONE',  ( -1.031422197589716205, 37.93675465142474224, -25.67058493451456513 ) ) ;
#26522 = CARTESIAN_POINT ( 'NONE',  ( 25.64708228042118776, 91.32398912287028736, 66.39944550735300766 ) ) ;
#26524 = CARTESIAN_POINT ( 'NONE',  ( -1.031422197589716205, 1.530725436377464499, -45.78027046666444733 ) ) ;
#26525 = PLANE ( 'NONE',  #1532 ) ;
#26526 = CARTESIAN_POINT ( 'NONE',  ( -20.20700224038492721, 10.08426345511588984, -27.82980252387822517 ) ) ;
#26527 = CARTESIAN_POINT ( 'NONE',  ( 32.73300124599734318, 97.37344512919861472, 66.00340565729376863 ) ) ;
#26528 = EDGE_CURVE ( 'NONE', #9465, #26085, #14220, .T. ) ;
#26529 = VERTEX_POINT ( 'NONE', #8181 ) ;
#26530 = CARTESIAN_POINT ( 'NONE',  ( -2.904412668506672457, -2.864640348250298008, 47.56768199507434502 ) ) ;
#26531 = ORIENTED_EDGE ( 'NONE', *, *, #23940, .F. ) ;
#26532 = CARTESIAN_POINT ( 'NONE',  ( 2.433796855181233454, -84.34988187691011774, 118.5671979538053904 ) ) ;
#26533 = CARTESIAN_POINT ( 'NONE',  ( -20.20612092514791058, -23.26073121129628873, 18.30568145913871447 ) ) ;
#26534 = VERTEX_POINT ( 'NONE', #19522 ) ;
#26535 = ORIENTED_EDGE ( 'NONE', *, *, #8244, .F. ) ;
#26536 = B_SPLINE_CURVE_WITH_KNOTS ( 'NONE', 3,
 ( #6542, #8988, #23972, #4373, #15294, #10861, #24248, #28393 ),
 .UNSPECIFIED., .F., .F.,
 ( 4, 2, 2, 4 ),
 ( 2.237231151233565423E-16, 0.002761568181852865501, 0.005523136363705507222, 0.01104627272741080454 ),
 .UNSPECIFIED. ) ;
#26537 = CARTESIAN_POINT ( 'NONE',  ( -1.619063947482197729, -16.67502769180532596, 43.26576862488450104 ) ) ;
#26538 = EDGE_CURVE ( 'NONE', #24633, #12673, #23592, .T. ) ;
#26539 = ORIENTED_EDGE ( 'NONE', *, *, #8382, .T. ) ;
#26540 = CARTESIAN_POINT ( 'NONE',  ( 109.1587776205901861, 0.006388631651935892941, 0.003592288931003373258 ) ) ;
#26541 = EDGE_LOOP ( 'NONE', ( #3551, #12984, #9509, #22137 ) ) ;
#26542 = EDGE_CURVE ( 'NONE', #22192, #20045, #18503, .T. ) ;
#26543 = CARTESIAN_POINT ( 'NONE',  ( -8.786685647604890903, 38.68584556812300690, -37.00619870957947910 ) ) ;
#26544 =( BOUNDED_SURFACE ( )  B_SPLINE_SURFACE ( 3, 1, ( 
 ( #502, #15594 ),
 ( #4531, #5104 ),
 ( #4828, #26969 ),
 ( #2510, #18053 ) ),
 .UNSPECIFIED., .F., .F., .F. ) 
 B_SPLINE_SURFACE_WITH_KNOTS ( ( 4, 4 ),
 ( 2, 2 ),
 ( 0.000000000000000000, 1.000000000000000000 ),
 ( 0.000000000000000000, 1.000000000000000000 ),
 .UNSPECIFIED. ) 
 GEOMETRIC_REPRESENTATION_ITEM ( )  RATIONAL_B_SPLINE_SURFACE ( (
 ( 1.000000000000000000, 1.000000000000000000),
 ( 0.9934239774497837239, 0.8357310067453919133),
 ( 0.9934239774497837239, 0.8357310067453919133),
 ( 1.000000000000000000, 1.000000000000000000) ) ) 
 REPRESENTATION_ITEM ( '' )  SURFACE ( )  );
#26545 = DIRECTION ( 'NONE',  ( 1.000000000000000000, -6.938893903907226837E-18, 1.734723475976806709E-18 ) ) ;
#26546 = CARTESIAN_POINT ( 'NONE',  ( 1.832998868059890096, 137.8420662456176160, -45.34898734665905096 ) ) ;
#26547 = CARTESIAN_POINT ( 'NONE',  ( 55.79472521941426777, -37.00555938668304634, 62.63970324008249690 ) ) ;
#26548 = CARTESIAN_POINT ( 'NONE',  ( 1.834118845439484335, 107.7186227765454731, 97.22976650547458632 ) ) ;
#26549 = CARTESIAN_POINT ( 'NONE',  ( -1.045287976400351981, 12.68782741917293855, -44.00138577190654132 ) ) ;
#26550 = CARTESIAN_POINT ( 'NONE',  ( 25.73574536432414916, -0.8061344836377023482, 112.9674920590232574 ) ) ;
#26551 = CARTESIAN_POINT ( 'NONE',  ( 25.64692872815577829, -56.73392579406778680, 97.62272225320926111 ) ) ;
#26552 = B_SPLINE_CURVE_WITH_KNOTS ( 'NONE', 3,
 ( #13172, #11174, #19654, #17907, #24577, #11447, #28427, #4540, #8726, #2666, #26282, #11032, #26421 ),
 .UNSPECIFIED., .F., .F.,
 ( 4, 3, 3, 3, 4 ),
 ( 9.813077866773594792E-18, 0.0007657099931970698858, 0.001531419946797932816, 0.002296279302920152098, 0.003061450627205747257 ),
 .UNSPECIFIED. ) ;
#26553 = ORIENTED_EDGE ( 'NONE', *, *, #7675, .F. ) ;
#26554 = DIRECTION ( 'NONE',  ( 0.7637818620346800147, -0.6201872550346642088, 0.1788995134688892708 ) ) ;
#26555 = CARTESIAN_POINT ( 'NONE',  ( -20.20700224038492721, -29.58392382092674211, -0.9908225410477480288 ) ) ;
#26556 = CARTESIAN_POINT ( 'NONE',  ( 26.11404676487257603, -108.0249973236469572, 33.91085499298339556 ) ) ;
#26557 = B_SPLINE_CURVE_WITH_KNOTS ( 'NONE', 3,
 ( #5554, #19214, #16640, #27565, #5410, #7881, #3398 ),
 .UNSPECIFIED., .F., .F.,
 ( 4, 3, 4 ),
 ( 0.000000000000000000, 0.02398743853561371292, 0.04000277880656220864 ),
 .UNSPECIFIED. ) ;
#26558 = CARTESIAN_POINT ( 'NONE',  ( 1.833485406944057594, -125.4007332306550921, 73.01664920992921282 ) ) ;
#26559 = ORIENTED_EDGE ( 'NONE', *, *, #1434, .F. ) ;
#26560 = CARTESIAN_POINT ( 'NONE',  ( -8.786685647604894456, 7.199674155859698388, 53.04920435127174017 ) ) ;
#26561 = CARTESIAN_POINT ( 'NONE',  ( -12.94347594948475333, -48.30328466416771960, -6.555928820869143969 ) ) ;
#26562 = CARTESIAN_POINT ( 'NONE',  ( 25.64708228042119487, 112.2886173090159616, 11.84161204513297605 ) ) ;
#26563 = CARTESIAN_POINT ( 'NONE',  ( 1.833485406944043827, -45.34878176254329674, 137.8414413349084100 ) ) ;
#26564 = VERTEX_POINT ( 'NONE', #8313 ) ;
#26565 = CARTESIAN_POINT ( 'NONE',  ( -4.473127245936434626, -18.25038884639903003, -45.82513704981538183 ) ) ;
#26566 = EDGE_CURVE ( 'NONE', #22983, #1293, #12338, .T. ) ;
#26567 = EDGE_CURVE ( 'NONE', #25087, #18715, #1811, .T. ) ;
#26568 = CARTESIAN_POINT ( 'NONE',  ( 109.1624594426973260, 0.01551217196236919470, 0.003771499231549628635 ) ) ;
#26569 = CARTESIAN_POINT ( 'NONE',  ( -1.539760825549681966, -35.94320866319468166, 29.16712717142800670 ) ) ;
#26570 = ORIENTED_EDGE ( 'NONE', *, *, #5204, .T. ) ;
#26571 = LINE ( 'NONE', #6873, #17021 ) ;
#26572 = DIRECTION ( 'NONE',  ( -0.5914120900931443270, 0.1598001217819472741, -0.7903769105750327872 ) ) ;
#26573 = PLANE ( 'NONE',  #9675 ) ;
#26574 = ORIENTED_EDGE ( 'NONE', *, *, #7103, .T. ) ;
#26575 = DIRECTION ( 'NONE',  ( -1.000000000000000000, -0.000000000000000000, -0.000000000000000000 ) ) ;
#26576 = CARTESIAN_POINT ( 'NONE',  ( 55.79472521941426777, -6.880567342319213964, -72.42790650415581410 ) ) ;
#26577 = CARTESIAN_POINT ( 'NONE',  ( 25.64699802086723324, -34.66526531169716208, 107.4581924007664071 ) ) ;
#26578 = LINE ( 'NONE', #11054, #18150 ) ;
#26579 = DIRECTION ( 'NONE',  ( 1.000000000000000000, -6.938893903907226837E-18, 1.734723475976806709E-18 ) ) ;
#26580 = CARTESIAN_POINT ( 'NONE',  ( 1.832998868059890096, -58.53348008137737679, 132.7810136645736350 ) ) ;
#26581 = EDGE_LOOP ( 'NONE', ( #12837, #8999, #28189, #5085 ) ) ;
#26582 = CARTESIAN_POINT ( 'NONE',  ( 109.1624594426973260, -0.008380433676406151208, 0.01358749486988127669 ) ) ;
#26583 = FACE_OUTER_BOUND ( 'NONE', #5020, .T. ) ;
#26584 = CARTESIAN_POINT ( 'NONE',  ( -20.20700224038492721, 29.58392382092673500, -0.9908225410479557516 ) ) ;
#26585 = VECTOR ( 'NONE', #23345, 1000.000000000000000 ) ;
#26586 = CARTESIAN_POINT ( 'NONE',  ( 109.1778270068192853, 0.009031542838326012818, -0.002278716897417647214 ) ) ;
#26587 = ORIENTED_EDGE ( 'NONE', *, *, #21382, .T. ) ;
#26588 = B_SPLINE_CURVE_WITH_KNOTS ( 'NONE', 3,
 ( #15093, #28466, #8771, #23911 ),
 .UNSPECIFIED., .F., .F.,
 ( 4, 4 ),
 ( 1.173473438232358829E-16, 0.008383748772659590717 ),
 .UNSPECIFIED. ) ;
#26589 = VERTEX_POINT ( 'NONE', #3851 ) ;
#26590 = CARTESIAN_POINT ( 'NONE',  ( -28.41354790283022069, 18.00456980371900784, -14.62505768302807319 ) ) ;
#26591 = CARTESIAN_POINT ( 'NONE',  ( 2.430230287190581429, -133.5180086894995100, 57.85706160874099169 ) ) ;
#26592 = CARTESIAN_POINT ( 'NONE',  ( 26.11404676487259024, -33.91085499298451822, 108.0249973236466445 ) ) ;
#26593 = CARTESIAN_POINT ( 'NONE',  ( -1.050230347360791017, 0.0004630652117437840452, -45.79907861464602092 ) ) ;
#26594 = CARTESIAN_POINT ( 'NONE',  ( -16.86833981943413363, 43.82216161736224791, -5.948101187261743306 ) ) ;
#26595 = CARTESIAN_POINT ( 'NONE',  ( 26.11404676487257603, -103.8885755249572469, 45.01677474591374306 ) ) ;
#26596 = CARTESIAN_POINT ( 'NONE',  ( 25.81918753295379432, 46.82320532096518662, 102.8711004511195028 ) ) ;
#26597 = ORIENTED_EDGE ( 'NONE', *, *, #2247, .F. ) ;
#26598 = CARTESIAN_POINT ( 'NONE',  ( 1.833206308920069860, 132.2594750499825977, 59.70089323729781938 ) ) ;
#26599 = CARTESIAN_POINT ( 'NONE',  ( -55.25719721206881729, -0.008651607285659737578, -0.007063345920777289004 ) ) ;
#26600 = DIRECTION ( 'NONE',  ( 1.000000000000000000, -6.938893903907226837E-18, -5.541455922705464902E-20 ) ) ;
#26601 = EDGE_CURVE ( 'NONE', #14777, #6545, #13873, .T. ) ;
#26602 = FACE_OUTER_BOUND ( 'NONE', #23436, .T. ) ;
#26603 = EDGE_CURVE ( 'NONE', #26024, #24227, #17220, .T. ) ;
#26604 = FACE_OUTER_BOUND ( 'NONE', #24605, .T. ) ;
#26605 = CARTESIAN_POINT ( 'NONE',  ( 1.834118845439484335, 72.70910183320567910, 125.5799175751972143 ) ) ;
#26606 = VERTEX_POINT ( 'NONE', #12477 ) ;
#26608 = EDGE_CURVE ( 'NONE', #26730, #604, #20351, .T. ) ;
#26607 = CARTESIAN_POINT ( 'NONE',  ( -20.24419206586953379, 29.61012937815439372, -1.282847120831333898 ) ) ;
#26609 = CARTESIAN_POINT ( 'NONE',  ( 1.833485406944057594, -117.7091014914944225, -84.86072343962690923 ) ) ;
#26610 = ORIENTED_EDGE ( 'NONE', *, *, #12158, .T. ) ;
#26611 = EDGE_CURVE ( 'NONE', #4663, #8780, #16612, .T. ) ;
#26612 = ORIENTED_EDGE ( 'NONE', *, *, #2594, .T. ) ;
#26613 = ORIENTED_EDGE ( 'NONE', *, *, #24753, .F. ) ;
#26614 = B_SPLINE_CURVE_WITH_KNOTS ( 'NONE', 3,
 ( #21414, #8192, #12219, #10487, #7927, #18984, #6039 ),
 .UNSPECIFIED., .F., .F.,
 ( 4, 3, 4 ),
 ( 2.453269466693398621E-17, 0.009512539173626417474, 0.02506242213020847681 ),
 .UNSPECIFIED. ) ;
#26615 = CARTESIAN_POINT ( 'NONE',  ( 25.64700659047694487, -23.25292178500283669, -110.4909389345861825 ) ) ;
#26616 = CARTESIAN_POINT ( 'NONE',  ( -55.24271866751342941, 0.006671293903668397071, 0.006757859501010046559 ) ) ;
#26617 = ORIENTED_EDGE ( 'NONE', *, *, #18954, .F. ) ;
#26618 = DIRECTION ( 'NONE',  ( -0.5946245182733608248, -0.7332888028688948623, 0.3297108033645193004 ) ) ;
#26619 = CARTESIAN_POINT ( 'NONE',  ( -55.24390624410018802, -0.01027195578987978239, -0.001811362924362686826 ) ) ;
#26620 = EDGE_LOOP ( 'NONE', ( #16912, #21007, #14027, #1315 ) ) ;
#26621 = CARTESIAN_POINT ( 'NONE',  ( -20.37983603106074426, 10.62371319148641291, -27.81368274044714539 ) ) ;
#26622 = EDGE_LOOP ( 'NONE', ( #24700, #16333, #15475, #12185 ) ) ;
#26623 = CARTESIAN_POINT ( 'NONE',  ( -55.25297051322618813, 0.01019003092403740832, -0.01093108995495187946 ) ) ;
#26624 = CARTESIAN_POINT ( 'NONE',  ( 2.263178113027063176, 13.80342493153510652, 144.7392881653024403 ) ) ;
#26625 = CARTESIAN_POINT ( 'NONE',  ( 109.1587776205901577, 0.007280006032833117625, 0.0008489206734409118381 ) ) ;
#26626 = CARTESIAN_POINT ( 'NONE',  ( 2.433796855181233454, 74.00833731765563073, 125.2830755159756677 ) ) ;
#26627 = CARTESIAN_POINT ( 'NONE',  ( 109.1589550718174877, -0.001014448720240690048, 0.007507020724817400209 ) ) ;
#26628 = CARTESIAN_POINT ( 'NONE',  ( 13.36082413113061307, -84.67697637120325282, -127.3428651193256940 ) ) ;
#26629 = CARTESIAN_POINT ( 'NONE',  ( -7.733045908741331687, -25.81515396910893045, -45.70676731105710644 ) ) ;
#26630 = B_SPLINE_CURVE_WITH_KNOTS ( 'NONE', 3,
 ( #4004, #4677, #13449, #6190, #23616, #6997, #24564 ),
 .UNSPECIFIED., .F., .F.,
 ( 4, 3, 4 ),
 ( 2.453269466693398621E-17, 0.009512539173626417474, 0.02506242213020847681 ),
 .UNSPECIFIED. ) ;
#26631 = ADVANCED_FACE ( 'NONE', ( #9303 ), #8824, .F. ) ;
#26632 = CARTESIAN_POINT ( 'NONE',  ( -22.34422965417125795, -34.15536449444077505, 16.46028608106144731 ) ) ;
#26633 = B_SPLINE_CURVE_WITH_KNOTS ( 'NONE', 3,
 ( #27710, #6540, #24108, #26243, #18027, #24245 ),
 .UNSPECIFIED., .F., .F.,
 ( 4, 2, 4 ),
 ( 4.286557520396696095E-16, 0.003576372551511235957, 0.007152745103022043437 ),
 .UNSPECIFIED. ) ;
#26634 = CARTESIAN_POINT ( 'NONE',  ( -55.24271866751342941, -0.004365563123935077734, -0.008433070970613952902 ) ) ;
#26635 = CARTESIAN_POINT ( 'NONE',  ( 1.832998868059890096, 96.70023740551124547, 108.1944082009160581 ) ) ;
#26636 = CARTESIAN_POINT ( 'NONE',  ( -55.24271866751342941, -0.009369360294294061531, 0.001545935011626861600 ) ) ;
#26637 = ORIENTED_EDGE ( 'NONE', *, *, #28444, .T. ) ;
#26638 = VERTEX_POINT ( 'NONE', #17496 ) ;
#26640 = EDGE_CURVE ( 'NONE', #19484, #21175, #19374, .T. ) ;
#26639 = CARTESIAN_POINT ( 'NONE',  ( 26.11404676487257603, -22.43340081644687345, -110.9778746459749499 ) ) ;
#26641 = CARTESIAN_POINT ( 'NONE',  ( 25.64681081121879203, 107.2555980796245905, -35.28660243342437752 ) ) ;
#26642 = VERTEX_POINT ( 'NONE', #26142 ) ;
#26643 = ORIENTED_EDGE ( 'NONE', *, *, #20899, .F. ) ;
#26644 = ORIENTED_EDGE ( 'NONE', *, *, #14796, .F. ) ;
#26645 = CARTESIAN_POINT ( 'NONE',  ( 109.1587776205901577, -0.002185517590245302823, -0.006995903587858420293 ) ) ;
#26646 = CARTESIAN_POINT ( 'NONE',  ( 109.1592201516379674, -0.002720803050370518023, -0.007376275279032888654 ) ) ;
#26647 = AXIS2_PLACEMENT_3D ( 'NONE', #25624, #28305, #1828 ) ;
#26648 = CARTESIAN_POINT ( 'NONE',  ( 32.73300124599739291, -103.7392577722171865, -55.46353551262117776 ) ) ;
#26649 = CARTESIAN_POINT ( 'NONE',  ( 26.11404676487259024, -97.48350837663652158, 57.58742681967414256 ) ) ;
#26650 = CARTESIAN_POINT ( 'NONE',  ( -20.57838717382308147, -28.96176188950213870, 7.715628353033985753 ) ) ;
#26651 = ORIENTED_EDGE ( 'NONE', *, *, #2945, .F. ) ;
#26652 = CARTESIAN_POINT ( 'NONE',  ( -9.156249394959706578, 8.027840202793937507, -53.90509764945131366 ) ) ;
#26653 = CARTESIAN_POINT ( 'NONE',  ( 26.11404676487259024, -90.92995828888244603, 67.46175819463337575 ) ) ;
#26654 = CARTESIAN_POINT ( 'NONE',  ( 10.93730112725983439, -148.8212007290663621, 26.59437931460704263 ) ) ;
#26655 = CARTESIAN_POINT ( 'NONE',  ( 1.832998868059890096, -29.64765804470170352, 142.0492247521721936 ) ) ;
#26656 = CARTESIAN_POINT ( 'NONE',  ( 19.66333377628734169, -72.72773398758253904, 116.9853418557801916 ) ) ;
#26657 = CIRCLE ( 'NONE', #20229, 117.6351876552689504 ) ;
#26659 = CARTESIAN_POINT ( 'NONE',  ( 2.430230287190592531, -144.8619874886005903, -13.76600171652791715 ) ) ;
#26658 = CARTESIAN_POINT ( 'NONE',  ( -55.24271866751342941, 0.004365563123935787236, 0.008433070970613791573 ) ) ;
#26660 = EDGE_CURVE ( 'NONE', #17270, #5961, #4691, .T. ) ;
#26661 = CIRCLE ( 'NONE', #14239, 80.00000000000000000 ) ;
#26662 = CARTESIAN_POINT ( 'NONE',  ( 1.833750490713712322, -144.2866297127912389, -15.43355859895807214 ) ) ;
#26663 = CARTESIAN_POINT ( 'NONE',  ( -1.048172774974294619, -36.44231470008696760, 27.73787987941047817 ) ) ;
#26664 = CARTESIAN_POINT ( 'NONE',  ( -20.37983603106074426, 29.73529213200291821, 1.508851015062683487 ) ) ;
#26665 = CARTESIAN_POINT ( 'NONE',  ( -1.619063947482197729, -43.26576862488445130, -16.67502769180545386 ) ) ;
#26666 = CARTESIAN_POINT ( 'NONE',  ( 28.43349137099832191, -116.8557575815931528, 42.22940898499174978 ) ) ;
#26667 = ORIENTED_EDGE ( 'NONE', *, *, #11972, .T. ) ;
#26668 = CARTESIAN_POINT ( 'NONE',  ( -1.045287976400362417, -12.68782741917263657, 44.00138577190661948 ) ) ;
#26670 = AXIS2_PLACEMENT_3D ( 'NONE', #3199, #11978, #26793 ) ;
#26669 =( BOUNDED_SURFACE ( )  B_SPLINE_SURFACE ( 3, 1, ( 
 ( #22348, #2610 ),
 ( #11391, #4921 ),
 ( #13686, #22493 ),
 ( #11532, #10923 ) ),
 .UNSPECIFIED., .F., .F., .F. ) 
 B_SPLINE_SURFACE_WITH_KNOTS ( ( 4, 4 ),
 ( 2, 2 ),
 ( 0.000000000000000000, 1.000000000000000000 ),
 ( 0.000000000000000000, 1.000000000000000000 ),
 .UNSPECIFIED. ) 
 GEOMETRIC_REPRESENTATION_ITEM ( )  RATIONAL_B_SPLINE_SURFACE ( (
 ( 1.000000000000000000, 1.000000000000000000),
 ( 0.9960225298536222738, 0.9999952330161893110),
 ( 0.9960225298536222738, 0.9999952330161893110),
 ( 1.000000000000000000, 1.000000000000000000) ) ) 
 REPRESENTATION_ITEM ( '' )  SURFACE ( )  );
#26671 = ORIENTED_EDGE ( 'NONE', *, *, #6226, .F. ) ;
#26673 = ADVANCED_FACE ( 'NONE', ( #13044 ), #14536, .F. ) ;
#26672 = CARTESIAN_POINT ( 'NONE',  ( -20.57838717382308147, -29.92853265176830746, 1.611677988432673070 ) ) ;
#26674 = CARTESIAN_POINT ( 'NONE',  ( 2.108393763691184031, 1.280847988473803101, -145.2872457912033042 ) ) ;
#26675 = ORIENTED_EDGE ( 'NONE', *, *, #10589, .F. ) ;
#26676 = ORIENTED_EDGE ( 'NONE', *, *, #8471, .T. ) ;
#26677 = EDGE_CURVE ( 'NONE', #18316, #22163, #26552, .T. ) ;
#26678 = ORIENTED_EDGE ( 'NONE', *, *, #23656, .F. ) ;
#26679 = CARTESIAN_POINT ( 'NONE',  ( -12.82751273423876803, -48.09651489336695107, -8.715310691360061313 ) ) ;
#26680 = ORIENTED_EDGE ( 'NONE', *, *, #10823, .T. ) ;
#26681 = CARTESIAN_POINT ( 'NONE',  ( -25.21435515916043357, 16.39063784838743132, -30.48034229288645136 ) ) ;
#26682 = AXIS2_PLACEMENT_3D ( 'NONE', #23811, #15267, #8128 ) ;
#26683 = VECTOR ( 'NONE', #7117, 1000.000000000000000 ) ;
#26684 = CARTESIAN_POINT ( 'NONE',  ( 2.433796855181205476, -84.34988187690851191, -118.5671979538065273 ) ) ;
#26685 = B_SPLINE_CURVE_WITH_KNOTS ( 'NONE', 3,
 ( #15433, #24541, #4804, #22372, #15879, #9547, #7838, #25391, #5668, #9689 ),
 .UNSPECIFIED., .F., .F.,
 ( 4, 3, 3, 4 ),
 ( 0.000000000000000000, 0.0002669560319015579978, 0.0005492286108966487179, 0.0008315040496093540050 ),
 .UNSPECIFIED. ) ;
#26686 = CARTESIAN_POINT ( 'NONE',  ( -55.24271866751342941, 0.008488649505346581442, -0.004256484107793381474 ) ) ;
#26687 = VECTOR ( 'NONE', #5867, 1000.000000000000114 ) ;
#26688 = CARTESIAN_POINT ( 'NONE',  ( 16.75465622695633172, 117.7275519421690149, -79.80233222761897594 ) ) ;
#26689 = DIRECTION ( 'NONE',  ( -1.000000000000000000, -0.000000000000000000, -0.000000000000000000 ) ) ;
#26690 = EDGE_CURVE ( 'NONE', #11148, #28132, #20754, .T. ) ;
#26691 = CARTESIAN_POINT ( 'NONE',  ( 25.73574536432414206, -110.3312765349291737, -24.27578079247274090 ) ) ;
#26692 = CARTESIAN_POINT ( 'NONE',  ( 109.1721716018069515, 0.01616973485710005917, 0.005466227998627309036 ) ) ;
#26693 = PRESENTATION_STYLE_ASSIGNMENT (( #17903 ) ) ;
#26694 = ORIENTED_EDGE ( 'NONE', *, *, #11864, .F. ) ;
#26695 = CARTESIAN_POINT ( 'NONE',  ( -2.265401668238146815, 11.98901689611106036, 45.46007138824028004 ) ) ;
#26696 = CARTESIAN_POINT ( 'NONE',  ( -25.21435515916025594, 34.29329011225976842, -4.655591116594504086 ) ) ;
#26697 = EDGE_CURVE ( 'NONE', #27443, #15365, #24559, .T. ) ;
#26698 = CARTESIAN_POINT ( 'NONE',  ( 1.833206310202334155, 0.7447039688725679563, 145.1075835704899362 ) ) ;
#26699 = CARTESIAN_POINT ( 'NONE',  ( 26.11404676487257603, 90.92995828888292920, -67.46175819463273626 ) ) ;
#26700 = VERTEX_POINT ( 'NONE', #7009 ) ;
#26701 = CARTESIAN_POINT ( 'NONE',  ( 109.1592201516379674, -0.003661068210032719476, 0.006957642258155058955 ) ) ;
#26702 = CIRCLE ( 'NONE', #6510, 151.1787379149930359 ) ;
#26703 = CARTESIAN_POINT ( 'NONE',  ( 26.28373643307405061, -118.1623717393431718, -48.05579805965654572 ) ) ;
#26704 = CARTESIAN_POINT ( 'NONE',  ( -1.259920593601971062, -38.49623866863331045, 25.19630221849093488 ) ) ;
#26705 = VERTEX_POINT ( 'NONE', #2370 ) ;
#26706 = CARTESIAN_POINT ( 'NONE',  ( 28.43349137099835744, 69.71646995966310101, -102.8504004831928853 ) ) ;
#26707 = ORIENTED_EDGE ( 'NONE', *, *, #19535, .F. ) ;
#26708 = AXIS2_PLACEMENT_3D ( 'NONE', #8096, #23640, #4166 ) ;
#26709 = CARTESIAN_POINT ( 'NONE',  ( -21.41430102051744200, -30.75470819672111134, 1.815007301162295805 ) ) ;
#26710 =( BOUNDED_SURFACE ( )  B_SPLINE_SURFACE ( 3, 1, ( 
 ( #7106, #24674 ),
 ( #26792, #22796 ),
 ( #27216, #9830 ),
 ( #4789, #2762 ) ),
 .UNSPECIFIED., .F., .F., .F. ) 
 B_SPLINE_SURFACE_WITH_KNOTS ( ( 4, 4 ),
 ( 2, 2 ),
 ( 0.000000000000000000, 1.000000000000000000 ),
 ( 0.000000000000000000, 1.000000000000000000 ),
 .UNSPECIFIED. ) 
 GEOMETRIC_REPRESENTATION_ITEM ( )  RATIONAL_B_SPLINE_SURFACE ( (
 ( 1.000000000000000000, 1.000000000000000000),
 ( 0.9956975270656954757, 0.8568959468854893125),
 ( 0.9956975270656954757, 0.8568959468854893125),
 ( 1.000000000000000000, 1.000000000000000000) ) ) 
 REPRESENTATION_ITEM ( '' )  SURFACE ( )  );
#26711 = ORIENTED_EDGE ( 'NONE', *, *, #24344, .F. ) ;
#26712 = CARTESIAN_POINT ( 'NONE',  ( 8.186469829614409832, 34.43598812953313626, -145.3272524103319085 ) ) ;
#26713 = VERTEX_POINT ( 'NONE', #15766 ) ;
#26714 = CARTESIAN_POINT ( 'NONE',  ( -25.21435515916043713, -31.17620025257576799, 15.02493970636179377 ) ) ;
#26715 = ORIENTED_EDGE ( 'NONE', *, *, #12002, .F. ) ;
#26716 = CARTESIAN_POINT ( 'NONE',  ( 10.93730112725992676, -65.95960219663038515, -136.0306644680990473 ) ) ;
#26717 = CARTESIAN_POINT ( 'NONE',  ( 25.64699802086724034, 107.3112355540545764, -35.11755197949727147 ) ) ;
#26718 = CARTESIAN_POINT ( 'NONE',  ( -20.20700224038492721, 16.58740185276746359, 24.51628800869029234 ) ) ;
#26719 = CARTESIAN_POINT ( 'NONE',  ( -21.81686047589426991, 6.867757412721210208, 37.90526371014249918 ) ) ;
#26720 = FACE_OUTER_BOUND ( 'NONE', #26519, .T. ) ;
#26721 = ORIENTED_EDGE ( 'NONE', *, *, #26378, .T. ) ;
#26722 = EDGE_CURVE ( 'NONE', #17500, #21826, #14182, .T. ) ;
#26723 = CARTESIAN_POINT ( 'NONE',  ( -25.21435515916043357, -6.169479169075226643, 34.05351380035340014 ) ) ;
#26724 = CARTESIAN_POINT ( 'NONE',  ( 25.98552792386799126, 33.93357582585639420, -107.9280603639523548 ) ) ;
#26725 = CARTESIAN_POINT ( 'NONE',  ( 2.430230287190572103, 60.50928654924933880, -132.3371620660944643 ) ) ;
#26726 = ORIENTED_EDGE ( 'NONE', *, *, #7671, .F. ) ;
#26727 = VECTOR ( 'NONE', #10852, 1000.000000000000000 ) ;
#26728 = EDGE_CURVE ( 'NONE', #26995, #19237, #15273, .T. ) ;
#26729 = VERTEX_POINT ( 'NONE', #22645 ) ;
#26730 = VERTEX_POINT ( 'NONE', #13984 ) ;
#26731 = LINE ( 'NONE', #22438, #8330 ) ;
#26732 = CARTESIAN_POINT ( 'NONE',  ( 1.833485406944043827, -44.33323125129830089, -138.1714136985312962 ) ) ;
#26733 = CARTESIAN_POINT ( 'NONE',  ( -1.056502255334265339, 36.75727364034771938, 27.33667001641128991 ) ) ;
#26734 = EDGE_CURVE ( 'NONE', #9765, #9035, #6116, .T. ) ;
#26735 = CARTESIAN_POINT ( 'NONE',  ( -1.048994561756802391, 0.7655149579823430361, -45.79144455904140187 ) ) ;
#26736 = CARTESIAN_POINT ( 'NONE',  ( -25.21435515916043713, 16.39063784838786475, 30.48034229288620622 ) ) ;
#26737 = CARTESIAN_POINT ( 'NONE',  ( -20.20700224038492365, 23.35150625415685255, 18.19058640100197977 ) ) ;
#26738 = CARTESIAN_POINT ( 'NONE',  ( 25.64681081121879203, -91.10197563707900770, -66.70335573067958990 ) ) ;
#26739 = ORIENTED_EDGE ( 'NONE', *, *, #14796, .T. ) ;
#26740 = CARTESIAN_POINT ( 'NONE',  ( 109.1586900883932856, 0.006561743627145262027, 0.002810909342002427570 ) ) ;
#26741 = CARTESIAN_POINT ( 'NONE',  ( -7.078251931573406708, -51.82710018979472721, 5.101176922831208493 ) ) ;
#26742 = CARTESIAN_POINT ( 'NONE',  ( 1.833206308920094729, -58.34024961171146373, -132.8652726225758158 ) ) ;
#26743 = CARTESIAN_POINT ( 'NONE',  ( 109.1778270068192853, 0.009220257877180842651, -0.001322180554001304307 ) ) ;
#26744 = VERTEX_POINT ( 'NONE', #3195 ) ;
#26745 = CARTESIAN_POINT ( 'NONE',  ( 109.1778270068192853, 0.007152128381194052670, -0.005967275455169908024 ) ) ;
#26746 = EDGE_LOOP ( 'NONE', ( #20135, #3751, #20660, #18993 ) ) ;
#26747 = CARTESIAN_POINT ( 'NONE',  ( 32.73300124599738581, 8.473903470907664826, -117.3295799645428588 ) ) ;
#26748 = ORIENTED_EDGE ( 'NONE', *, *, #3803, .F. ) ;
#26749 = CONICAL_SURFACE ( 'NONE', #11127, 117.6351876552689504, 0.9945805576725580410 ) ;
#26750 = ORIENTED_EDGE ( 'NONE', *, *, #28081, .F. ) ;
#26751 = VERTEX_POINT ( 'NONE', #24672 ) ;
#26753 =( BOUNDED_SURFACE ( )  B_SPLINE_SURFACE ( 3, 1, ( 
 ( #12722, #8989 ),
 ( #15151, #23974 ),
 ( #15437, #11002 ),
 ( #17607, #26247 ) ),
 .UNSPECIFIED., .F., .F., .F. ) 
 B_SPLINE_SURFACE_WITH_KNOTS ( ( 4, 4 ),
 ( 2, 2 ),
 ( 0.000000000000000000, 1.000000000000000000 ),
 ( 0.000000000000000000, 1.000000000000000000 ),
 .UNSPECIFIED. ) 
 GEOMETRIC_REPRESENTATION_ITEM ( )  RATIONAL_B_SPLINE_SURFACE ( (
 ( 1.000000000000000000, 1.000000000000000000),
 ( 0.9956975270656954757, 0.8568959468854893125),
 ( 0.9956975270656954757, 0.8568959468854893125),
 ( 1.000000000000000000, 1.000000000000000000) ) ) 
 REPRESENTATION_ITEM ( '' )  SURFACE ( )  );
#26752 = CIRCLE ( 'NONE', #28131, 117.6351876552689504 ) ;
#26754 = B_SPLINE_CURVE_WITH_KNOTS ( 'NONE', 3,
 ( #3268, #21094, #18802, #20668, #14049, #18950 ),
 .UNSPECIFIED., .F., .F.,
 ( 4, 2, 4 ),
 ( 1.504716382203053018E-16, 0.003570751334075636125, 0.007141502668151121329 ),
 .UNSPECIFIED. ) ;
#26755 = CARTESIAN_POINT ( 'NONE',  ( -55.24271866751342941, -0.008433070970613520956, 0.004365563123935277227 ) ) ;
#26756 = FACE_OUTER_BOUND ( 'NONE', #8257, .T. ) ;
#26757 = CARTESIAN_POINT ( 'NONE',  ( 25.69398547355842410, 57.11291030433652338, 97.43788956976163718 ) ) ;
#26758 = ADVANCED_FACE ( 'NONE', ( #20604 ), #1512, .T. ) ;
#26759 = CARTESIAN_POINT ( 'NONE',  ( 119.2224693531408803, -69.99999999999998579, 40.00000000000003553 ) ) ;
#26760 = ORIENTED_EDGE ( 'NONE', *, *, #18252, .F. ) ;
#26761 = CARTESIAN_POINT ( 'NONE',  ( 8.186469829614290816, -143.0750865143070598, 42.84118568057157006 ) ) ;
#26762 = CARTESIAN_POINT ( 'NONE',  ( 25.87036335909425588, 45.07965203035060142, -103.6841944152901505 ) ) ;
#26763 = CARTESIAN_POINT ( 'NONE',  ( -8.786685647604898008, 48.22796981442802178, 23.24040270374343464 ) ) ;
#26764 = ORIENTED_EDGE ( 'NONE', *, *, #17287, .T. ) ;
#26765 = ADVANCED_FACE ( 'NONE', ( #26931 ), #915, .F. ) ;
#26766 = DIRECTION ( 'NONE',  ( -0.5914120900931443270, 0.09226095020377932110, 0.8010740644654240628 ) ) ;
#26767 = EDGE_LOOP ( 'NONE', ( #20003, #21225, #7579, #18768 ) ) ;
#26768 = CARTESIAN_POINT ( 'NONE',  ( 1.833838850093465700, 141.9387658801234977, -30.17001957361848241 ) ) ;
#26769 = CARTESIAN_POINT ( 'NONE',  ( 25.64700659047697329, -45.71714758798305667, -103.2418925369177316 ) ) ;
#26770 = CARTESIAN_POINT ( 'NONE',  ( -8.786685647604898008, 48.22796981442802178, 23.24040270374343464 ) ) ;
#26771 = CARTESIAN_POINT ( 'NONE',  ( 10.93730112725992853, -56.95489579269655422, -140.0398180619117738 ) ) ;
#26772 = CARTESIAN_POINT ( 'NONE',  ( -55.25297051322618813, -0.001818774723749082148, -0.01483298743814642773 ) ) ;
#26773 = VECTOR ( 'NONE', #15006, 1000.000000000000114 ) ;
#26774 = EDGE_CURVE ( 'NONE', #25292, #4874, #2173, .T. ) ;
#26775 = CARTESIAN_POINT ( 'NONE',  ( -15.02187109954785704, -33.49412687891593521, -32.04062513125103351 ) ) ;
#26776 = CARTESIAN_POINT ( 'NONE',  ( -4.780792508754313275, -25.98388465890110410, -42.16805077400949386 ) ) ;
#26777 = AXIS2_PLACEMENT_3D ( 'NONE', #12976, #25809, #19597 ) ;
#26778 = CARTESIAN_POINT ( 'NONE',  ( 8.186469829614395621, 19.05650981810018862, -148.1306754360699927 ) ) ;
#26779 = CARTESIAN_POINT ( 'NONE',  ( -8.786685647604887350, -38.68584556812326980, -37.00619870957918778 ) ) ;
#26780 = CARTESIAN_POINT ( 'NONE',  ( 25.64681081121879203, 56.81519825470756047, 97.57530875170624540 ) ) ;
#26781 = CARTESIAN_POINT ( 'NONE',  ( -1.619063947482197729, 38.92136151114943488, 25.20140673341330739 ) ) ;
#26782 = ORIENTED_EDGE ( 'NONE', *, *, #11580, .F. ) ;
#26783 = ORIENTED_EDGE ( 'NONE', *, *, #5469, .T. ) ;
#26784 = CARTESIAN_POINT ( 'NONE',  ( -1.619063947482197729, -43.26576862488421682, 16.67502769180607203 ) ) ;
#26785 = CARTESIAN_POINT ( 'NONE',  ( 10.93730112725969938, 71.28103789254939215, 133.3192575531800799 ) ) ;
#26786 = VERTEX_POINT ( 'NONE', #24517 ) ;
#26787 = ORIENTED_EDGE ( 'NONE', *, *, #1268, .F. ) ;
#26788 = AXIS2_PLACEMENT_3D ( 'NONE', #7775, #16682, #10725 ) ;
#26789 = EDGE_LOOP ( 'NONE', ( #17430, #15202, #12567, #8197 ) ) ;
#26790 = CARTESIAN_POINT ( 'NONE',  ( -20.38016308990358638, 29.73560196176844528, -1.509191766064308382 ) ) ;
#26791 = CIRCLE ( 'NONE', #7531, 151.1787379149930359 ) ;
#26792 = CARTESIAN_POINT ( 'NONE',  ( 109.1589550718174877, -0.007553890059312251028, 0.0005685167901298121941 ) ) ;
#26793 = DIRECTION ( 'NONE',  ( 0.000000000000000000, 0.000000000000000000, 1.000000000000000000 ) ) ;
#26794 = AXIS2_PLACEMENT_3D ( 'NONE', #23760, #21985, #17107 ) ;
#26795 = ADVANCED_FACE ( 'NONE', ( #23951 ), #5534, .F. ) ;
#26796 = EDGE_CURVE ( 'NONE', #6523, #12888, #1947, .T. ) ;
#26797 = CARTESIAN_POINT ( 'NONE',  ( -55.24340739397742084, -0.007744344507854280558, -0.006539691034612628989 ) ) ;
#26798 = B_SPLINE_CURVE_WITH_KNOTS ( 'NONE', 3,
 ( #28446, #14663, #25758, #23615, #28036, #17101 ),
 .UNSPECIFIED., .F., .F.,
 ( 4, 2, 4 ),
 ( 0.000000000000000000, 0.0004335151646191514122, 0.0008670303292383013064 ),
 .UNSPECIFIED. ) ;
#26799 = B_SPLINE_CURVE_WITH_KNOTS ( 'NONE', 3,
 ( #23525, #25811, #3788, #6628, #1621, #7993, #5671 ),
 .UNSPECIFIED., .F., .F.,
 ( 4, 3, 4 ),
 ( 6.019590444871180375E-16, 0.02816610861753244058, 0.04000277880656280538 ),
 .UNSPECIFIED. ) ;
#26800 = CARTESIAN_POINT ( 'NONE',  ( 26.11404676487257603, -74.91683232330916553, -84.89295829319569009 ) ) ;
#26801 = CARTESIAN_POINT ( 'NONE',  ( 2.430230287190581429, -142.6294793592099666, 28.83279105684380639 ) ) ;
#26802 = EDGE_CURVE ( 'NONE', #12561, #20253, #16639, .T. ) ;
#26803 = CARTESIAN_POINT ( 'NONE',  ( -25.21435515916043357, -6.169479169075226643, 34.05351380035340014 ) ) ;
#26804 = CARTESIAN_POINT ( 'NONE',  ( -1.058197053496172213, 42.99116279335175506, 15.81317659443640444 ) ) ;
#26805 = CARTESIAN_POINT ( 'NONE',  ( 21.16825799904903960, 4.416019842158419806, 135.3612955721067408 ) ) ;
#26806 = CARTESIAN_POINT ( 'NONE',  ( 1.831572820252009626, -117.9752562883661255, -84.49389457294256545 ) ) ;
#26807 = CARTESIAN_POINT ( 'NONE',  ( -20.20700224038492010, -18.19058640100240254, -23.35150625415651859 ) ) ;
#26808 = EDGE_CURVE ( 'NONE', #1423, #8797, #820, .T. ) ;
#26809 = CARTESIAN_POINT ( 'NONE',  ( -1.044556982611273277, 12.57890920527776224, -44.03203163107531282 ) ) ;
#26810 = FACE_OUTER_BOUND ( 'NONE', #19539, .T. ) ;
#26811 = CARTESIAN_POINT ( 'NONE',  ( -1.239374126674604337, 25.08410696974298304, 38.61989855450910625 ) ) ;
#26812 = ORIENTED_EDGE ( 'NONE', *, *, #716, .T. ) ;
#26814 = CARTESIAN_POINT ( 'NONE',  ( -5.986830583229487246, -49.46736940480267464, -11.27873876172122181 ) ) ;
#26813 = CARTESIAN_POINT ( 'NONE',  ( -15.02187109954782507, 8.264310930413024892, 45.60876405941875333 ) ) ;
#26815 = CARTESIAN_POINT ( 'NONE',  ( -1.045287976400383290, 36.12803364096649972, 28.14015102489766917 ) ) ;
#26816 = CARTESIAN_POINT ( 'NONE',  ( 1.834118845439484335, -125.5799175751964754, -72.70910183320698650 ) ) ;
#26817 = CARTESIAN_POINT ( 'NONE',  ( -1.464342487929851222, 16.57334911911573982, 43.13914623307943685 ) ) ;
#26818 = ADVANCED_FACE ( 'NONE', ( #15787 ), #23387, .F. ) ;
#26819 = ORIENTED_EDGE ( 'NONE', *, *, #20722, .T. ) ;
#26820 = CARTESIAN_POINT ( 'NONE',  ( -1.019300379054419947, 16.06793277091992067, -42.90269154183433642 ) ) ;
#26821 = VERTEX_POINT ( 'NONE', #22202 ) ;
#26822 = CARTESIAN_POINT ( 'NONE',  ( -25.21435515916025594, 1.749597353048488237E-16, -4.373993382621220594E-17 ) ) ;
#26823 = CARTESIAN_POINT ( 'NONE',  ( -55.24300891470648622, -0.009812809446890113918, -0.0003472257464246985225 ) ) ;
#26824 = ORIENTED_EDGE ( 'NONE', *, *, #13546, .F. ) ;
#26825 = CARTESIAN_POINT ( 'NONE',  ( -1.113427685306992876, -28.52429901637193410, -35.91272432484649357 ) ) ;
#26826 = VERTEX_POINT ( 'NONE', #27259 ) ;
#26827 = CARTESIAN_POINT ( 'NONE',  ( 1.833721034905664959, -97.36162733017636128, -107.5990973104333079 ) ) ;
#26828 = VERTEX_POINT ( 'NONE', #22688 ) ;
#26829 = CARTESIAN_POINT ( 'NONE',  ( 2.063896406836605024, 60.31174178979986777, -132.1577797566299921 ) ) ;
#26830 = CIRCLE ( 'NONE', #13977, 151.1787379149930359 ) ;
#26831 = EDGE_CURVE ( 'NONE', #22079, #9286, #5991, .T. ) ;
#26832 = CARTESIAN_POINT ( 'NONE',  ( 2.108393763691180478, 125.1820217068196115, 73.75286979200500070 ) ) ;
#26833 = CARTESIAN_POINT ( 'NONE',  ( 10.93730112726006354, 145.2260730187408626, -42.00474393596100953 ) ) ;
#26834 = DIRECTION ( 'NONE',  ( 1.000000000000000000, -6.938893903907226837E-18, 1.734723475976806709E-18 ) ) ;
#26835 = ADVANCED_FACE ( 'NONE', ( #3233 ), #15592, .F. ) ;
#26836 = FACE_OUTER_BOUND ( 'NONE', #8209, .T. ) ;
#26837 = CARTESIAN_POINT ( 'NONE',  ( 26.28373643307434548, 67.34887744616764849, 108.3320567927989231 ) ) ;
#26838 = FACE_OUTER_BOUND ( 'NONE', #19637, .T. ) ;
#26839 = CARTESIAN_POINT ( 'NONE',  ( -1.045287976400351981, -15.59869763335126436, -43.05558670614231431 ) ) ;
#26840 = CARTESIAN_POINT ( 'NONE',  ( -1.045287976400362417, -1.530335034934427574, -45.76855895860943235 ) ) ;
#26841 = ORIENTED_EDGE ( 'NONE', *, *, #7138, .F. ) ;
#26842 = CARTESIAN_POINT ( 'NONE',  ( -1.031422197589711764, -1.530725436377143867, 45.78027046666444022 ) ) ;
#26843 = CARTESIAN_POINT ( 'NONE',  ( -1.045287976400379737, -37.92705037016725100, 25.66401692420055269 ) ) ;
#26844 = CARTESIAN_POINT ( 'NONE',  ( 25.64670758986458310, -84.24158725144673099, 75.18147256662025768 ) ) ;
#26845 = CARTESIAN_POINT ( 'NONE',  ( 10.93730112726005821, 140.0398180619120865, -56.95489579269602842 ) ) ;
#26846 = CARTESIAN_POINT ( 'NONE',  ( 2.433796855181219243, 86.69855925933974561, 116.8607839509059829 ) ) ;
#26847 = ORIENTED_EDGE ( 'NONE', *, *, #17307, .F. ) ;
#26848 = CARTESIAN_POINT ( 'NONE',  ( 10.93730112725932813, 151.0983828010088246, -4.928439153520510985 ) ) ;
#26849 = CARTESIAN_POINT ( 'NONE',  ( 30.58324630866340854, -112.0331114996531454, -45.56259622822469879 ) ) ;
#26850 = CARTESIAN_POINT ( 'NONE',  ( 16.05277956358233027, 87.96830019103632026, 113.1291064380262270 ) ) ;
#26851 = EDGE_LOOP ( 'NONE', ( #19159, #14599, #8761, #5090 ) ) ;
#26852 = CARTESIAN_POINT ( 'NONE',  ( 109.1586900883932856, -0.005715190711481754789, 0.004277182003227202392 ) ) ;
#26853 = ORIENTED_EDGE ( 'NONE', *, *, #25079, .F. ) ;
#26854 = CARTESIAN_POINT ( 'NONE',  ( 26.11404676487257603, -112.7148551500681037, 10.71016160607530310 ) ) ;
#26855 = CARTESIAN_POINT ( 'NONE',  ( 24.01988960052061373, 9.440825210283430025, 130.7041393974934635 ) ) ;
#26856 = ORIENTED_EDGE ( 'NONE', *, *, #22231, .F. ) ;
#26857 = CARTESIAN_POINT ( 'NONE',  ( 13.36082413113063083, -150.7747251079860291, -25.56125765253606730 ) ) ;
#26858 = VECTOR ( 'NONE', #16112, 999.9999999999998863 ) ;
#26859 = ORIENTED_EDGE ( 'NONE', *, *, #21634, .F. ) ;
#26860 = B_SPLINE_CURVE_WITH_KNOTS ( 'NONE', 3,
 ( #6609, #6464, #21860, #17385, #10647, #21719, #2256 ),
 .UNSPECIFIED., .F., .F.,
 ( 4, 3, 4 ),
 ( 2.619375006920453907E-17, 0.02816610861753245793, 0.04000277880656212537 ),
 .UNSPECIFIED. ) ;
#26861 = CARTESIAN_POINT ( 'NONE',  ( -55.24340739397742084, -0.003826481709803442217, 0.009386184976286439385 ) ) ;
#26862 = ADVANCED_FACE ( 'NONE', ( #18634 ), #27215, .F. ) ;
#26863 = VERTEX_POINT ( 'NONE', #18326 ) ;
#26864 = CARTESIAN_POINT ( 'NONE',  ( 25.64681081121880624, 103.3177883989785499, -45.54494737132120008 ) ) ;
#26865 = CARTESIAN_POINT ( 'NONE',  ( -20.57838717382308147, -10.78122205917020437, -27.96569011373082603 ) ) ;
#26866 = ADVANCED_FACE ( 'NONE', ( #27107 ), #24291, .F. ) ;
#26867 = CARTESIAN_POINT ( 'NONE',  ( 25.64704443564076541, -35.01840413910206706, 107.3436266109712420 ) ) ;
#26868 = CARTESIAN_POINT ( 'NONE',  ( 24.01988960052062794, -130.9749633972836591, -4.273195451970020819 ) ) ;
#26869 = CARTESIAN_POINT ( 'NONE',  ( -1.155001620486262759, 16.13799328198422245, -42.97366440495917317 ) ) ;
#26870 = LINE ( 'NONE', #15934, #8345 ) ;
#26871 = EDGE_CURVE ( 'NONE', #4178, #27450, #27945, .T. ) ;
#26872 = ORIENTED_EDGE ( 'NONE', *, *, #16880, .T. ) ;
#26873 = CARTESIAN_POINT ( 'NONE',  ( 16.75465622695642764, -62.05388459345985552, 127.9746229614485458 ) ) ;
#26874 = CARTESIAN_POINT ( 'NONE',  ( -55.24198130335446422, -0.006617369590171728877, 0.006527480770973505091 ) ) ;
#26875 = CARTESIAN_POINT ( 'NONE',  ( -23.77929240705205771, -25.06639637888440220, -26.20227034809546041 ) ) ;
#26876 = VERTEX_POINT ( 'NONE', #10851 ) ;
#26877 = VERTEX_POINT ( 'NONE', #28108 ) ;
#26878 = ORIENTED_EDGE ( 'NONE', *, *, #8812, .F. ) ;
#26879 = LINE ( 'NONE', #20255, #17509 ) ;
#26880 = FACE_OUTER_BOUND ( 'NONE', #6349, .T. ) ;
#26881 = CARTESIAN_POINT ( 'NONE',  ( -1.155001620486248548, -38.31519699443482097, 25.28075036143263077 ) ) ;
#26882 = CARTESIAN_POINT ( 'NONE',  ( 28.37644542392848734, 42.25924161794038270, -116.9383271603240360 ) ) ;
#26883 = CARTESIAN_POINT ( 'NONE',  ( -23.77929240705188008, 35.93174012244194415, -4.877832571065094491 ) ) ;
#26884 = CARTESIAN_POINT ( 'NONE',  ( -20.90916690077961704, -28.59207721780126477, 27.35210456531406109 ) ) ;
#26885 = CARTESIAN_POINT ( 'NONE',  ( -20.47566262905010603, 1.586617686065558974, -29.82700878811084522 ) ) ;
#26886 = VERTEX_POINT ( 'NONE', #8269 ) ;
#26887 = CARTESIAN_POINT ( 'NONE',  ( 16.75465622695658041, -133.7599617830022964, -48.33695624543456404 ) ) ;
#26888 = CARTESIAN_POINT ( 'NONE',  ( 2.433796855181205476, -98.43889364293931976, 107.1581411821782268 ) ) ;
#26889 = CARTESIAN_POINT ( 'NONE',  ( 1.832998868059858122, 145.1092030902949830, -0.5339089137753102454 ) ) ;
#26890 = CARTESIAN_POINT ( 'NONE',  ( -25.21435515916043713, 4.655591116594827383, 34.29329011225949841 ) ) ;
#26891 = CARTESIAN_POINT ( 'NONE',  ( 9.884929003653608603, 91.84919534722101275, -119.2676479132364733 ) ) ;
#26892 = ORIENTED_EDGE ( 'NONE', *, *, #26924, .F. ) ;
#26893 = CARTESIAN_POINT ( 'NONE',  ( 55.79472521941426777, -72.27573336313946584, -8.328398066092509211 ) ) ;
#26894 =( BOUNDED_SURFACE ( )  B_SPLINE_SURFACE ( 3, 1, ( 
 ( #13282, #26524 ),
 ( #329, #11560 ),
 ( #20337, #6829 ),
 ( #629, #17747 ) ),
 .UNSPECIFIED., .F., .F., .F. ) 
 B_SPLINE_SURFACE_WITH_KNOTS ( ( 4, 4 ),
 ( 2, 2 ),
 ( 0.000000000000000000, 1.000000000000000000 ),
 ( 0.000000000000000000, 1.000000000000000000 ),
 .UNSPECIFIED. ) 
 GEOMETRIC_REPRESENTATION_ITEM ( )  RATIONAL_B_SPLINE_SURFACE ( (
 ( 1.000000000000000000, 1.000000000000000000),
 ( 0.9593753223639863714, 0.9995975284513187731),
 ( 0.9593753223639863714, 0.9995975284513187731),
 ( 1.000000000000000000, 1.000000000000000000) ) ) 
 REPRESENTATION_ITEM ( '' )  SURFACE ( )  );
#26895 = ORIENTED_EDGE ( 'NONE', *, *, #31, .F. ) ;
#26896 = CARTESIAN_POINT ( 'NONE',  ( 1.833485406944043827, -108.1939177044932592, 96.69979900902130510 ) ) ;
#26897 = ORIENTED_EDGE ( 'NONE', *, *, #28325, .T. ) ;
#26898 = ORIENTED_EDGE ( 'NONE', *, *, #6361, .F. ) ;
#26899 = EDGE_CURVE ( 'NONE', #22237, #7969, #17281, .T. ) ;
#26900 = ORIENTED_EDGE ( 'NONE', *, *, #648, .F. ) ;
#26901 = EDGE_CURVE ( 'NONE', #5673, #6096, #12844, .T. ) ;
#26902 = FACE_OUTER_BOUND ( 'NONE', #4243, .T. ) ;
#26903 = CARTESIAN_POINT ( 'NONE',  ( 109.1589550718175161, -0.007008495014555500037, -0.002874971999837398241 ) ) ;
#26904 = CARTESIAN_POINT ( 'NONE',  ( 1.832998868059858122, -108.1944082009150776, -96.70023740551231128 ) ) ;
#26905 = DIRECTION ( 'NONE',  ( -5.541455922705464902E-20, 5.223019709708320524E-21, -1.000000000000000000 ) ) ;
#26906 = ORIENTED_EDGE ( 'NONE', *, *, #17863, .T. ) ;
#26907 = CARTESIAN_POINT ( 'NONE',  ( 2.263178607246673746, 13.80342482180279262, -144.7392885066941517 ) ) ;
#26908 = CARTESIAN_POINT ( 'NONE',  ( 25.64681081121879203, 45.54494737132363724, -103.3177883989774841 ) ) ;
#26909 = CARTESIAN_POINT ( 'NONE',  ( 10.93730112725932635, 0.000000000000000000, 0.000000000000000000 ) ) ;
#26910 = EDGE_LOOP ( 'NONE', ( #9067, #18626, #5887, #3791 ) ) ;
#26911 = EDGE_LOOP ( 'NONE', ( #17889, #5345, #19660, #4259 ) ) ;
#26912 = CARTESIAN_POINT ( 'NONE',  ( -55.24271866751342941, 0.008433070970614256479, -0.004365563123935527895 ) ) ;
#26913 = CARTESIAN_POINT ( 'NONE',  ( -1.464342487929863212, 43.13914623307960738, -16.57334911911526731 ) ) ;
#26914 = CARTESIAN_POINT ( 'NONE',  ( 2.263178113027050298, -145.3892419963350733, -1.401567040889715621 ) ) ;
#26915 = CARTESIAN_POINT ( 'NONE',  ( 13.84597867724980880, 25.80666409311568188, 144.4146018799363560 ) ) ;
#26916 = LINE ( 'NONE', #24500, #26234 ) ;
#26917 = DIRECTION ( 'NONE',  ( -1.000000000000000000, -0.000000000000000000, -0.000000000000000000 ) ) ;
#26918 = CARTESIAN_POINT ( 'NONE',  ( -20.57838717382308147, -18.89542499756482741, 23.26537097894125594 ) ) ;
#26919 = B_SPLINE_CURVE_WITH_KNOTS ( 'NONE', 3,
 ( #11147, #8699, #2063, #12861, #21654, #19768, #21941, #11007, #24253, #19629, #8560, #27989, #17326 ),
 .UNSPECIFIED., .F., .F.,
 ( 4, 3, 3, 3, 4 ),
 ( 9.813077866773594792E-18, 0.0007657099931970512375, 0.001531419946797918071, 0.002296279302920157302, 0.003061450627205767206 ),
 .UNSPECIFIED. ) ;
#26920 = CARTESIAN_POINT ( 'NONE',  ( -6.588769196390753535, -38.42957692275866322, -34.04709086065298607 ) ) ;
#26921 = CARTESIAN_POINT ( 'NONE',  ( -8.786685647604890903, -47.14957014837335691, 25.35688121747554291 ) ) ;
#26922 = CARTESIAN_POINT ( 'NONE',  ( 25.81918753295380142, -107.7789657594972255, -34.03777907512026246 ) ) ;
#26923 = ORIENTED_EDGE ( 'NONE', *, *, #19615, .F. ) ;
#26924 = EDGE_CURVE ( 'NONE', #10427, #13097, #6122, .T. ) ;
#26925 = EDGE_LOOP ( 'NONE', ( #21887, #25187, #15414, #21343 ) ) ;
#26926 = CARTESIAN_POINT ( 'NONE',  ( -23.79248802219730052, 24.83956736572410051, -22.01156985585177495 ) ) ;
#26927 = VERTEX_POINT ( 'NONE', #17176 ) ;
#26928 = ORIENTED_EDGE ( 'NONE', *, *, #8376, .T. ) ;
#26929 = EDGE_CURVE ( 'NONE', #8439, #23751, #17032, .T. ) ;
#26930 = ORIENTED_EDGE ( 'NONE', *, *, #16250, .T. ) ;
#26931 = FACE_OUTER_BOUND ( 'NONE', #2702, .T. ) ;
#26932 = CARTESIAN_POINT ( 'NONE',  ( -1.045287976400351981, 36.12803364096590997, -28.14015102489844011 ) ) ;
#26933 = EDGE_CURVE ( 'NONE', #20203, #6666, #1830, .T. ) ;
#26934 = CARTESIAN_POINT ( 'NONE',  ( -1.045287976400362417, 43.05558670614268379, 15.59869763335023229 ) ) ;
#26935 = CARTESIAN_POINT ( 'NONE',  ( -1.031422197589716205, -44.01264471863856897, -12.69107518035485782 ) ) ;
#26936 = UNCERTAINTY_MEASURE_WITH_UNIT (LENGTH_MEASURE( 1.000000000000000082E-05 ), #22572, 'distance_accuracy_value', 'NONE');
#26937 = CARTESIAN_POINT ( 'NONE',  ( -20.21097721712959938, -24.14932359587277233, 17.13687106192370280 ) ) ;
#26938 = CARTESIAN_POINT ( 'NONE',  ( 32.73300124599739291, -108.9684813982485707, -44.31599526638064646 ) ) ;
#26939 = CARTESIAN_POINT ( 'NONE',  ( 25.98552792386799837, -74.89816102339773352, 84.79516057869859935 ) ) ;
#26940 = LINE ( 'NONE', #26071, #5147 ) ;
#26941 = B_SPLINE_CURVE_WITH_KNOTS ( 'NONE', 3,
 ( #11516, #20293, #24072, #4758, #13529, #4900 ),
 .UNSPECIFIED., .F., .F.,
 ( 4, 2, 4 ),
 ( 2.168404344971008868E-18, 0.0006311636237756730562, 0.001262327247551343727 ),
 .UNSPECIFIED. ) ;
#26942 = CARTESIAN_POINT ( 'NONE',  ( 2.108985857320901935, 60.26444811757399833, 132.2056553747747785 ) ) ;
#26943 = CARTESIAN_POINT ( 'NONE',  ( -21.41427618760457818, -16.60878262545437778, -25.94789270595500597 ) ) ;
#26944 = CARTESIAN_POINT ( 'NONE',  ( 8.186469829613955085, 145.3272524103320222, 34.43598812953141675 ) ) ;
#26945 = ORIENTED_EDGE ( 'NONE', *, *, #8433, .F. ) ;
#26946 = B_SPLINE_CURVE_WITH_KNOTS ( 'NONE', 3,
 ( #4440, #26461, #17262, #12943, #15232, #130, #9058, #15651 ),
 .UNSPECIFIED., .F., .F.,
 ( 4, 2, 2, 4 ),
 ( 0.000000000000000000, 0.002761524886576650645, 0.005523049773153301291, 0.01104609954630661299 ),
 .UNSPECIFIED. ) ;
#26947 = VECTOR ( 'NONE', #20440, 999.9999999999998863 ) ;
#26948 = CARTESIAN_POINT ( 'NONE',  ( -24.53237795827027767, -29.54731592868574808, -16.68575684089485023 ) ) ;
#26949 = CARTESIAN_POINT ( 'NONE',  ( 25.64670758986457955, -22.98827151089207632, -110.5460908981864776 ) ) ;
#26950 = CARTESIAN_POINT ( 'NONE',  ( -28.41354790283022069, -18.00456980371888704, 14.62505768302820464 ) ) ;
#26951 = CARTESIAN_POINT ( 'NONE',  ( -1.044556982611269502, 15.70482750345296452, 43.01635920718332784 ) ) ;
#26952 = VERTEX_POINT ( 'NONE', #8138 ) ;
#26953 = CARTESIAN_POINT ( 'NONE',  ( 1.833750490713697223, -14.90257883162655084, -144.3424379351781681 ) ) ;
#26954 = EDGE_CURVE ( 'NONE', #12126, #4463, #464, .T. ) ;
#26955 = ORIENTED_EDGE ( 'NONE', *, *, #14433, .F. ) ;
#26956 = CARTESIAN_POINT ( 'NONE',  ( 1.833206310202330602, -84.68961945193537133, 117.8322271314361558 ) ) ;
#26957 = CARTESIAN_POINT ( 'NONE',  ( 25.64681081121879203, -12.21581276189883170, 112.2483031020013016 ) ) ;
#26958 = VERTEX_POINT ( 'NONE', #12710 ) ;
#26959 = EDGE_CURVE ( 'NONE', #22124, #16228, #13517, .T. ) ;
#26960 = ORIENTED_EDGE ( 'NONE', *, *, #26036, .T. ) ;
#26961 = ORIENTED_EDGE ( 'NONE', *, *, #10630, .T. ) ;
#26962 = ADVANCED_FACE ( 'NONE', ( #14875 ), #1660, .F. ) ;
#26963 = ORIENTED_EDGE ( 'NONE', *, *, #24011, .T. ) ;
#26964 = CARTESIAN_POINT ( 'NONE',  ( -8.786685647604896232, 25.35688121747570278, 47.14957014837326454 ) ) ;
#26965 = EDGE_CURVE ( 'NONE', #17046, #10778, #16904, .T. ) ;
#26966 = CARTESIAN_POINT ( 'NONE',  ( -1.583189561560252701, 25.21827308671288392, 38.94740041318267032 ) ) ;
#26967 = CARTESIAN_POINT ( 'NONE',  ( 109.1586059443104944, 0.006637156007970154009, -0.002447596125914190766 ) ) ;
#26968 = CARTESIAN_POINT ( 'NONE',  ( 28.37644542392835234, 102.9230687709019634, -69.76573497038990013 ) ) ;
#26969 = CARTESIAN_POINT ( 'NONE',  ( -1.019300379054419947, -28.53917295602871818, 35.83762006677432055 ) ) ;
#26970 = B_SPLINE_CURVE_WITH_KNOTS ( 'NONE', 3,
 ( #52, #13858, #11417, #15728 ),
 .UNSPECIFIED., .F., .F.,
 ( 4, 4 ),
 ( 3.405187508996590202E-16, 0.01077107486149765994 ),
 .UNSPECIFIED. ) ;
#26971 = CARTESIAN_POINT ( 'NONE',  ( -20.20700224038492010, 8.199606986804733211, 28.44216453106527709 ) ) ;
#26972 = CARTESIAN_POINT ( 'NONE',  ( -1.050231094221210082, 26.71409683968617799, -37.20185272688468814 ) ) ;
#26973 = CARTESIAN_POINT ( 'NONE',  ( -1.046936909428682005, 1.275306677858881743, 45.77873603877004882 ) ) ;
#26974 = ORIENTED_EDGE ( 'NONE', *, *, #18448, .T. ) ;
#26975 = CARTESIAN_POINT ( 'NONE',  ( 32.73300124599734318, 16.10546300444822165, 116.5274707358856290 ) ) ;
#26977 = CARTESIAN_POINT ( 'NONE',  ( 25.64670758986457955, 56.88615781331626664, -97.53391148296614688 ) ) ;
#26976 = CARTESIAN_POINT ( 'NONE',  ( 25.64692232868534560, 66.10288322707316411, -91.53874134430731146 ) ) ;
#26978 = CARTESIAN_POINT ( 'NONE',  ( 2.108985857320881507, 1.281428372375777114, 145.2876352664463013 ) ) ;
#26979 = FILL_AREA_STYLE ('',( #20804 ) ) ;
#26980 = CARTESIAN_POINT ( 'NONE',  ( -24.53239521893653219, 24.99972072650176713, 22.94500969220215580 ) ) ;
#26981 = LINE ( 'NONE', #22849, #6090 ) ;
#26982 = CARTESIAN_POINT ( 'NONE',  ( 25.86096068574578055, 110.7864907291861130, -22.52859312382080503 ) ) ;
#26983 = LINE ( 'NONE', #20379, #11171 ) ;
#26984 = ORIENTED_EDGE ( 'NONE', *, *, #17412, .F. ) ;
#26985 = B_SPLINE_CURVE_WITH_KNOTS ( 'NONE', 3,
 ( #14590, #23395, #19328, #8266, #10431, #14873 ),
 .UNSPECIFIED., .F., .F.,
 ( 4, 2, 4 ),
 ( 7.757919228897728493E-18, 0.003570751334075633956, 0.007141502668151267913 ),
 .UNSPECIFIED. ) ;
#26986 = DIRECTION ( 'NONE',  ( 0.000000000000000000, 5.223019709707975211E-21, -1.000000000000000000 ) ) ;
#26987 = EDGE_CURVE ( 'NONE', #4463, #21774, #7684, .T. ) ;
#26988 = ORIENTED_EDGE ( 'NONE', *, *, #17095, .F. ) ;
#26989 = B_SPLINE_CURVE_WITH_KNOTS ( 'NONE', 3,
 ( #16601, #9993, #14277, #5368 ),
 .UNSPECIFIED., .F., .F.,
 ( 4, 4 ),
 ( 0.000000000000000000, 0.008383560773332717278 ),
 .UNSPECIFIED. ) ;
#26990 = B_SPLINE_CURVE_WITH_KNOTS ( 'NONE', 3,
 ( #28014, #1957, #19379, #8182, #8314, #28154, #8457 ),
 .UNSPECIFIED., .F., .F.,
 ( 4, 3, 4 ),
 ( 7.341549781884751001E-16, 0.02816610861753246139, 0.04000277880656284007 ),
 .UNSPECIFIED. ) ;
#26991 = FACE_OUTER_BOUND ( 'NONE', #24643, .T. ) ;
#26992 = EDGE_CURVE ( 'NONE', #6704, #14115, #10309, .T. ) ;
#26993 = CARTESIAN_POINT ( 'NONE',  ( 19.66333377628711077, 9.924285918886457836, 137.3914191246404357 ) ) ;
#26994 = FACE_OUTER_BOUND ( 'NONE', #5746, .T. ) ;
#26995 = VERTEX_POINT ( 'NONE', #1636 ) ;
#26996 = CARTESIAN_POINT ( 'NONE',  ( 5.340103579038215642, -71.72120379026111436, 128.8311297206839470 ) ) ;
#26997 = ORIENTED_EDGE ( 'NONE', *, *, #10680, .T. ) ;
#26998 = DIRECTION ( 'NONE',  ( 0.000000000000000000, 0.000000000000000000, 1.000000000000000000 ) ) ;
#26999 = CARTESIAN_POINT ( 'NONE',  ( 16.05277956358197144, -109.5668455727254695, -92.36732600443316699 ) ) ;
#27000 = CARTESIAN_POINT ( 'NONE',  ( 25.64692232868533139, 107.2834780834840274, -35.20209749635197483 ) ) ;
#27001 = CARTESIAN_POINT ( 'NONE',  ( 25.81918753295377655, -113.0221398901143033, 0.9336804662323209270 ) ) ;
#27002 = EDGE_LOOP ( 'NONE', ( #10572, #19244, #26474, #9856 ) ) ;
#27003 = CARTESIAN_POINT ( 'NONE',  ( 25.64707127832796019, 0.04959866882966159490, 112.9112343549835487 ) ) ;
#27004 = CARTESIAN_POINT ( 'NONE',  ( -7.762687761849950397E-17, 3.022826910523253725E-17, 44.74884827092600403 ) ) ;
#27005 = DIRECTION ( 'NONE',  ( 0.7637818620346801257, 0.5345501402766276167, -0.3617919495470772184 ) ) ;
#27006 = ORIENTED_EDGE ( 'NONE', *, *, #11400, .T. ) ;
#27007 = ORIENTED_EDGE ( 'NONE', *, *, #28290, .F. ) ;
#27008 = VERTEX_POINT ( 'NONE', #10435 ) ;
#27009 = CARTESIAN_POINT ( 'NONE',  ( 25.70243777736192570, -90.94412140945908618, -66.98101477609100129 ) ) ;
#27010 = CARTESIAN_POINT ( 'NONE',  ( -1.583189561560255143, 46.33203782964461936, 2.490696082060026573 ) ) ;
#27011 = CARTESIAN_POINT ( 'NONE',  ( -20.57838717382308147, -1.611677988432568709, -29.92853265176830746 ) ) ;
#27012 = CARTESIAN_POINT ( 'NONE',  ( -8.786685647604887350, 53.04920435127183254, 7.199674155859139724 ) ) ;
#27013 = CARTESIAN_POINT ( 'NONE',  ( 25.64708228042119131, -83.93578330383134301, 75.52311986517997866 ) ) ;
#27014 = CARTESIAN_POINT ( 'NONE',  ( 25.64703792032472762, 45.78915563622703644, -103.2099561461819661 ) ) ;
#27015 = ORIENTED_EDGE ( 'NONE', *, *, #18346, .F. ) ;
#27016 = DIRECTION ( 'NONE',  ( 1.000000000000000000, -6.938893903907226837E-18, 1.734723475976806709E-18 ) ) ;
#27017 = CARTESIAN_POINT ( 'NONE',  ( -2.265401668238146371, -29.73100299756539755, 36.42007794497283157 ) ) ;
#27018 = AXIS2_PLACEMENT_3D ( 'NONE', #24897, #11641, #3293 ) ;
#27019 = CARTESIAN_POINT ( 'NONE',  ( 1.833721034905635872, -145.1093571238132540, 0.3559403234832136942 ) ) ;
#27020 = CARTESIAN_POINT ( 'NONE',  ( -15.02187109954783928, 20.12219089991090115, -41.75590530176315696 ) ) ;
#27021 = CARTESIAN_POINT ( 'NONE',  ( 1.834118845439484335, -72.40084790867418008, 125.7578880615042749 ) ) ;
#27022 = CARTESIAN_POINT ( 'NONE',  ( 8.186469829614386740, -27.65107825763847416, -146.7694295239428186 ) ) ;
#27023 = EDGE_CURVE ( 'NONE', #25151, #26744, #23839, .T. ) ;
#27024 = ORIENTED_EDGE ( 'NONE', *, *, #23079, .F. ) ;
#27025 = DIRECTION ( 'NONE',  ( 0.5914120900931444380, 0.8010740644654229525, 0.09226095020378749512 ) ) ;
#27026 = CARTESIAN_POINT ( 'NONE',  ( -22.23342874802668234, 7.677086057585391643, 30.68433055777672180 ) ) ;
#27027 = EDGE_CURVE ( 'NONE', #11830, #11861, #22676, .T. ) ;
#27028 = CARTESIAN_POINT ( 'NONE',  ( -9.156249394959713683, 53.74753343182715781, 9.022661520477214481 ) ) ;
#27029 = EDGE_LOOP ( 'NONE', ( #27344, #20920, #15346, #24593 ) ) ;
#27030 = ADVANCED_FACE ( 'NONE', ( #28381 ), #25563, .F. ) ;
#27031 = ORIENTED_EDGE ( 'NONE', *, *, #5803, .F. ) ;
#27032 = ORIENTED_EDGE ( 'NONE', *, *, #2319, .T. ) ;
#27033 = VECTOR ( 'NONE', #16336, 1000.000000000000114 ) ;
#27034 = CARTESIAN_POINT ( 'NONE',  ( 109.1778270068192853, -0.0006237116683870695330, 0.009293669915260193218 ) ) ;
#27035 = CARTESIAN_POINT ( 'NONE',  ( 10.93730112725932635, 0.000000000000000000, 0.000000000000000000 ) ) ;
#27036 = CARTESIAN_POINT ( 'NONE',  ( 13.84597867724968268, -82.31427113894703496, -121.4327876424623440 ) ) ;
#27037 = CARTESIAN_POINT ( 'NONE',  ( 26.11404676487259024, 97.48350837663691948, -57.58742681967348176 ) ) ;
#27038 = ORIENTED_EDGE ( 'NONE', *, *, #3216, .F. ) ;
#27039 = CARTESIAN_POINT ( 'NONE',  ( -25.21435515916042647, 15.02493970636146692, -31.17620025257592786 ) ) ;
#27040 = CARTESIAN_POINT ( 'NONE',  ( 25.69398547355839213, 45.25878216557570966, -103.4778695380284148 ) ) ;
#27041 = EDGE_CURVE ( 'NONE', #6478, #10003, #13560, .T. ) ;
#27042 = CARTESIAN_POINT ( 'NONE',  ( -1.058197053496169548, -45.77356582045592859, -1.754224732379389362 ) ) ;
#27043 = ORIENTED_EDGE ( 'NONE', *, *, #3123, .F. ) ;
#27044 = ORIENTED_EDGE ( 'NONE', *, *, #20876, .F. ) ;
#27045 = CARTESIAN_POINT ( 'NONE',  ( -12.94347594948481195, -43.91326021875530472, -21.16159467081338263 ) ) ;
#27046 = CARTESIAN_POINT ( 'NONE',  ( -25.21435515916044423, -16.39063784838720395, 30.48034229288656505 ) ) ;
#27047 = CARTESIAN_POINT ( 'NONE',  ( -4.162674018437141576, 48.79210541969627712, 3.424137510345119484 ) ) ;
#27048 = CARTESIAN_POINT ( 'NONE',  ( -55.25297051322618813, -0.01306918787467559705, 0.007247191603131494450 ) ) ;
#27049 = CARTESIAN_POINT ( 'NONE',  ( 109.1587776205901861, 0.006729130500864210183, 0.002904816147411993371 ) ) ;
#27050 =( BOUNDED_SURFACE ( )  B_SPLINE_SURFACE ( 3, 1, ( 
 ( #27236, #25102 ),
 ( #5367, #10418 ),
 ( #3924, #6367 ),
 ( #8396, #15118 ) ),
 .UNSPECIFIED., .F., .F., .F. ) 
 B_SPLINE_SURFACE_WITH_KNOTS ( ( 4, 4 ),
 ( 2, 2 ),
 ( 0.000000000000000000, 1.000000000000000000 ),
 ( 0.000000000000000000, 1.000000000000000000 ),
 .UNSPECIFIED. ) 
 GEOMETRIC_REPRESENTATION_ITEM ( )  RATIONAL_B_SPLINE_SURFACE ( (
 ( 1.000000000000000000, 1.000000000000000000),
 ( 0.6386103224230316178, 0.9954351624131538845),
 ( 0.6386103224230316178, 0.9954351624131538845),
 ( 1.000000000000000000, 1.000000000000000000) ) ) 
 REPRESENTATION_ITEM ( '' )  SURFACE ( )  );
#27051 = ADVANCED_FACE ( 'NONE', ( #17443 ), #2393, .T. ) ;
#27052 = CARTESIAN_POINT ( 'NONE',  ( 2.433796855181219243, -125.2830755159749003, -74.00833731765692391 ) ) ;
#27053 = CARTESIAN_POINT ( 'NONE',  ( 109.1721716018069515, -0.01673651515802106193, 0.003350975118860912826 ) ) ;
#27054 = ORIENTED_EDGE ( 'NONE', *, *, #25078, .F. ) ;
#27055 = CARTESIAN_POINT ( 'NONE',  ( 10.93730112725999248, 42.00474393596446987, -145.2260730187398110 ) ) ;
#27056 = CARTESIAN_POINT ( 'NONE',  ( 2.263178113027036531, 16.59120315151768921, -144.4462808674008443 ) ) ;
#27057 = B_SPLINE_CURVE_WITH_KNOTS ( 'NONE', 3,
 ( #19575, #28340, #26193, #6489, #3609, #12387 ),
 .UNSPECIFIED., .F., .F.,
 ( 4, 2, 4 ),
 ( 2.084489702152424451E-17, 0.0006311571484585999344, 0.001262314296917178835 ),
 .UNSPECIFIED. ) ;
#27058 = ADVANCED_FACE ( 'NONE', ( #13135 ), #23544, .F. ) ;
#27059 = CARTESIAN_POINT ( 'NONE',  ( -1.044557008772706297, 44.03203053429572833, -12.57891310333364210 ) ) ;
#27060 = CARTESIAN_POINT ( 'NONE',  ( 28.37603512858443366, -45.02094145483448528, 105.5302493666425505 ) ) ;
#27061 = EDGE_CURVE ( 'NONE', #13776, #14553, #12802, .T. ) ;
#27062 = CARTESIAN_POINT ( 'NONE',  ( -23.79248802219722947, 3.207402715357613676, 33.03370827286725842 ) ) ;
#27063 = EDGE_LOOP ( 'NONE', ( #18148, #2640, #17812, #10540 ) ) ;
#27064 = VERTEX_POINT ( 'NONE', #19749 ) ;
#27065 = CARTESIAN_POINT ( 'NONE',  ( 1.833750490713715209, 145.1094586213657749, 0.2669522761650450771 ) ) ;
#27066 = ORIENTED_EDGE ( 'NONE', *, *, #4748, .F. ) ;
#27067 = EDGE_LOOP ( 'NONE', ( #14694, #13615, #25129, #11445 ) ) ;
#27068 = VERTEX_POINT ( 'NONE', #6678 ) ;
#27069 = CARTESIAN_POINT ( 'NONE',  ( -1.045287976400362417, -1.530335034933495653, 45.76855895860946788 ) ) ;
#27070 = CARTESIAN_POINT ( 'NONE',  ( 2.433796855181233454, 31.67151202412969724, 142.0211193075556935 ) ) ;
#27071 = CARTESIAN_POINT ( 'NONE',  ( -21.81686047589424859, -38.17230180719262478, -5.181745222995322919 ) ) ;
#27072 = CARTESIAN_POINT ( 'NONE',  ( 1.894214914920967274, -126.1778046718831376, -71.74757687370589565 ) ) ;
#27073 = CARTESIAN_POINT ( 'NONE',  ( -1.539760825549686185, 2.469813586483733392, 46.22267384399377477 ) ) ;
#27074 = CARTESIAN_POINT ( 'NONE',  ( 26.11404676487257603, -74.91683232331033082, 84.89295829319468112 ) ) ;
#27075 = DIRECTION ( 'NONE',  ( -0.5914120900931443270, 0.3962188444547338761, -0.7023121577978085339 ) ) ;
#27076 = CARTESIAN_POINT ( 'NONE',  ( 13.36082413113061307, 9.660980093454693218, 152.6206443696329131 ) ) ;
#27077 = DIRECTION ( 'NONE',  ( -1.000000000000000000, 6.938893903907227607E-18, -1.734723475976806902E-18 ) ) ;
#27078 = EDGE_CURVE ( 'NONE', #13021, #24113, #5637, .T. ) ;
#27079 = CARTESIAN_POINT ( 'NONE',  ( -23.77929240705206482, 17.17389748746964173, -31.93650644494346835 ) ) ;
#27080 = CARTESIAN_POINT ( 'NONE',  ( -12.94347594948485103, 23.08810053288751263, 42.93165645342833869 ) ) ;
#27081 = CARTESIAN_POINT ( 'NONE',  ( 10.93730112725990367, -133.3192575531795399, -71.28103789255078482 ) ) ;
#27082 =( BOUNDED_SURFACE ( )  B_SPLINE_SURFACE ( 3, 1, ( 
 ( #28414, #8714 ),
 ( #26268, #21390 ),
 ( #19784, #6566 ),
 ( #8443, #19640 ) ),
 .UNSPECIFIED., .F., .F., .F. ) 
 B_SPLINE_SURFACE_WITH_KNOTS ( ( 4, 4 ),
 ( 2, 2 ),
 ( 0.000000000000000000, 1.000000000000000000 ),
 ( 0.000000000000000000, 1.000000000000000000 ),
 .UNSPECIFIED. ) 
 GEOMETRIC_REPRESENTATION_ITEM ( )  RATIONAL_B_SPLINE_SURFACE ( (
 ( 1.000000000000000000, 1.000000000000000000),
 ( 0.6386103224230302855, 0.9954351624131538845),
 ( 0.6386103224230302855, 0.9954351624131538845),
 ( 1.000000000000000000, 1.000000000000000000) ) ) 
 REPRESENTATION_ITEM ( '' )  SURFACE ( )  );
#27083 = ADVANCED_FACE ( 'NONE', ( #26514 ), #9326, .T. ) ;
#27084 = CARTESIAN_POINT ( 'NONE',  ( 109.1624594426973260, 0.01570508117119674002, -0.002863932759303885849 ) ) ;
#27085 = EDGE_CURVE ( 'NONE', #11589, #12174, #1145, .T. ) ;
#27086 = CARTESIAN_POINT ( 'NONE',  ( 25.87036335909426654, 76.38467849957150690, 83.35447252092892256 ) ) ;
#27087 = CARTESIAN_POINT ( 'NONE',  ( -1.048171036023494596, -37.64178826568587510, 26.08692787913908617 ) ) ;
#27088 = CARTESIAN_POINT ( 'NONE',  ( -20.57838717382308147, 29.92853265176831812, 1.611677988432465014 ) ) ;
#27089 = CARTESIAN_POINT ( 'NONE',  ( 25.64703792032472052, 83.80974623566390846, -75.66285916808213585 ) ) ;
#27090 = VERTEX_POINT ( 'NONE', #22658 ) ;
#27091 = CARTESIAN_POINT ( 'NONE',  ( -1.583189561560255143, 16.68617981233701997, -43.29471907393748609 ) ) ;
#27092 = VERTEX_POINT ( 'NONE', #3738 ) ;
#27093 = CARTESIAN_POINT ( 'NONE',  ( 109.1589550718175161, -0.006669585340474292433, -0.003591809816099503141 ) ) ;
#27094 = DIRECTION ( 'NONE',  ( -0.5914120900931443270, -0.3352908775637108985, -0.7333565075147389090 ) ) ;
#27095 = B_SPLINE_CURVE_WITH_KNOTS ( 'NONE', 3,
 ( #13528, #19002, #5913, #10087, #25498, #8204, #16706, #10240, #23198, #23336 ),
 .UNSPECIFIED., .F., .F.,
 ( 4, 3, 3, 4 ),
 ( 3.469446951953614189E-17, 0.0002669559177086070585, 0.0005339118354150947186, 0.001067817517169157744 ),
 .UNSPECIFIED. ) ;
#27096 = EDGE_LOOP ( 'NONE', ( #3553, #5009, #26402, #2292 ) ) ;
#27097 = ORIENTED_EDGE ( 'NONE', *, *, #2391, .T. ) ;
#27098 = B_SPLINE_CURVE_WITH_KNOTS ( 'NONE', 3,
 ( #27389, #9997, #25545, #7995, #23104, #5517, #3364, #18759, #7702, #12149 ),
 .UNSPECIFIED., .F., .F.,
 ( 4, 2, 2, 2, 4 ),
 ( 2.602085213965210642E-18, 0.0003346267210630942475, 0.0006692534421261858929, 0.001003880163189277593, 0.001338506884252369184 ),
 .UNSPECIFIED. ) ;
#27099 = VERTEX_POINT ( 'NONE', #11842 ) ;
#27100 = CARTESIAN_POINT ( 'NONE',  ( 109.1589550718175161, 0.0002241941239325955654, 0.007571935245608775629 ) ) ;
#27101 = LINE ( 'NONE', #22826, #9697 ) ;
#27102 = B_SPLINE_CURVE_WITH_KNOTS ( 'NONE', 3,
 ( #175, #7098, #6664, #4920, #20, #26362 ),
 .UNSPECIFIED., .F., .F.,
 ( 4, 2, 4 ),
 ( 4.336808689942017736E-18, 0.0006311636237756799951, 0.001262327247551355003 ),
 .UNSPECIFIED. ) ;
#27103 = CARTESIAN_POINT ( 'NONE',  ( -4.473127245936431073, 26.34600523034598396, 41.70021447285024863 ) ) ;
#27104 = CARTESIAN_POINT ( 'NONE',  ( 1.833838848569428581, 144.2962335061013448, -15.34509722932385145 ) ) ;
#27105 = CARTESIAN_POINT ( 'NONE',  ( -55.25297051322618813, -0.007247191603131164853, -0.01306918787467609838 ) ) ;
#27106 = EDGE_CURVE ( 'NONE', #2997, #5380, #7251, .T. ) ;
#27107 = FACE_OUTER_BOUND ( 'NONE', #10080, .T. ) ;
#27108 = MECHANICAL_DESIGN_GEOMETRIC_PRESENTATION_REPRESENTATION (  '', ( #10212 ), #72 ) ;
#27109 = CARTESIAN_POINT ( 'NONE',  ( 1.833838848569439683, -72.70900949568685689, -125.5797553397076882 ) ) ;
#27110 = CARTESIAN_POINT ( 'NONE',  ( -55.24271866751342941, 0.001545935011627245191, 0.009369360294294363373 ) ) ;
#27111 = CARTESIAN_POINT ( 'NONE',  ( 109.1778270068192853, 0.009293669915253098199, -0.0006237116683806388047 ) ) ;
#27112 = AXIS2_PLACEMENT_3D ( 'NONE', #15203, #24023, #2106 ) ;
#27113 = B_SPLINE_CURVE_WITH_KNOTS ( 'NONE', 3,
 ( #14637, #3849, #12614, #15327, #28424, #17494, #19792, #10608, #6296, #28151 ),
 .UNSPECIFIED., .F., .F.,
 ( 4, 3, 3, 4 ),
 ( 1.387778780781445676E-17, 0.0002669560319015652078, 0.0005492286108966281180, 0.0008315040496093381757 ),
 .UNSPECIFIED. ) ;
#27114 = CARTESIAN_POINT ( 'NONE',  ( 1.832998868059890096, 59.50898020732510929, 132.3466930259795618 ) ) ;
#27115 = CARTESIAN_POINT ( 'NONE',  ( 109.1586900883932856, 0.007002774699553659596, -0.001385221016536874366 ) ) ;
#27116 = CARTESIAN_POINT ( 'NONE',  ( 19.66333377628701484, -95.46107873288957535, 99.30798531455323541 ) ) ;
#27117 = EDGE_CURVE ( 'NONE', #8996, #4319, #3590, .T. ) ;
#27118 = EDGE_LOOP ( 'NONE', ( #8907, #19816, #12933, #8418 ) ) ;
#27119 = VERTEX_POINT ( 'NONE', #24814 ) ;
#27120 = CARTESIAN_POINT ( 'NONE',  ( -55.24198130335446422, -0.008252882783649790471, 0.004276389980776089048 ) ) ;
#27122 = CARTESIAN_POINT ( 'NONE',  ( -23.79248802219724368, 7.157555990716900851, -32.40806545715334153 ) ) ;
#27121 = CARTESIAN_POINT ( 'NONE',  ( -1.031422197589711764, -36.13727897780146492, -28.14735071801730726 ) ) ;
#27123 = CARTESIAN_POINT ( 'NONE',  ( -20.20700224038492365, -8.199606986804534259, -28.44216453106533748 ) ) ;
#27124 = CARTESIAN_POINT ( 'NONE',  ( 19.66333377628716406, 33.01772659807287624, -133.7337774474995058 ) ) ;
#27125 = DIRECTION ( 'NONE',  ( -0.000000000000000000, -0.000000000000000000, 1.000000000000000000 ) ) ;
#27126 = ORIENTED_EDGE ( 'NONE', *, *, #25692, .F. ) ;
#27127 = EDGE_CURVE ( 'NONE', #20942, #16924, #3224, .T. ) ;
#27128 = ORIENTED_EDGE ( 'NONE', *, *, #26374, .T. ) ;
#27129 = CARTESIAN_POINT ( 'NONE',  ( -23.79223135445718995, -32.40779366744830270, 7.157574570129486169 ) ) ;
#27130 = CARTESIAN_POINT ( 'NONE',  ( 109.1586900883932856, 0.006757191295056129768, -0.002301750759607921679 ) ) ;
#27131 = CARTESIAN_POINT ( 'NONE',  ( -1.045287976400379737, -37.92705037016725100, 25.66401692420055269 ) ) ;
#27132 = ORIENTED_EDGE ( 'NONE', *, *, #17764, .T. ) ;
#27133 = CARTESIAN_POINT ( 'NONE',  ( 109.1721716018069657, -0.005466227998629111413, -0.01616973485710948913 ) ) ;
#27134 = ORIENTED_EDGE ( 'NONE', *, *, #17635, .F. ) ;
#27135 = CARTESIAN_POINT ( 'NONE',  ( -1.155031165708878094, -16.13806347973029176, -42.97366960678595404 ) ) ;
#27136 =( BOUNDED_SURFACE ( )  B_SPLINE_SURFACE ( 3, 1, ( 
 ( #16582, #25665 ),
 ( #23366, #5942 ),
 ( #14697, #23505 ),
 ( #10949, #8943 ) ),
 .UNSPECIFIED., .F., .F., .F. ) 
 B_SPLINE_SURFACE_WITH_KNOTS ( ( 4, 4 ),
 ( 2, 2 ),
 ( 0.000000000000000000, 1.000000000000000000 ),
 ( 0.000000000000000000, 1.000000000000000000 ),
 .UNSPECIFIED. ) 
 GEOMETRIC_REPRESENTATION_ITEM ( )  RATIONAL_B_SPLINE_SURFACE ( (
 ( 1.000000000000000000, 1.000000000000000000),
 ( 0.7789835883360578528, 0.9689951854195403280),
 ( 0.7789835883360578528, 0.9689951854195403280),
 ( 1.000000000000000000, 1.000000000000000000) ) ) 
 REPRESENTATION_ITEM ( '' )  SURFACE ( )  );
#27137 = VECTOR ( 'NONE', #11241, 1000.000000000000227 ) ;
#27138 = CARTESIAN_POINT ( 'NONE',  ( -7.078251931573400491, -34.59014398252887190, 38.93060825814266934 ) ) ;
#27139 = VECTOR ( 'NONE', #11505, 999.9999999999998863 ) ;
#27140 = EDGE_LOOP ( 'NONE', ( #8701, #23627, #15012, #16517 ) ) ;
#27141 = CARTESIAN_POINT ( 'NONE',  ( -55.25297051322618813, -0.01306918787467238607, -0.007247191603129069307 ) ) ;
#27142 = CIRCLE ( 'NONE', #15169, 20.00000000000000000 ) ;
#27143 = VERTEX_POINT ( 'NONE', #9541 ) ;
#27144 = CARTESIAN_POINT ( 'NONE',  ( -22.23226125620944771, -16.78323347921898900, 26.80886670319655707 ) ) ;
#27145 = VERTEX_POINT ( 'NONE', #27911 ) ;
#27146 = CARTESIAN_POINT ( 'NONE',  ( -8.786685647604885574, 6.096987947571466530E-17, -1.524246986892866633E-17 ) ) ;
#27147 = EDGE_CURVE ( 'NONE', #10856, #11536, #21283, .T. ) ;
#27148 = CARTESIAN_POINT ( 'NONE',  ( 109.1586059443104944, -0.005438258427225644252, 0.004524147648833148731 ) ) ;
#27149 = CARTESIAN_POINT ( 'NONE',  ( -15.02187109954782507, 8.264310930413024892, 45.60876405941875333 ) ) ;
#27150 = CARTESIAN_POINT ( 'NONE',  ( -24.53237795827023859, -3.868415699415882258, -33.71192251888856362 ) ) ;
#27151 = EDGE_CURVE ( 'NONE', #17620, #2385, #6647, .T. ) ;
#27152 = ORIENTED_EDGE ( 'NONE', *, *, #25998, .F. ) ;
#27153 = CARTESIAN_POINT ( 'NONE',  ( 13.84597867724965070, -64.00674338125939755, 132.0026437215599344 ) ) ;
#27154 = CARTESIAN_POINT ( 'NONE',  ( -1.045287976400351981, 43.05558670614237116, -15.59869763335110449 ) ) ;
#27155 = CARTESIAN_POINT ( 'NONE',  ( 109.1586059443104944, -0.007001002073869792321, 0.001014167950289951176 ) ) ;
#27156 = VERTEX_POINT ( 'NONE', #12507 ) ;
#27157 = EDGE_CURVE ( 'NONE', #27476, #22024, #23490, .T. ) ;
#27158 = ORIENTED_EDGE ( 'NONE', *, *, #25398, .T. ) ;
#27159 = VERTEX_POINT ( 'NONE', #3067 ) ;
#27160 = CARTESIAN_POINT ( 'NONE',  ( -55.25297051322618813, -0.006313402748432862636, 0.01354497706059893877 ) ) ;
#27161 = CARTESIAN_POINT ( 'NONE',  ( -25.21435515916025594, 1.749597353048488237E-16, -4.373993382621220594E-17 ) ) ;
#27163 = CARTESIAN_POINT ( 'NONE',  ( 1.831572820252008738, -141.7320553118904058, -31.13525033585638369 ) ) ;
#27162 = CARTESIAN_POINT ( 'NONE',  ( 1.833485406944043827, 108.1939177044938560, -96.69979900902059455 ) ) ;
#27164 = COLOUR_RGB ( '',0.7921568627450980005, 0.8196078431372548767, 0.9333333333333333481 ) ;
#27165 = FACE_OUTER_BOUND ( 'NONE', #6204, .T. ) ;
#27166 = CARTESIAN_POINT ( 'NONE',  ( -1.019300379054419725, -12.21833869579434761, 44.15350047934410327 ) ) ;
#27167 = CARTESIAN_POINT ( 'NONE',  ( 2.433796855181233454, 96.28145139437833677, -109.1007109081216129 ) ) ;
#27168 = DIRECTION ( 'NONE',  ( -1.000000000000000000, -0.000000000000000000, -0.000000000000000000 ) ) ;
#27169 = ORIENTED_EDGE ( 'NONE', *, *, #17569, .T. ) ;
#27170 = CARTESIAN_POINT ( 'NONE',  ( 1.831572820252009626, -142.1425225354578004, -29.20415387690713516 ) ) ;
#27171 = CARTESIAN_POINT ( 'NONE',  ( -6.588769196390751759, -34.04709086065287238, 38.42957692275880532 ) ) ;
#27172 = AXIS2_PLACEMENT_3D ( 'NONE', #11783, #14065, #25037 ) ;
#27173 = CARTESIAN_POINT ( 'NONE',  ( -20.38016308990357928, 28.74660391518355951, 7.753479680700641197 ) ) ;
#27174 = CARTESIAN_POINT ( 'NONE',  ( 109.1589550718175161, 0.0005685167901217448626, -0.007553890059316987690 ) ) ;
#27175 = CARTESIAN_POINT ( 'NONE',  ( -1.583189561560252701, 2.490696082059875138, -46.33203782964461936 ) ) ;
#27176 = ORIENTED_EDGE ( 'NONE', *, *, #25667, .T. ) ;
#27177 = CARTESIAN_POINT ( 'NONE',  ( 109.1586900883932856, 0.007088091345229654248, -0.0008465529156635364033 ) ) ;
#27178 = CARTESIAN_POINT ( 'NONE',  ( -20.57838717382308147, 16.28767523336157552, 25.16001208503087838 ) ) ;
#27179 = VERTEX_POINT ( 'NONE', #16709 ) ;
#27180 = ORIENTED_EDGE ( 'NONE', *, *, #2766, .T. ) ;
#27181 = CONICAL_SURFACE ( 'NONE', #18920, 117.6351876552689504, 0.9945805576725580410 ) ;
#27182 = CARTESIAN_POINT ( 'NONE',  ( 109.1778270068192853, 0.001322180554001401668, 0.009220257877180830508 ) ) ;
#27183 = CARTESIAN_POINT ( 'NONE',  ( 25.64708228042119131, -23.43704872438680553, -110.4520805602538047 ) ) ;
#27184 = CARTESIAN_POINT ( 'NONE',  ( 109.1592201516379674, -0.005027640251767255368, -0.006044422199822518590 ) ) ;
#27185 = VECTOR ( 'NONE', #12487, 1000.000000000000000 ) ;
#27186 = CARTESIAN_POINT ( 'NONE',  ( 1.894214914920957948, 58.16536411968120746, -132.9862534094750686 ) ) ;
#27187 = CARTESIAN_POINT ( 'NONE',  ( -6.588769196390770411, 50.13301368233300082, -11.07780292579711556 ) ) ;
#27188 = ORIENTED_EDGE ( 'NONE', *, *, #6380, .T. ) ;
#27189 = CARTESIAN_POINT ( 'NONE',  ( -55.24300891470650754, -0.0003472257464211635897, -0.009812809446892990090 ) ) ;
#27190 = EDGE_CURVE ( 'NONE', #4782, #16046, #28240, .T. ) ;
#27191 = CARTESIAN_POINT ( 'NONE',  ( 2.430230287190589422, -16.65331920325641235, -144.5585181921887568 ) ) ;
#27192 = CARTESIAN_POINT ( 'NONE',  ( 109.1592201516379674, 0.004368284148529012062, 0.006536841731953418715 ) ) ;
#27193 = ORIENTED_EDGE ( 'NONE', *, *, #27284, .F. ) ;
#27194 = EDGE_CURVE ( 'NONE', #24539, #28478, #589, .T. ) ;
#27195 = ORIENTED_EDGE ( 'NONE', *, *, #27395, .T. ) ;
#27196 = CARTESIAN_POINT ( 'NONE',  ( -1.619063947482197729, -35.99532424477357750, 29.22875152547795707 ) ) ;
#27197 = CARTESIAN_POINT ( 'NONE',  ( -1.050229599974473516, -37.20249516760156183, 26.71319688967675177 ) ) ;
#27198 = FACE_OUTER_BOUND ( 'NONE', #6174, .T. ) ;
#27199 = ADVANCED_FACE ( 'NONE', ( #9409 ), #1045, .T. ) ;
#27200 = LINE ( 'NONE', #25071, #12428 ) ;
#27201 = CARTESIAN_POINT ( 'NONE',  ( -2.904412668506661355, 36.79926976721492338, 30.27712468694946679 ) ) ;
#27202 = DIRECTION ( 'NONE',  ( 0.000000000000000000, 1.000000000000000000, 3.122502256758243698E-15 ) ) ;
#27203 = CARTESIAN_POINT ( 'NONE',  ( -1.048171036023517466, -45.78635789057865679, -1.020520027228972504 ) ) ;
#27204 = ORIENTED_EDGE ( 'NONE', *, *, #8972, .T. ) ;
#27205 = CARTESIAN_POINT ( 'NONE',  ( 25.73574536432413140, 84.49061642666573846, -74.99093179013885901 ) ) ;
#27206 = DIRECTION ( 'NONE',  ( 1.000000000000000000, -6.938893903907226837E-18, 1.734723475976806709E-18 ) ) ;
#27207 = VECTOR ( 'NONE', #11742, 1000.000000000000114 ) ;
#27208 = CARTESIAN_POINT ( 'NONE',  ( 25.64704443564077252, -107.4261196778965228, 34.76451658509497378 ) ) ;
#27209 = AXIS2_PLACEMENT_3D ( 'NONE', #7114, #17738, #4795 ) ;
#27210 = ORIENTED_EDGE ( 'NONE', *, *, #11966, .F. ) ;
#27211 = CARTESIAN_POINT ( 'NONE',  ( 25.64704443564079739, -75.65149037849816693, 83.82001435192599104 ) ) ;
#27212 = ORIENTED_EDGE ( 'NONE', *, *, #9371, .F. ) ;
#27213 = ORIENTED_EDGE ( 'NONE', *, *, #5493, .T. ) ;
#27214 = ORIENTED_EDGE ( 'NONE', *, *, #15791, .F. ) ;
#27215 =( BOUNDED_SURFACE ( )  B_SPLINE_SURFACE ( 3, 1, ( 
 ( #7858, #16036 ),
 ( #5101, #20500 ),
 ( #788, #25265 ),
 ( #12161, #20928 ) ),
 .UNSPECIFIED., .F., .F., .F. ) 
 B_SPLINE_SURFACE_WITH_KNOTS ( ( 4, 4 ),
 ( 2, 2 ),
 ( 0.000000000000000000, 1.000000000000000000 ),
 ( 0.000000000000000000, 1.000000000000000000 ),
 .UNSPECIFIED. ) 
 GEOMETRIC_REPRESENTATION_ITEM ( )  RATIONAL_B_SPLINE_SURFACE ( (
 ( 1.000000000000000000, 1.000000000000000000),
 ( 0.6386103224230316178, 0.9954351624131538845),
 ( 0.6386103224230316178, 0.9954351624131538845),
 ( 1.000000000000000000, 1.000000000000000000) ) ) 
 REPRESENTATION_ITEM ( '' )  SURFACE ( )  );
#27216 = CARTESIAN_POINT ( 'NONE',  ( 109.1587776205901577, -0.007186028091163443668, 0.001442274045003878562 ) ) ;
#27217 = FACE_OUTER_BOUND ( 'NONE', #5110, .T. ) ;
#27218 = B_SPLINE_CURVE_WITH_KNOTS ( 'NONE', 3,
 ( #21102, #3694, #27741, #25160 ),
 .UNSPECIFIED., .F., .F.,
 ( 4, 4 ),
 ( 0.000000000000000000, 0.008383560773332731156 ),
 .UNSPECIFIED. ) ;
#27219 = CARTESIAN_POINT ( 'NONE',  ( 109.1721716018069515, 0.01019541462303036154, -0.01368917435590592639 ) ) ;
#27220 = ADVANCED_FACE ( 'NONE', ( #19004 ), #3867, .F. ) ;
#27221 = B_SPLINE_CURVE_WITH_KNOTS ( 'NONE', 3,
 ( #4577, #4727, #22147, #13347, #13927, #26732 ),
 .UNSPECIFIED., .F., .F.,
 ( 4, 2, 4 ),
 ( 1.084202172485504434E-17, 0.0006311636237756648162, 0.001262327247551318574 ),
 .UNSPECIFIED. ) ;
#27222 = CARTESIAN_POINT ( 'NONE',  ( -2.265401668238147259, 25.45016726748371738, 39.53028715828205009 ) ) ;
#27224 =( BOUNDED_SURFACE ( )  B_SPLINE_SURFACE ( 3, 1, ( 
 ( #5167, #16103 ),
 ( #27473, #7785 ),
 ( #25186, #27327 ),
 ( #20709, #15963 ) ),
 .UNSPECIFIED., .F., .F., .F. ) 
 B_SPLINE_SURFACE_WITH_KNOTS ( ( 4, 4 ),
 ( 2, 2 ),
 ( 0.000000000000000000, 1.000000000000000000 ),
 ( 0.000000000000000000, 1.000000000000000000 ),
 .UNSPECIFIED. ) 
 GEOMETRIC_REPRESENTATION_ITEM ( )  RATIONAL_B_SPLINE_SURFACE ( (
 ( 1.000000000000000000, 1.000000000000000000),
 ( 0.9956975270656955868, 0.8568959468854907557),
 ( 0.9956975270656955868, 0.8568959468854907557),
 ( 1.000000000000000000, 1.000000000000000000) ) ) 
 REPRESENTATION_ITEM ( '' )  SURFACE ( )  );
#27223 = CONICAL_SURFACE ( 'NONE', #27714, 151.1787379149930359, 0.5880026024245678107 ) ;
#27225 = VECTOR ( 'NONE', #19552, 1000.000000000000114 ) ;
#27226 = CARTESIAN_POINT ( 'NONE',  ( 10.93730112725932635, 0.000000000000000000, 0.000000000000000000 ) ) ;
#27227 = EDGE_CURVE ( 'NONE', #4347, #1523, #7515, .T. ) ;
#27228 = DIRECTION ( 'NONE',  ( 0.7563875759206388771, -0.6531865459554681008, -0.03500244528122332249 ) ) ;
#27229 = CARTESIAN_POINT ( 'NONE',  ( 109.1587776205901577, -0.007328861771496576576, -8.330235397652469671E-05 ) ) ;
#27230 = CARTESIAN_POINT ( 'NONE',  ( 25.64681081121879203, 45.54494737132363724, -103.3177883989774841 ) ) ;
#27231 = CARTESIAN_POINT ( 'NONE',  ( 26.11404676487259024, -24.64483677384768967, -110.5078194225163912 ) ) ;
#27232 = CARTESIAN_POINT ( 'NONE',  ( -23.79223135445719350, -13.25822371132274924, 30.42557260166825017 ) ) ;
#27233 = CARTESIAN_POINT ( 'NONE',  ( -1.113427685306994652, -25.34053733836502431, 38.22586258295222450 ) ) ;
#27235 = CARTESIAN_POINT ( 'NONE',  ( 25.69398547355840279, -83.43419615433049330, 76.12333255527484255 ) ) ;
#27234 = FACE_OUTER_BOUND ( 'NONE', #456, .T. ) ;
#27236 = CARTESIAN_POINT ( 'NONE',  ( 109.1778270068192853, -0.005186985107080890889, -0.007736698406806078593 ) ) ;
#27237 = FACE_OUTER_BOUND ( 'NONE', #14971, .T. ) ;
#27238 = CARTESIAN_POINT ( 'NONE',  ( 32.73300124599738581, -28.19767303745521758, -114.2056417606550696 ) ) ;
#27239 = VERTEX_POINT ( 'NONE', #15077 ) ;
#27240 = CARTESIAN_POINT ( 'NONE',  ( -55.24340739397742794, 0.003826481709800397344, 0.009386184976285138343 ) ) ;
#27241 = ORIENTED_EDGE ( 'NONE', *, *, #28290, .T. ) ;
#27242 = CARTESIAN_POINT ( 'NONE',  ( 2.063896406836609909, 141.8093313989364788, -31.51663808384418530 ) ) ;
#27244 = VECTOR ( 'NONE', #14800, 1000.000000000000000 ) ;
#27243 = CARTESIAN_POINT ( 'NONE',  ( 9.884929003653608603, -65.04493172071570939, 135.7578851563883973 ) ) ;
#27245 = ORIENTED_EDGE ( 'NONE', *, *, #21152, .F. ) ;
#27246 = B_SPLINE_CURVE_WITH_KNOTS ( 'NONE', 3,
 ( #27709, #12853, #19075, #21228, #7872, #1506 ),
 .UNSPECIFIED., .F., .F.,
 ( 4, 2, 4 ),
 ( 7.806255641895631925E-18, 0.0006311636237756803203, 0.001262327247551352834 ),
 .UNSPECIFIED. ) ;
#27247 = AXIS2_PLACEMENT_3D ( 'NONE', #13075, #1990, #10789 ) ;
#27248 = ORIENTED_EDGE ( 'NONE', *, *, #26603, .T. ) ;
#27249 = ORIENTED_EDGE ( 'NONE', *, *, #2514, .T. ) ;
#27250 = ORIENTED_EDGE ( 'NONE', *, *, #23793, .T. ) ;
#27251 = DIRECTION ( 'NONE',  ( 1.000000000000000000, -6.938893903907226837E-18, 1.734723475976806709E-18 ) ) ;
#27252 = EDGE_CURVE ( 'NONE', #22237, #24705, #23609, .T. ) ;
#27253 = LINE ( 'NONE', #103, #25795 ) ;
#27254 = ADVANCED_FACE ( 'NONE', ( #2117 ), #22450, .F. ) ;
#27255 = CARTESIAN_POINT ( 'NONE',  ( 109.1592201516379674, -0.003476928926134757649, -0.007051465909552751508 ) ) ;
#27256 = EDGE_CURVE ( 'NONE', #11627, #1639, #21737, .T. ) ;
#27257 = CARTESIAN_POINT ( 'NONE',  ( -4.178947244162622532, 45.38689110596718734, -18.28784278438465805 ) ) ;
#27258 =( BOUNDED_SURFACE ( )  B_SPLINE_SURFACE ( 3, 1, ( 
 ( #26489, #13535 ),
 ( #15402, #10829 ),
 ( #19455, #8525 ),
 ( #19591, #6505 ) ),
 .UNSPECIFIED., .F., .F., .F. ) 
 B_SPLINE_SURFACE_WITH_KNOTS ( ( 4, 4 ),
 ( 2, 2 ),
 ( 0.000000000000000000, 1.000000000000000000 ),
 ( 0.000000000000000000, 1.000000000000000000 ),
 .UNSPECIFIED. ) 
 GEOMETRIC_REPRESENTATION_ITEM ( )  RATIONAL_B_SPLINE_SURFACE ( (
 ( 1.000000000000000000, 1.000000000000000000),
 ( 0.6386103224230302855, 0.9954351624131538845),
 ( 0.6386103224230302855, 0.9954351624131538845),
 ( 1.000000000000000000, 1.000000000000000000) ) ) 
 REPRESENTATION_ITEM ( '' )  SURFACE ( )  );
#27259 = CARTESIAN_POINT ( 'NONE',  ( -20.20700224038492721, 28.44216453106548315, 8.199606986804035103 ) ) ;
#27260 = CARTESIAN_POINT ( 'NONE',  ( 1.894214914920982151, 71.74757687370632198, -126.1778046718828534 ) ) ;
#27261 = CARTESIAN_POINT ( 'NONE',  ( 1.831572820252008738, 86.09108691067926600, -116.8148281295960516 ) ) ;
#27262 = CARTESIAN_POINT ( 'NONE',  ( 109.1589550718175161, 0.005233222325307164934, 0.005477029346534945282 ) ) ;
#27263 = AXIS2_PLACEMENT_3D ( 'NONE', #6878, #24598, #15623 ) ;
#27264 = CARTESIAN_POINT ( 'NONE',  ( -21.41430102051745266, 30.75470819672112199, -1.815007301162081088 ) ) ;
#27266 = DIRECTION ( 'NONE',  ( -0.5914120900931442160, 0.7333565075147400192, -0.3352908775637083449 ) ) ;
#27265 = CARTESIAN_POINT ( 'NONE',  ( -1.583189561560252701, -43.29471907393753582, -16.68617981233686365 ) ) ;
#27267 = DIRECTION ( 'NONE',  ( -0.7071067811865485719, 0.000000000000000000, -0.7071067811865465735 ) ) ;
#27268 = VECTOR ( 'NONE', #3850, 1000.000000000000114 ) ;
#27269 = ORIENTED_EDGE ( 'NONE', *, *, #7675, .T. ) ;
#27270 = EDGE_LOOP ( 'NONE', ( #885, #26675, #6549, #7885 ) ) ;
#27271 = CARTESIAN_POINT ( 'NONE',  ( -55.24198130335446422, -0.009190321388309828296, 0.001391250620101365347 ) ) ;
#27273 = CARTESIAN_POINT ( 'NONE',  ( 25.64700659047693776, -91.48068002582068914, 66.18331466615532577 ) ) ;
#27272 = CARTESIAN_POINT ( 'NONE',  ( 2.433796855181205476, 60.50726454508082952, -132.3327394885224919 ) ) ;
#27274 = CARTESIAN_POINT ( 'NONE',  ( 5.340103579038172121, -28.39990973304568911, 144.6887562507423297 ) ) ;
#27275 = CARTESIAN_POINT ( 'NONE',  ( -8.786685647604898008, 48.22796981442765940, -23.24040270374399952 ) ) ;
#27276 = LINE ( 'NONE', #7732, #18771 ) ;
#27277 = ORIENTED_EDGE ( 'NONE', *, *, #22943, .T. ) ;
#27278 = CARTESIAN_POINT ( 'NONE',  ( -20.90916690077959927, 28.59207721780146727, -27.35210456531384082 ) ) ;
#27279 = CARTESIAN_POINT ( 'NONE',  ( 1.833485406944057594, -0.5339064996874559599, -145.1085452359073429 ) ) ;
#27280 = CARTESIAN_POINT ( 'NONE',  ( 32.73300124599735028, 72.21147546950551543, 92.86301839380053025 ) ) ;
#27281 = CARTESIAN_POINT ( 'NONE',  ( -20.20700224038492010, 18.19058640100223556, -23.35150625415664649 ) ) ;
#27282 = B_SPLINE_CURVE_WITH_KNOTS ( 'NONE', 3,
 ( #2741, #18419, #5187, #13963, #11818, #867, #9654, #27197, #2593, #24349, #15683, #17842, #15979 ),
 .UNSPECIFIED., .F., .F.,
 ( 4, 3, 3, 3, 4 ),
 ( 1.551583845779545699E-17, 0.0007657099931970551407, 0.001531419946797920239, 0.002296279302920158170, 0.003061450627205758099 ),
 .UNSPECIFIED. ) ;
#27283 = CARTESIAN_POINT ( 'NONE',  ( 1.894214914920955728, 116.8658096527534411, -86.08679174687961222 ) ) ;
#27284 = EDGE_CURVE ( 'NONE', #21028, #7787, #20346, .T. ) ;
#27285 = ORIENTED_EDGE ( 'NONE', *, *, #9436, .T. ) ;
#27286 = CARTESIAN_POINT ( 'NONE',  ( -28.13707043255157103, -18.96624908365855688, -12.83104814250447134 ) ) ;
#27287 = ADVANCED_FACE ( 'NONE', ( #8757 ), #5897, .F. ) ;
#27288 = EDGE_CURVE ( 'NONE', #23571, #24705, #3899, .T. ) ;
#27289 = ORIENTED_EDGE ( 'NONE', *, *, #19249, .F. ) ;
#27290 = CARTESIAN_POINT ( 'NONE',  ( -20.20700224038492365, 8.199606986804329978, -28.44216453106539078 ) ) ;
#27291 = ORIENTED_EDGE ( 'NONE', *, *, #18829, .T. ) ;
#27292 = PRODUCT_CONTEXT ( 'NONE', #5692, 'mechanical' ) ;
#27293 = CARTESIAN_POINT ( 'NONE',  ( -1.464342487929844783, -44.64187261869788870, -11.94843286121900228 ) ) ;
#27294 = B_SPLINE_CURVE_WITH_KNOTS ( 'NONE', 3,
 ( #1998, #15086, #23906, #4436, #17535, #19839, #10657 ),
 .UNSPECIFIED., .F., .F.,
 ( 4, 3, 4 ),
 ( 9.299800619644450092E-17, 0.009512539173626386249, 0.02506242213020836232 ),
 .UNSPECIFIED. ) ;
#27295 = CARTESIAN_POINT ( 'NONE',  ( -55.25719721206881729, 0.0006290797159235729736, 0.01115102788683339750 ) ) ;
#27296 = CARTESIAN_POINT ( 'NONE',  ( 119.2224693531408803, 70.00000000000004263, 39.99999999999999289 ) ) ;
#27297 = FACE_OUTER_BOUND ( 'NONE', #4188, .T. ) ;
#27298 = ORIENTED_EDGE ( 'NONE', *, *, #11998, .T. ) ;
#27299 = VECTOR ( 'NONE', #19217, 1000.000000000000114 ) ;
#27300 = CARTESIAN_POINT ( 'NONE',  ( 109.1721716018069657, 0.01665253177026229658, -0.003746085893652622081 ) ) ;
#27301 = CARTESIAN_POINT ( 'NONE',  ( -1.044556982611275053, -45.76404732357875815, 1.643392503293194862 ) ) ;
#27302 = CARTESIAN_POINT ( 'NONE',  ( 109.1586900883932856, -0.007137750914550312215, 0.0001010081143975802818 ) ) ;
#27303 = ORIENTED_EDGE ( 'NONE', *, *, #3714, .F. ) ;
#27304 = VERTEX_POINT ( 'NONE', #1842 ) ;
#27305 = ORIENTED_EDGE ( 'NONE', *, *, #24157, .T. ) ;
#27306 = CARTESIAN_POINT ( 'NONE',  ( -55.24390624410018802, 0.004572280736702236288, 0.009374879212970765180 ) ) ;
#27307 = CARTESIAN_POINT ( 'NONE',  ( 109.1586059443104944, 0.006856640434645982184, 0.001740416220250496498 ) ) ;
#27309 = CARTESIAN_POINT ( 'NONE',  ( 24.22246935314087324, -69.99999999999998579, 40.00000000000003553 ) ) ;
#27308 = CARTESIAN_POINT ( 'NONE',  ( 28.37644542392834524, 98.15613422114097375, 76.32685750075042108 ) ) ;
#27310 = CARTESIAN_POINT ( 'NONE',  ( 13.84597867724981946, 55.26821062125554107, 135.8932891738218132 ) ) ;
#27311 = CARTESIAN_POINT ( 'NONE',  ( 1.832998868059858122, -125.9352106559978921, -72.09222286251214484 ) ) ;
#27312 = CARTESIAN_POINT ( 'NONE',  ( -20.57838717382308147, -18.89542499756516847, -23.26537097894098594 ) ) ;
#27313 =( BOUNDED_SURFACE ( )  B_SPLINE_SURFACE ( 3, 1, ( 
 ( #14152, #2803 ),
 ( #22827, #24986 ),
 ( #23115, #1075 ),
 ( #13877, #27404 ) ),
 .UNSPECIFIED., .F., .F., .F. ) 
 B_SPLINE_SURFACE_WITH_KNOTS ( ( 4, 4 ),
 ( 2, 2 ),
 ( 0.000000000000000000, 1.000000000000000000 ),
 ( 0.000000000000000000, 1.000000000000000000 ),
 .UNSPECIFIED. ) 
 GEOMETRIC_REPRESENTATION_ITEM ( )  RATIONAL_B_SPLINE_SURFACE ( (
 ( 1.000000000000000000, 1.000000000000000000),
 ( 0.9956975270656955868, 0.8568959468854907557),
 ( 0.9956975270656955868, 0.8568959468854907557),
 ( 1.000000000000000000, 1.000000000000000000) ) ) 
 REPRESENTATION_ITEM ( '' )  SURFACE ( )  );
#27314 = CARTESIAN_POINT ( 'NONE',  ( 10.93730112725936721, 145.2260730187397542, 42.00474393596321931 ) ) ;
#27315 = ORIENTED_EDGE ( 'NONE', *, *, #16181, .F. ) ;
#27316 = CARTESIAN_POINT ( 'NONE',  ( 109.1778270068192853, 0.002278716897421752870, -0.009031542838317233382 ) ) ;
#27317 = CARTESIAN_POINT ( 'NONE',  ( -4.162674018437125589, -31.44946543094270197, 37.46098494546626512 ) ) ;
#27318 = CARTESIAN_POINT ( 'NONE',  ( 25.65782528836481902, 110.3293115225706629, 24.04194111108905574 ) ) ;
#27319 = CARTESIAN_POINT ( 'NONE',  ( 109.1592201516379674, -0.007566779963318568183, 0.002134489919774338555 ) ) ;
#27320 = CARTESIAN_POINT ( 'NONE',  ( -4.473127245936431073, 37.94261489385763753, 31.51789735524151226 ) ) ;
#27321 = CARTESIAN_POINT ( 'NONE',  ( -20.20612091757424267, 16.46550228026431384, 24.59769958242370436 ) ) ;
#27322 = LINE ( 'NONE', #10771, #1316 ) ;
#27323 = EDGE_LOOP ( 'NONE', ( #8398, #5918, #6222, #27862 ) ) ;
#27324 = CARTESIAN_POINT ( 'NONE',  ( 1.833206310202349698, 29.44113265021129067, -142.0914673790817346 ) ) ;
#27325 = EDGE_CURVE ( 'NONE', #21943, #17335, #26860, .T. ) ;
#27326 = CARTESIAN_POINT ( 'NONE',  ( 28.37644542392842695, -95.06674036596263022, 80.14194118792678978 ) ) ;
#27327 = CARTESIAN_POINT ( 'NONE',  ( 2.063896406836605024, -86.47093297169081438, 116.7302989755734330 ) ) ;
#27328 = EDGE_CURVE ( 'NONE', #11014, #12154, #11166, .T. ) ;
#27329 = B_SPLINE_CURVE_WITH_KNOTS ( 'NONE', 3,
 ( #17193, #25981, #3821, #4377, #6271, #19213, #17613, #13151 ),
 .UNSPECIFIED., .F., .F.,
 ( 4, 2, 2, 4 ),
 ( 0.000000000000000000, 0.002761524886576655416, 0.005523049773153310832, 0.01104609954630660432 ),
 .UNSPECIFIED. ) ;
#27330 = VERTEX_POINT ( 'NONE', #8909 ) ;
#27331 = EDGE_LOOP ( 'NONE', ( #23025, #26651, #17693, #14367 ) ) ;
#27332 = ADVANCED_FACE ( 'NONE', ( #19551 ), #26465, .F. ) ;
#27333 = CARTESIAN_POINT ( 'NONE',  ( -1.031422197589716205, 25.67058493451444079, -37.93675465142481329 ) ) ;
#27334 = CARTESIAN_POINT ( 'NONE',  ( -1.046935749539996685, -43.14401153755477480, -15.35946454248379034 ) ) ;
#27335 = ADVANCED_FACE ( 'NONE', ( #26583 ), #18392, .F. ) ;
#27336 = CARTESIAN_POINT ( 'NONE',  ( -1.045287976400362417, -15.59869763335038506, 43.05558670614261985 ) ) ;
#27337 = DIRECTION ( 'NONE',  ( -1.000000000000000000, -0.000000000000000000, -0.000000000000000000 ) ) ;
#27338 = CARTESIAN_POINT ( 'NONE',  ( 25.81918753295378721, 97.41320410180168210, -57.31966094783101795 ) ) ;
#27339 = ORIENTED_EDGE ( 'NONE', *, *, #8674, .F. ) ;
#27340 = CARTESIAN_POINT ( 'NONE',  ( 25.70243777736191149, 66.98101477609128551, -90.94412140945890144 ) ) ;
#27341 = CARTESIAN_POINT ( 'NONE',  ( 25.64700659047696973, -103.2418925369176605, 45.71714758798341904 ) ) ;
#27342 = VECTOR ( 'NONE', #12647, 999.9999999999998863 ) ;
#27343 = CARTESIAN_POINT ( 'NONE',  ( 1.832998868059858122, 72.09222286251258538, -125.9352106559976363 ) ) ;
#27344 = ORIENTED_EDGE ( 'NONE', *, *, #1689, .F. ) ;
#27345 = EDGE_LOOP ( 'NONE', ( #2697, #10315, #25034, #22349 ) ) ;
#27346 = CARTESIAN_POINT ( 'NONE',  ( 109.1592201516379674, 0.002913740842103182058, -0.007302213399787563404 ) ) ;
#27347 = CARTESIAN_POINT ( 'NONE',  ( -55.25297051322618813, 0.01093108995494865114, -0.01019003092403491552 ) ) ;
#27348 = CARTESIAN_POINT ( 'NONE',  ( 2.108985857320926804, 84.36123201973967412, -118.2933707022550323 ) ) ;
#27349 = CARTESIAN_POINT ( 'NONE',  ( -90.83090735639699176, 4.592425496802575156E-15, 37.50000000000001421 ) ) ;
#27350 = CARTESIAN_POINT ( 'NONE',  ( 109.1586900883932856, 0.004277182003220951316, -0.005715190711488736183 ) ) ;
#27351 = CARTESIAN_POINT ( 'NONE',  ( -1.045287976400365970, 1.530335034933814731, -45.76855895860946788 ) ) ;
#27352 = CARTESIAN_POINT ( 'NONE',  ( -1.050229599974462413, -45.79907399707869331, -0.2556477501657915541 ) ) ;
#27353 = EDGE_LOOP ( 'NONE', ( #4439, #20185, #936, #10263 ) ) ;
#27354 = FACE_OUTER_BOUND ( 'NONE', #10794, .T. ) ;
#27355 = CARTESIAN_POINT ( 'NONE',  ( 109.1592201516379674, 0.007620268632971107306, -0.001934867487021749589 ) ) ;
#27356 =( BOUNDED_SURFACE ( )  B_SPLINE_SURFACE ( 3, 1, ( 
 ( #9185, #17947 ),
 ( #7189, #4728 ),
 ( #2707, #13500 ),
 ( #2263, #11634 ) ),
 .UNSPECIFIED., .F., .F., .F. ) 
 B_SPLINE_SURFACE_WITH_KNOTS ( ( 4, 4 ),
 ( 2, 2 ),
 ( 0.000000000000000000, 1.000000000000000000 ),
 ( 0.000000000000000000, 1.000000000000000000 ),
 .UNSPECIFIED. ) 
 GEOMETRIC_REPRESENTATION_ITEM ( )  RATIONAL_B_SPLINE_SURFACE ( (
 ( 1.000000000000000000, 1.000000000000000000),
 ( 0.7789835883360576307, 0.9689951854195403280),
 ( 0.7789835883360576307, 0.9689951854195403280),
 ( 1.000000000000000000, 1.000000000000000000) ) ) 
 REPRESENTATION_ITEM ( '' )  SURFACE ( )  );
#27357 = CARTESIAN_POINT ( 'NONE',  ( -1.155001620486248770, -25.28075036143248866, -38.31519699443491334 ) ) ;
#27358 = CARTESIAN_POINT ( 'NONE',  ( 25.64670758986459731, -75.92149922855251987, 83.57526425215473864 ) ) ;
#27359 = CARTESIAN_POINT ( 'NONE',  ( 25.64706233108857347, 0.08898442854020095771, -112.9112020921832453 ) ) ;
#27360 = ORIENTED_EDGE ( 'NONE', *, *, #23458, .T. ) ;
#27361 = CARTESIAN_POINT ( 'NONE',  ( -1.045287976400386842, -28.14015102489780062, 36.12803364096639314 ) ) ;
#27362 = B_SPLINE_CURVE_WITH_KNOTS ( 'NONE', 3,
 ( #16034, #9567, #9141, #24567, #5387, #20070, #6999, #15754 ),
 .UNSPECIFIED., .F., .F.,
 ( 4, 2, 2, 4 ),
 ( 0.000000000000000000, 0.002761524886576655416, 0.005523049773153310832, 0.01104609954630662166 ),
 .UNSPECIFIED. ) ;
#27363 = CARTESIAN_POINT ( 'NONE',  ( -28.41354790283022069, -8.345538364876929904, 21.64275480268756269 ) ) ;
#27364 = VERTEX_POINT ( 'NONE', #257 ) ;
#27365 = EDGE_CURVE ( 'NONE', #16671, #21028, #14549, .T. ) ;
#27366 = B_SPLINE_CURVE_WITH_KNOTS ( 'NONE', 3,
 ( #21199, #10289, #19046, #8122, #7550, #16307, #20577, #3030 ),
 .UNSPECIFIED., .F., .F.,
 ( 4, 2, 2, 4 ),
 ( 1.734723475976807094E-18, 0.0002429588503611230296, 0.0004859177007222443244, 0.0009718354014444825772 ),
 .UNSPECIFIED. ) ;
#27367 = B_SPLINE_CURVE_WITH_KNOTS ( 'NONE', 3,
 ( #21074, #20649, #12302, #25004 ),
 .UNSPECIFIED., .F., .F.,
 ( 4, 4 ),
 ( 2.754785121498913159E-16, 0.01077107486149849434 ),
 .UNSPECIFIED. ) ;
#27368 = ORIENTED_EDGE ( 'NONE', *, *, #25927, .T. ) ;
#27369 = ORIENTED_EDGE ( 'NONE', *, *, #24094, .T. ) ;
#27370 = ADVANCED_FACE ( 'NONE', ( #6887 ), #28138, .F. ) ;
#27371 = CARTESIAN_POINT ( 'NONE',  ( -7.078251931573400491, -26.33626633876254886, -44.92740138729156030 ) ) ;
#27372 = CARTESIAN_POINT ( 'NONE',  ( 10.93730112725932635, 0.000000000000000000, 0.000000000000000000 ) ) ;
#27373 = B_SPLINE_CURVE_WITH_KNOTS ( 'NONE', 3,
 ( #19662, #8322, #28023, #15191, #2098, #6586, #13050, #21835 ),
 .UNSPECIFIED., .F., .F.,
 ( 4, 2, 2, 4 ),
 ( 2.211348276820754320E-16, 0.002761568181852866368, 0.005523136363705511559, 0.01104627272741080107 ),
 .UNSPECIFIED. ) ;
#27374 = CARTESIAN_POINT ( 'NONE',  ( 109.1624594426973260, 0.01358749486988130618, 0.008380433676406104371 ) ) ;
#27375 = CARTESIAN_POINT ( 'NONE',  ( 1.834118845439484335, -107.7186227765447910, -97.22976650547533950 ) ) ;
#27376 = CARTESIAN_POINT ( 'NONE',  ( -20.20612091757422490, -28.48192249925583752, 8.058516044219494745 ) ) ;
#27377 = CARTESIAN_POINT ( 'NONE',  ( 25.98107933586720009, 107.9289867379274312, -33.92073193606466930 ) ) ;
#27378 = FACE_OUTER_BOUND ( 'NONE', #27765, .T. ) ;
#27379 = CARTESIAN_POINT ( 'NONE',  ( -28.13707043255157103, -0.7675454997505393173, 22.88591869784691468 ) ) ;
#27380 = CARTESIAN_POINT ( 'NONE',  ( -20.24419206586952313, -27.76448493191437095, 10.37009329716794248 ) ) ;
#27381 = LINE ( 'NONE', #7692, #13411 ) ;
#27382 = CARTESIAN_POINT ( 'NONE',  ( -1.619063947482197729, -25.20140673341345305, 38.92136151114934961 ) ) ;
#27383 = CARTESIAN_POINT ( 'NONE',  ( -20.57838717382308147, 29.92853265176831812, 1.611677988432465014 ) ) ;
#27384 = CARTESIAN_POINT ( 'NONE',  ( 25.64681081121880624, -23.06870491922396837, 110.5293738517607665 ) ) ;
#27385 = CARTESIAN_POINT ( 'NONE',  ( 9.884929003653608603, -149.2134106160914939, -19.90991253123399574 ) ) ;
#27386 = CARTESIAN_POINT ( 'NONE',  ( 28.37603512858451182, -58.91311972676474795, -98.45183098818044698 ) ) ;
#27387 = CARTESIAN_POINT ( 'NONE',  ( 1.894214914920950177, -107.2270864706596711, 97.83100278581372322 ) ) ;
#27388 = ORIENTED_EDGE ( 'NONE', *, *, #24439, .F. ) ;
#27389 = CARTESIAN_POINT ( 'NONE',  ( -1.619063947482194177, 25.20140673341374438, -38.92136151114915066 ) ) ;
#27390 = ORIENTED_EDGE ( 'NONE', *, *, #2906, .T. ) ;
#27391 = FACE_OUTER_BOUND ( 'NONE', #16629, .T. ) ;
#27392 =( BOUNDED_SURFACE ( )  B_SPLINE_SURFACE ( 3, 1, ( 
 ( #4078, #5977 ),
 ( #12848, #12712 ),
 ( #25698, #15138 ),
 ( #23964, #14734 ) ),
 .UNSPECIFIED., .F., .F., .F. ) 
 B_SPLINE_SURFACE_WITH_KNOTS ( ( 4, 4 ),
 ( 2, 2 ),
 ( 0.000000000000000000, 1.000000000000000000 ),
 ( 0.000000000000000000, 1.000000000000000000 ),
 .UNSPECIFIED. ) 
 GEOMETRIC_REPRESENTATION_ITEM ( )  RATIONAL_B_SPLINE_SURFACE ( (
 ( 1.000000000000000000, 1.000000000000000000),
 ( 0.9960225298536222738, 0.9999952330161893110),
 ( 0.9960225298536222738, 0.9999952330161893110),
 ( 1.000000000000000000, 1.000000000000000000) ) ) 
 REPRESENTATION_ITEM ( '' )  SURFACE ( )  );
#27393 = CARTESIAN_POINT ( 'NONE',  ( -1.045287976400362417, 25.66401692420069125, 37.92705037016716574 ) ) ;
#27394 = ORIENTED_EDGE ( 'NONE', *, *, #18156, .T. ) ;
#27395 = EDGE_CURVE ( 'NONE', #6221, #4343, #15170, .T. ) ;
#27396 = B_SPLINE_CURVE_WITH_KNOTS ( 'NONE', 3,
 ( #21573, #19415, #8486, #26039 ),
 .UNSPECIFIED., .F., .F.,
 ( 4, 4 ),
 ( 3.207224699059970292E-16, 0.01077107486149834342 ),
 .UNSPECIFIED. ) ;
#27397 = EDGE_LOOP ( 'NONE', ( #26760, #27038, #12417, #17612 ) ) ;
#27398 = ORIENTED_EDGE ( 'NONE', *, *, #385, .T. ) ;
#27399 = EDGE_CURVE ( 'NONE', #17616, #23498, #8039, .T. ) ;
#27400 = EDGE_CURVE ( 'NONE', #4630, #23252, #9032, .T. ) ;
#27401 =( BOUNDED_SURFACE ( )  B_SPLINE_SURFACE ( 3, 1, ( 
 ( #14930, #23750 ),
 ( #3996, #19394 ),
 ( #17235, #6311 ),
 ( #15059, #23884 ) ),
 .UNSPECIFIED., .F., .F., .F. ) 
 B_SPLINE_SURFACE_WITH_KNOTS ( ( 4, 4 ),
 ( 2, 2 ),
 ( 0.000000000000000000, 1.000000000000000000 ),
 ( 0.000000000000000000, 1.000000000000000000 ),
 .UNSPECIFIED. ) 
 GEOMETRIC_REPRESENTATION_ITEM ( )  RATIONAL_B_SPLINE_SURFACE ( (
 ( 1.000000000000000000, 1.000000000000000000),
 ( 0.9956975270656954757, 0.8568959468854893125),
 ( 0.9956975270656954757, 0.8568959468854893125),
 ( 1.000000000000000000, 1.000000000000000000) ) ) 
 REPRESENTATION_ITEM ( '' )  SURFACE ( )  );
#27402 = CARTESIAN_POINT ( 'NONE',  ( 55.49584447822657296, 29.26468316696772831, 66.38758986585125399 ) ) ;
#27403 = CARTESIAN_POINT ( 'NONE',  ( -22.23226125620944060, -26.80886670319648246, -16.78323347921907427 ) ) ;
#27404 = CARTESIAN_POINT ( 'NONE',  ( 2.430230287190581429, -84.35270093935177727, -118.5711603495689985 ) ) ;
#27405 = CARTESIAN_POINT ( 'NONE',  ( -55.24300891470648622, -0.006048736206180239418, 0.007734635432132643158 ) ) ;
#27406 = CARTESIAN_POINT ( 'NONE',  ( -28.13707043255157103, -14.07296284901319439, 18.06394523322468615 ) ) ;
#27407 = CARTESIAN_POINT ( 'NONE',  ( -1.056502255334264895, 27.33667001641221717, 36.75727364034702305 ) ) ;
#27408 = CARTESIAN_POINT ( 'NONE',  ( -1.113548883309550153, 28.52482525634944821, -35.91246368318211069 ) ) ;
#27409 = CARTESIAN_POINT ( 'NONE',  ( 6.224689322667647851, 100.9623537450651725, 108.2965163446077810 ) ) ;
#27410 = B_SPLINE_CURVE_WITH_KNOTS ( 'NONE', 3,
 ( #24321, #26885, #11350, #24181, #24619, #19842 ),
 .UNSPECIFIED., .F., .F.,
 ( 4, 2, 4 ),
 ( 5.135960789613967459E-18, 0.0004335151646191499485, 0.0008670303292382946928 ),
 .UNSPECIFIED. ) ;
#27411 = CARTESIAN_POINT ( 'NONE',  ( 2.430230287190572103, 142.0258656395021717, 31.67257033707552338 ) ) ;
#27412 = CARTESIAN_POINT ( 'NONE',  ( 2.263178113027036087, 57.85473702513869654, 133.3897502891096281 ) ) ;
#27413 = ORIENTED_EDGE ( 'NONE', *, *, #11379, .T. ) ;
#27414 = ORIENTED_EDGE ( 'NONE', *, *, #28360, .T. ) ;
#27415 = CARTESIAN_POINT ( 'NONE',  ( -1.048172774974295285, -26.08722459372758706, 37.64158596421241043 ) ) ;
#27417 = CARTESIAN_POINT ( 'NONE',  ( 25.73574536432418469, 57.18187897120932206, -97.42965068311163179 ) ) ;
#27416 = CARTESIAN_POINT ( 'NONE',  ( -55.24300891470648622, 0.009812809446890878931, 0.0003472257464245802360 ) ) ;
#27418 = CARTESIAN_POINT ( 'NONE',  ( -20.21097721712959938, -24.14932359587277233, 17.13687106192370280 ) ) ;
#27419 = CARTESIAN_POINT ( 'NONE',  ( -8.786685647604892679, -53.04920435127177569, 7.199674155859498548 ) ) ;
#27420 = ORIENTED_EDGE ( 'NONE', *, *, #1976, .F. ) ;
#27421 = EDGE_CURVE ( 'NONE', #22385, #8288, #14830, .T. ) ;
#27422 = ORIENTED_EDGE ( 'NONE', *, *, #22750, .T. ) ;
#27423 = CARTESIAN_POINT ( 'NONE',  ( 25.64704443564079739, 91.42548471394280796, -66.25951665433191806 ) ) ;
#27424 = CARTESIAN_POINT ( 'NONE',  ( 25.98552792386801613, -35.98568266743438926, -107.2612904323493410 ) ) ;
#27425 = LINE ( 'NONE', #12727, #1069 ) ;
#27426 = VERTEX_POINT ( 'NONE', #7040 ) ;
#27427 = B_SPLINE_CURVE_WITH_KNOTS ( 'NONE', 3,
 ( #16102, #3302, #2873, #20863 ),
 .UNSPECIFIED., .F., .F.,
 ( 4, 4 ),
 ( 6.938893903907228378E-18, 0.008383560773332719013 ),
 .UNSPECIFIED. ) ;
#27428 = EDGE_CURVE ( 'NONE', #24861, #9521, #20032, .T. ) ;
#27429 = CARTESIAN_POINT ( 'NONE',  ( 109.1589550718175161, 0.007553890059316984221, 0.0005685167901217716424 ) ) ;
#27430 = VERTEX_POINT ( 'NONE', #4995 ) ;
#27431 = VERTEX_POINT ( 'NONE', #13772 ) ;
#27432 = CARTESIAN_POINT ( 'NONE',  ( 1.834118845439484335, -44.67218053242300613, -138.0627591860434507 ) ) ;
#27433 =( BOUNDED_SURFACE ( )  B_SPLINE_SURFACE ( 3, 1, ( 
 ( #17127, #3897 ),
 ( #8502, #19155 ),
 ( #1592, #10256 ),
 ( #1723, #27926 ) ),
 .UNSPECIFIED., .F., .F., .F. ) 
 B_SPLINE_SURFACE_WITH_KNOTS ( ( 4, 4 ),
 ( 2, 2 ),
 ( 0.000000000000000000, 1.000000000000000000 ),
 ( 0.000000000000000000, 1.000000000000000000 ),
 .UNSPECIFIED. ) 
 GEOMETRIC_REPRESENTATION_ITEM ( )  RATIONAL_B_SPLINE_SURFACE ( (
 ( 1.000000000000000000, 1.000000000000000000),
 ( 0.9934239774497838349, 0.8357310067453913582),
 ( 0.9934239774497838349, 0.8357310067453913582),
 ( 1.000000000000000000, 1.000000000000000000) ) ) 
 REPRESENTATION_ITEM ( '' )  SURFACE ( )  );
#27434 = ORIENTED_EDGE ( 'NONE', *, *, #23918, .T. ) ;
#27435 = CARTESIAN_POINT ( 'NONE',  ( 25.64681081121879203, 112.3352186517030731, 11.38886654529711961 ) ) ;
#27436 = ORIENTED_EDGE ( 'NONE', *, *, #26987, .F. ) ;
#27437 = APPLICATION_PROTOCOL_DEFINITION ( 'draft international standard', 'automotive_design', 1998, #19299 ) ;
#27438 = ADVANCED_FACE ( 'NONE', ( #18672 ), #6639, .F. ) ;
#27439 = CARTESIAN_POINT ( 'NONE',  ( 30.59141879584323220, 114.2039975081485750, -21.51299111589929325 ) ) ;
#27440 = CARTESIAN_POINT ( 'NONE',  ( -1.619063947482201282, -16.67502769180592992, -43.26576862488428077 ) ) ;
#27441 = CARTESIAN_POINT ( 'NONE',  ( 26.11404676487257603, -47.08215554553588333, 102.9690087468800073 ) ) ;
#27442 = CARTESIAN_POINT ( 'NONE',  ( -28.13707043255157103, -14.07296284901345551, -18.06394523322448009 ) ) ;
#27443 = VERTEX_POINT ( 'NONE', #5286 ) ;
#27444 = CARTESIAN_POINT ( 'NONE',  ( -1.045287976400362417, -12.68782741917263657, 44.00138577190661948 ) ) ;
#27446 = FACE_OUTER_BOUND ( 'NONE', #16463, .T. ) ;
#27445 = CARTESIAN_POINT ( 'NONE',  ( 2.433796855181219243, 144.5536872373194228, -16.65276281464415575 ) ) ;
#27447 = CARTESIAN_POINT ( 'NONE',  ( -23.79223135445720771, 28.60983116549966354, -16.82181692922826599 ) ) ;
#27448 = ORIENTED_EDGE ( 'NONE', *, *, #19384, .F. ) ;
#27449 = ORIENTED_EDGE ( 'NONE', *, *, #13566, .T. ) ;
#27450 = VERTEX_POINT ( 'NONE', #971 ) ;
#27451 = CARTESIAN_POINT ( 'NONE',  ( -1.619063947482194177, -46.30105812165547974, 2.489035965910640247 ) ) ;
#27452 = DIRECTION ( 'NONE',  ( 0.000000000000000000, 5.223019709707975211E-21, -1.000000000000000000 ) ) ;
#27454 = CARTESIAN_POINT ( 'NONE',  ( -8.786685647604885574, 6.096987947571466530E-17, -1.524246986892866633E-17 ) ) ;
#27453 = CARTESIAN_POINT ( 'NONE',  ( -23.77929240705206482, -35.93174012244168836, 4.877832571065307654 ) ) ;
#27455 = DIRECTION ( 'NONE',  ( 0.000000000000000000, 5.223019709707975211E-21, -1.000000000000000000 ) ) ;
#27456 = DIRECTION ( 'NONE',  ( 0.000000000000000000, 5.223019709707975211E-21, -1.000000000000000000 ) ) ;
#27457 = ORIENTED_EDGE ( 'NONE', *, *, #5328, .F. ) ;
#27458 = CARTESIAN_POINT ( 'NONE',  ( -8.786685647604898008, 48.22796981442765940, -23.24040270374399952 ) ) ;
#27459 = CARTESIAN_POINT ( 'NONE',  ( 30.58324630866342986, -120.8793175557614603, 3.944468862007250110 ) ) ;
#27460 = EDGE_CURVE ( 'NONE', #20961, #20579, #7613, .T. ) ;
#27461 = VERTEX_POINT ( 'NONE', #18962 ) ;
#27462 = CARTESIAN_POINT ( 'NONE',  ( -55.24340739397742084, 0.002421372372454598174, 0.009842732675352095298 ) ) ;
#27463 = CARTESIAN_POINT ( 'NONE',  ( -1.048172774974287291, 13.17853518375297739, -43.86067135048624266 ) ) ;
#27464 = CARTESIAN_POINT ( 'NONE',  ( 109.1587776205901577, -0.006995903587858441977, 0.002185517590245231699 ) ) ;
#27465 = ADVANCED_FACE ( 'NONE', ( #5429 ), #1972, .T. ) ;
#27466 = CARTESIAN_POINT ( 'NONE',  ( 55.49584447822657296, 68.91748907713588324, 22.67407039687264714 ) ) ;
#27467 = DIRECTION ( 'NONE',  ( 0.000000000000000000, 5.223019709707975211E-21, -1.000000000000000000 ) ) ;
#27468 = CARTESIAN_POINT ( 'NONE',  ( -22.23342874802668234, 30.68433055777684970, -7.677086057585063017 ) ) ;
#27469 = ORIENTED_EDGE ( 'NONE', *, *, #18279, .T. ) ;
#27470 = CARTESIAN_POINT ( 'NONE',  ( -55.24271866751342941, 0.001425019990779439203, 0.009388511352200054269 ) ) ;
#27471 = AXIS2_PLACEMENT_3D ( 'NONE', #22782, #874, #16131 ) ;
#27472 = CARTESIAN_POINT ( 'NONE',  ( 1.833485406944043827, -29.64752363041439764, -142.0485807715649003 ) ) ;
#27473 = CARTESIAN_POINT ( 'NONE',  ( 109.1587776205901861, 0.002185517590237683917, -0.006995903587863981817 ) ) ;
#27474 = B_SPLINE_CURVE_WITH_KNOTS ( 'NONE', 3,
 ( #22174, #13107, #6355, #26480, #8795, #6785, #24204 ),
 .UNSPECIFIED., .F., .F.,
 ( 4, 3, 4 ),
 ( 2.695974601917670536E-16, 0.009512539173626363698, 0.02506242213020817844 ),
 .UNSPECIFIED. ) ;
#27475 = ORIENTED_EDGE ( 'NONE', *, *, #20880, .F. ) ;
#27476 = VERTEX_POINT ( 'NONE', #12328 ) ;
#27477 = CARTESIAN_POINT ( 'NONE',  ( 32.73300124599735739, -72.21147546950616913, 92.86301839379999024 ) ) ;
#27478 = CARTESIAN_POINT ( 'NONE',  ( 2.430230287190592531, -60.50928654924668137, -132.3371620660956864 ) ) ;
#27479 = SURFACE_SIDE_STYLE ('',( #1428 ) ) ;
#27480 = CARTESIAN_POINT ( 'NONE',  ( 1.832998868059890096, 144.3700883710219216, -14.63705790013863250 ) ) ;
#27481 = CARTESIAN_POINT ( 'NONE',  ( 1.833485406944057594, 125.4007332306555895, -73.01664920992834595 ) ) ;
#27482 = CARTESIAN_POINT ( 'NONE',  ( 16.75465622695671897, 140.8868039942614985, 19.47041796022283577 ) ) ;
#27483 = CARTESIAN_POINT ( 'NONE',  ( -7.078251931573406708, 51.82710018979476985, -5.101176922830847893 ) ) ;
#27484 =( BOUNDED_SURFACE ( )  B_SPLINE_SURFACE ( 3, 1, ( 
 ( #23228, #17146 ),
 ( #14562, #23368 ),
 ( #21033, #27940 ),
 ( #17001, #27812 ) ),
 .UNSPECIFIED., .F., .F., .F. ) 
 B_SPLINE_SURFACE_WITH_KNOTS ( ( 4, 4 ),
 ( 2, 2 ),
 ( 0.000000000000000000, 1.000000000000000000 ),
 ( 0.000000000000000000, 1.000000000000000000 ),
 .UNSPECIFIED. ) 
 GEOMETRIC_REPRESENTATION_ITEM ( )  RATIONAL_B_SPLINE_SURFACE ( (
 ( 1.000000000000000000, 1.000000000000000000),
 ( 0.9956975270656955868, 0.8568959468854907557),
 ( 0.9956975270656955868, 0.8568959468854907557),
 ( 1.000000000000000000, 1.000000000000000000) ) ) 
 REPRESENTATION_ITEM ( '' )  SURFACE ( )  );
#27485 = CARTESIAN_POINT ( 'NONE',  ( 1.833485406944043827, -117.0814567582538501, -85.72460230293812344 ) ) ;
#27486 = EDGE_LOOP ( 'NONE', ( #27946, #6984, #3546, #3672 ) ) ;
#27487 = EDGE_CURVE ( 'NONE', #13900, #1601, #27218, .T. ) ;
#27488 = EDGE_LOOP ( 'NONE', ( #1994, #7121, #19073, #11135 ) ) ;
#27489 = CARTESIAN_POINT ( 'NONE',  ( -1.239374126674604337, -45.98822239537608425, -2.406737988130961181 ) ) ;
#27490 = EDGE_CURVE ( 'NONE', #2493, #16646, #20708, .T. ) ;
#27491 = CARTESIAN_POINT ( 'NONE',  ( -55.24271866751342941, 0.008433070970614317194, 0.004365563123939311327 ) ) ;
#27492 = CARTESIAN_POINT ( 'NONE',  ( 32.73300124599738581, -16.10546300444743650, -116.5274707358856858 ) ) ;
#27493 = CARTESIAN_POINT ( 'NONE',  ( -1.046935749540006011, 12.93334586714240331, 43.93230528057167561 ) ) ;
#27494 = LINE ( 'NONE', #13824, #2802 ) ;
#27495 = CARTESIAN_POINT ( 'NONE',  ( 119.2224693531408803, -90.00000000000005684, 39.99999999999997158 ) ) ;
#27496 = B_SPLINE_CURVE_WITH_KNOTS ( 'NONE', 3,
 ( #9419, #22958, #27387, #25248, #1060, #20485 ),
 .UNSPECIFIED., .F., .F.,
 ( 4, 2, 4 ),
 ( 1.388456241783856658E-17, 0.0006311571484586047049, 0.001262314296917195532 ),
 .UNSPECIFIED. ) ;
#27497 = ORIENTED_EDGE ( 'NONE', *, *, #3742, .F. ) ;
#27498 = CARTESIAN_POINT ( 'NONE',  ( -55.24390624410018802, -0.009209468562452135382, -0.004896917417131697002 ) ) ;
#27499 = CARTESIAN_POINT ( 'NONE',  ( 32.73300124599732186, 0.000000000000000000, 0.000000000000000000 ) ) ;
#27500 = DIRECTION ( 'NONE',  ( 0.7637818620346800147, -0.1788995134688871336, -0.6201872550346648749 ) ) ;
#27501 = ADVANCED_FACE ( 'NONE', ( #3276 ), #24471, .F. ) ;
#27502 = CARTESIAN_POINT ( 'NONE',  ( 55.79472521941428198, 62.63970324008313639, -37.00555938668194500 ) ) ;
#27503 = CARTESIAN_POINT ( 'NONE',  ( 25.64692872815577473, 0.3216598674799600599, -112.9107203549055498 ) ) ;
#27504 = EDGE_CURVE ( 'NONE', #7370, #1405, #24129, .T. ) ;
#27505 = VERTEX_POINT ( 'NONE', #27582 ) ;
#27506 = CARTESIAN_POINT ( 'NONE',  ( 1.834118845439484335, -132.4921483272724174, -59.18411796427184157 ) ) ;
#27507 = CARTESIAN_POINT ( 'NONE',  ( 2.430230287190589422, -28.83279105684524879, 142.6294793592097108 ) ) ;
#27508 = ORIENTED_EDGE ( 'NONE', *, *, #25969, .T. ) ;
#27509 = CIRCLE ( 'NONE', #18770, 53.53553390275978785 ) ;
#27510 = VERTEX_POINT ( 'NONE', #21256 ) ;
#27511 = VERTEX_POINT ( 'NONE', #10342 ) ;
#27512 = CARTESIAN_POINT ( 'NONE',  ( -20.57838717382308147, -16.28767523336102130, 25.16001208503123365 ) ) ;
#27513 = CARTESIAN_POINT ( 'NONE',  ( -1.619063947482197729, -16.67502769180532596, 43.26576862488450104 ) ) ;
#27514 = DIRECTION ( 'NONE',  ( -1.000000000000000000, 0.000000000000000000, 0.000000000000000000 ) ) ;
#27515 = DIRECTION ( 'NONE',  ( -0.7637818620346801257, -0.5092696688508642211, 0.3965875333584858997 ) ) ;
#27516 =( BOUNDED_SURFACE ( )  B_SPLINE_SURFACE ( 3, 1, ( 
 ( #4587, #6908 ),
 ( #2567, #20561 ),
 ( #27174, #2716 ),
 ( #24326, #701 ) ),
 .UNSPECIFIED., .F., .F., .F. ) 
 B_SPLINE_SURFACE_WITH_KNOTS ( ( 4, 4 ),
 ( 2, 2 ),
 ( 0.000000000000000000, 1.000000000000000000 ),
 ( 0.000000000000000000, 1.000000000000000000 ),
 .UNSPECIFIED. ) 
 GEOMETRIC_REPRESENTATION_ITEM ( )  RATIONAL_B_SPLINE_SURFACE ( (
 ( 1.000000000000000000, 1.000000000000000000),
 ( 0.9956975270656955868, 0.8568959468854907557),
 ( 0.9956975270656955868, 0.8568959468854907557),
 ( 1.000000000000000000, 1.000000000000000000) ) ) 
 REPRESENTATION_ITEM ( '' )  SURFACE ( )  );
#27517 = CARTESIAN_POINT ( 'NONE',  ( -20.21097721712958517, 17.13687106192379161, 24.14932359587270483 ) ) ;
#27518 = EDGE_CURVE ( 'NONE', #15104, #4903, #773, .T. ) ;
#27519 = CARTESIAN_POINT ( 'NONE',  ( -1.031422197589711987, 45.78027046666443312, -1.530725436377622151 ) ) ;
#27520 = CARTESIAN_POINT ( 'NONE',  ( 25.64708010899963142, 83.94602815988672262, 75.51173009720550056 ) ) ;
#27521 = EDGE_CURVE ( 'NONE', #13492, #3933, #2135, .T. ) ;
#27522 = B_SPLINE_CURVE_WITH_KNOTS ( 'NONE', 3,
 ( #8556, #3666, #21233, #10577, #27984, #12857 ),
 .UNSPECIFIED., .F., .F.,
 ( 4, 2, 4 ),
 ( 1.965608005753612659E-17, 0.0006311571484586013438, 0.001262314296917182955 ),
 .UNSPECIFIED. ) ;
#27523 = CIRCLE ( 'NONE', #27471, 53.53553390275978785 ) ;
#27524 = CARTESIAN_POINT ( 'NONE',  ( -20.57838717382308147, 25.16001208503129760, 16.28767523336092893 ) ) ;
#27525 = CARTESIAN_POINT ( 'NONE',  ( -20.21097721712959583, -8.835581498567664838, -28.26295595852182529 ) ) ;
#27526 = CARTESIAN_POINT ( 'NONE',  ( 25.64681081121880624, -75.24277141833435678, -84.18689316040122606 ) ) ;
#27527 = CARTESIAN_POINT ( 'NONE',  ( -20.20997486282892552, 1.395963739018065216E-16, 29.60348406988233450 ) ) ;
#27528 = CARTESIAN_POINT ( 'NONE',  ( -1.045287976400362417, -44.00138577190658395, -12.68782741917276446 ) ) ;
#27529 = EDGE_CURVE ( 'NONE', #13048, #23610, #25031, .T. ) ;
#27530 = CARTESIAN_POINT ( 'NONE',  ( 2.430230287190592531, -13.76600171652741267, 144.8619874886005903 ) ) ;
#27531 = CARTESIAN_POINT ( 'NONE',  ( -1.619063947482197729, -2.489035965909835557, 46.30105812165550816 ) ) ;
#27532 = CARTESIAN_POINT ( 'NONE',  ( 25.64703792032467433, -0.1487959541333613023, -112.9111140735909657 ) ) ;
#27533 = CARTESIAN_POINT ( 'NONE',  ( 30.59138290137890337, -60.43009393261900897, -99.26509990456075627 ) ) ;
#27534 = CARTESIAN_POINT ( 'NONE',  ( -9.156249394959713683, 48.78605533024740737, -24.29252099376508056 ) ) ;
#27535 = ORIENTED_EDGE ( 'NONE', *, *, #19954, .F. ) ;
#27536 = LINE ( 'NONE', #7845, #9289 ) ;
#27537 = ORIENTED_EDGE ( 'NONE', *, *, #13331, .F. ) ;
#27538 = CARTESIAN_POINT ( 'NONE',  ( -1.045287976400379737, 44.00138577190644185, -12.68782741917337198 ) ) ;
#27539 = CARTESIAN_POINT ( 'NONE',  ( 25.64681081121879203, -112.9102952884414464, -0.4157506337739698132 ) ) ;
#27540 = VERTEX_POINT ( 'NONE', #17072 ) ;
#27541 = ORIENTED_EDGE ( 'NONE', *, *, #25385, .T. ) ;
#27542 = ORIENTED_EDGE ( 'NONE', *, *, #12228, .T. ) ;
#27543 = DIRECTION ( 'NONE',  ( 0.7637818620346800147, -0.5345501402766247301, 0.3617919495470812152 ) ) ;
#27544 = CARTESIAN_POINT ( 'NONE',  ( -1.239374126674604337, -42.99367564261267916, 16.50008610789344488 ) ) ;
#27545 = CARTESIAN_POINT ( 'NONE',  ( 26.11404676487259024, 108.0249973236467582, 33.91085499298413453 ) ) ;
#27546 = B_SPLINE_CURVE_WITH_KNOTS ( 'NONE', 3,
 ( #2018, #15832, #7072, #4753, #6922, #26757, #2882, #5317 ),
 .UNSPECIFIED., .F., .F.,
 ( 4, 2, 2, 4 ),
 ( 3.469446951953614189E-18, 0.0002429592666046712307, 0.0004859185332093389920, 0.0009718370664186921871 ),
 .UNSPECIFIED. ) ;
#27547 = CARTESIAN_POINT ( 'NONE',  ( 1.834118845439484335, 125.5799175751979959, -72.70910183320437170 ) ) ;
#27548 = EDGE_CURVE ( 'NONE', #704, #28334, #7306, .T. ) ;
#27549 = CARTESIAN_POINT ( 'NONE',  ( -1.619063947482201282, 35.99532424477380488, -29.22875152547769062 ) ) ;
#27550 = CARTESIAN_POINT ( 'NONE',  ( -1.046935749540007343, -12.93334586714209777, -43.93230528057176798 ) ) ;
#27551 = CARTESIAN_POINT ( 'NONE',  ( -8.786685647604890903, -48.22796981442785835, -23.24040270374372952 ) ) ;
#27553 = EDGE_LOOP ( 'NONE', ( #18361, #26444, #21795, #13550 ) ) ;
#27552 = EDGE_CURVE ( 'NONE', #18479, #3085, #26144, .T. ) ;
#27554 = ORIENTED_EDGE ( 'NONE', *, *, #25719, .F. ) ;
#27555 = CARTESIAN_POINT ( 'NONE',  ( -1.050229599974477512, -27.12684363859229109, 36.90196321294325799 ) ) ;
#27557 = CARTESIAN_POINT ( 'NONE',  ( 2.430230287190589422, 126.7388733285345097, 71.49654683843553471 ) ) ;
#27556 = CARTESIAN_POINT ( 'NONE',  ( 1.834118845439484335, -29.99597360112969469, -141.9759513273467917 ) ) ;
#27558 = EDGE_CURVE ( 'NONE', #5199, #10838, #1667, .T. ) ;
#27559 = CARTESIAN_POINT ( 'NONE',  ( 1.833603222531958288, -85.65285110156219162, 117.1340888386546766 ) ) ;
#27560 = CARTESIAN_POINT ( 'NONE',  ( 10.93730112725972425, -79.81734490845995822, 128.3908183996588264 ) ) ;
#27561 = ORIENTED_EDGE ( 'NONE', *, *, #58, .F. ) ;
#27562 = ORIENTED_EDGE ( 'NONE', *, *, #23041, .F. ) ;
#27563 = CARTESIAN_POINT ( 'NONE',  ( 2.433796855181233454, 137.9325382748291418, -46.34326152018600453 ) ) ;
#27564 = CARTESIAN_POINT ( 'NONE',  ( -55.25719721206881729, -0.006045473558784178643, -0.009391134844729129294 ) ) ;
#27565 = CARTESIAN_POINT ( 'NONE',  ( 19.66333377628704682, -133.7337774474999037, -33.01772659807248544 ) ) ;
#27566 = ORIENTED_EDGE ( 'NONE', *, *, #10241, .F. ) ;
#27567 = CARTESIAN_POINT ( 'NONE',  ( 25.64708228042121263, -97.80372460135714618, 56.42152786924468444 ) ) ;
#27568 = CARTESIAN_POINT ( 'NONE',  ( -1.619063947482197729, -38.92136151114925724, -25.20140673341360227 ) ) ;
#27569 =( BOUNDED_SURFACE ( )  B_SPLINE_SURFACE ( 3, 1, ( 
 ( #7488, #2875 ),
 ( #7339, #23189 ),
 ( #7642, #3445 ),
 ( #11654, #8071 ) ),
 .UNSPECIFIED., .F., .F., .F. ) 
 B_SPLINE_SURFACE_WITH_KNOTS ( ( 4, 4 ),
 ( 2, 2 ),
 ( 0.000000000000000000, 1.000000000000000000 ),
 ( 0.000000000000000000, 1.000000000000000000 ),
 .UNSPECIFIED. ) 
 GEOMETRIC_REPRESENTATION_ITEM ( )  RATIONAL_B_SPLINE_SURFACE ( (
 ( 1.000000000000000000, 1.000000000000000000),
 ( 0.6386103224230316178, 0.9954351624131538845),
 ( 0.6386103224230316178, 0.9954351624131538845),
 ( 1.000000000000000000, 1.000000000000000000) ) ) 
 REPRESENTATION_ITEM ( '' )  SURFACE ( )  );
#27570 = ORIENTED_EDGE ( 'NONE', *, *, #15828, .F. ) ;
#27571 = ORIENTED_EDGE ( 'NONE', *, *, #947, .T. ) ;
#27572 = CARTESIAN_POINT ( 'NONE',  ( -5.986830583229479252, 33.39046620690970002, 38.20088153919464702 ) ) ;
#27573 = ORIENTED_EDGE ( 'NONE', *, *, #20102, .T. ) ;
#27574 = CARTESIAN_POINT ( 'NONE',  ( -55.24300891470650754, 0.002702093572893664395, -0.009439835024159005245 ) ) ;
#27575 = VECTOR ( 'NONE', #16998, 1000.000000000000114 ) ;
#27576 = CARTESIAN_POINT ( 'NONE',  ( 2.063896406836609909, 57.85593781835596161, -133.2511741302114956 ) ) ;
#27577 = CARTESIAN_POINT ( 'NONE',  ( 5.340103579038299131, 133.7487108093472443, -62.06990748397718960 ) ) ;
#27578 = CARTESIAN_POINT ( 'NONE',  ( -25.21435515916043713, 23.92354251275973809, 25.00736669480994934 ) ) ;
#27579 = EDGE_CURVE ( 'NONE', #13750, #4626, #1425, .T. ) ;
#27580 = ORIENTED_EDGE ( 'NONE', *, *, #648, .T. ) ;
#27581 = B_SPLINE_CURVE_WITH_KNOTS ( 'NONE', 3,
 ( #17984, #2893, #7511, #22180 ),
 .UNSPECIFIED., .F., .F.,
 ( 4, 4 ),
 ( 3.105545673626859933E-16, 0.01077107486149804332 ),
 .UNSPECIFIED. ) ;
#27582 = CARTESIAN_POINT ( 'NONE',  ( 1.833485406944057594, -44.33323125130021225, 138.1714136985306993 ) ) ;
#27584 = CARTESIAN_POINT ( 'NONE',  ( 109.1778270068192853, -0.003210287141656817823, 0.008743876326153495956 ) ) ;
#27583 = LINE ( 'NONE', #16813, #16197 ) ;
#27585 = CARTESIAN_POINT ( 'NONE',  ( -1.323830074806772172, 28.92190886481864709, -35.86387698262922186 ) ) ;
#27586 = VERTEX_POINT ( 'NONE', #4255 ) ;
#27587 = VERTEX_POINT ( 'NONE', #13037 ) ;
#27588 = VERTEX_POINT ( 'NONE', #10602 ) ;
#27589 = CARTESIAN_POINT ( 'NONE',  ( -23.77929240705205771, 6.464423883190382192, -35.68044874544699496 ) ) ;
#27590 = CARTESIAN_POINT ( 'NONE',  ( 119.2224693531407667, -69.99999999999998579, 20.00000000000007461 ) ) ;
#27592 = CARTESIAN_POINT ( 'NONE',  ( 25.64708228042117000, 11.84161204513409338, -112.2886173090158763 ) ) ;
#27591 = FACE_OUTER_BOUND ( 'NONE', #6114, .T. ) ;
#27593 = CARTESIAN_POINT ( 'NONE',  ( 24.01988960052058886, 49.36855864442128450, 121.3896480498351877 ) ) ;
#27594 = CARTESIAN_POINT ( 'NONE',  ( -25.21435515916043002, 23.92354251275938992, -25.00736669481030106 ) ) ;
#27595 = CARTESIAN_POINT ( 'NONE',  ( -1.583189561560256253, -43.29471907393730135, 16.68617981233747827 ) ) ;
#27596 = CARTESIAN_POINT ( 'NONE',  ( 25.64692232868535626, 45.62640214192403931, -103.2819624397963452 ) ) ;
#27597 = ORIENTED_EDGE ( 'NONE', *, *, #23720, .T. ) ;
#27598 = CARTESIAN_POINT ( 'NONE',  ( -8.786685647604890903, 47.14957014837354876, -25.35688121747519119 ) ) ;
#27599 = CARTESIAN_POINT ( 'NONE',  ( -55.24300891470648622, 0.005486913146696770563, 0.008142823778062024953 ) ) ;
#27600 = DIRECTION ( 'NONE',  ( -0.5914120900931444380, 0.7870418015781071031, -0.1754905759872768534 ) ) ;
#27601 = CARTESIAN_POINT ( 'NONE',  ( 2.063896406836609909, 116.7302989755749252, -86.47093297168882486 ) ) ;
#27602 = CIRCLE ( 'NONE', #23030, 37.50000000000001421 ) ;
#27603 = CARTESIAN_POINT ( 'NONE',  ( 26.11404676487257603, 74.91683232330973397, 84.89295829319517850 ) ) ;
#27604 = CARTESIAN_POINT ( 'NONE',  ( -1.045287976400362417, -28.14015102489855735, -36.12803364096578207 ) ) ;
#27605 = CARTESIAN_POINT ( 'NONE',  ( 6.224689322667647851, -136.2818611715186989, -57.86870174583563653 ) ) ;
#27606 = AXIS2_PLACEMENT_3D ( 'NONE', #11195, #679, #15794 ) ;
#27607 = ORIENTED_EDGE ( 'NONE', *, *, #12996, .F. ) ;
#27608 = CARTESIAN_POINT ( 'NONE',  ( -1.583189561560253589, -46.33203782964459805, 2.490696082060356531 ) ) ;
#27610 = VECTOR ( 'NONE', #14149, 1000.000000000000114 ) ;
#27609 =( BOUNDED_SURFACE ( )  B_SPLINE_SURFACE ( 3, 1, ( 
 ( #7330, #18690 ),
 ( #9925, #20559 ),
 ( #22596, #25177 ),
 ( #5446, #11487 ) ),
 .UNSPECIFIED., .F., .F., .F. ) 
 B_SPLINE_SURFACE_WITH_KNOTS ( ( 4, 4 ),
 ( 2, 2 ),
 ( 0.000000000000000000, 1.000000000000000000 ),
 ( 0.000000000000000000, 1.000000000000000000 ),
 .UNSPECIFIED. ) 
 GEOMETRIC_REPRESENTATION_ITEM ( )  RATIONAL_B_SPLINE_SURFACE ( (
 ( 1.000000000000000000, 1.000000000000000000),
 ( 0.9956975270656955868, 0.8568959468854907557),
 ( 0.9956975270656955868, 0.8568959468854907557),
 ( 1.000000000000000000, 1.000000000000000000) ) ) 
 REPRESENTATION_ITEM ( '' )  SURFACE ( )  );
#27611 = CARTESIAN_POINT ( 'NONE',  ( 10.93730112725977932, -115.5857507957709913, 97.44200844886238144 ) ) ;
#27612 = CARTESIAN_POINT ( 'NONE',  ( -8.786685647604896232, 52.67761315067299677, 9.545808661480061019 ) ) ;
#27613 = ORIENTED_EDGE ( 'NONE', *, *, #20990, .F. ) ;
#27615 = EDGE_CURVE ( 'NONE', #7588, #22495, #22205, .T. ) ;
#27614 = CARTESIAN_POINT ( 'NONE',  ( -1.155001620486251879, -2.068551059060010022, 45.85729774065939779 ) ) ;
#27616 = EDGE_LOOP ( 'NONE', ( #4321, #16141, #19287, #7565 ) ) ;
#27617 = LINE ( 'NONE', #25626, #7062 ) ;
#27618 = CARTESIAN_POINT ( 'NONE',  ( 26.11404676487257603, 12.95861723607603544, -112.4785329405480780 ) ) ;
#27619 = EDGE_CURVE ( 'NONE', #8211, #18556, #18608, .T. ) ;
#27620 = CARTESIAN_POINT ( 'NONE',  ( -22.23342874802668234, 2.180636882146512079, -31.55488258420089664 ) ) ;
#27621 = ADVANCED_FACE ( 'NONE', ( #6570 ), #26295, .F. ) ;
#27622 = VECTOR ( 'NONE', #8844, 1000.000000000000114 ) ;
#27623 = B_SPLINE_CURVE_WITH_KNOTS ( 'NONE', 3,
 ( #5750, #18832, #25476, #16830, #1552, #9924, #5888 ),
 .UNSPECIFIED., .F., .F.,
 ( 4, 3, 4 ),
 ( 3.469446951953614189E-18, 0.009512539173626381045, 0.02506242213020843518 ),
 .UNSPECIFIED. ) ;
#27624 = CARTESIAN_POINT ( 'NONE',  ( 25.64681081121880624, -23.06870491922396837, 110.5293738517607665 ) ) ;
#27625 = CARTESIAN_POINT ( 'NONE',  ( -20.57838717382308147, -10.78122205917020437, -27.96569011373082603 ) ) ;
#27626 = FACE_OUTER_BOUND ( 'NONE', #3470, .T. ) ;
#27627 = VECTOR ( 'NONE', #17710, 1000.000000000000000 ) ;
#27628 = EDGE_CURVE ( 'NONE', #27099, #14753, #12109, .T. ) ;
#27629 = CARTESIAN_POINT ( 'NONE',  ( 1.833603222531969834, -59.42758433816056396, 132.3826570575581059 ) ) ;
#27630 = CARTESIAN_POINT ( 'NONE',  ( 25.64704443564079028, 112.3065506427463305, -11.66968230815798258 ) ) ;
#27631 = CARTESIAN_POINT ( 'NONE',  ( 55.79472521941426777, 28.92526238350474088, 66.75682020267539940 ) ) ;
#27632 = VERTEX_POINT ( 'NONE', #15040 ) ;
#27633 = CIRCLE ( 'NONE', #3266, 117.6351876552689504 ) ;
#27634 = ORIENTED_EDGE ( 'NONE', *, *, #11182, .F. ) ;
#27635 = CARTESIAN_POINT ( 'NONE',  ( -1.155031165708881646, -42.97366960678589720, 16.13806347973043387 ) ) ;
#27636 = CARTESIAN_POINT ( 'NONE',  ( 109.1778270068192853, -0.009177562596833058889, -0.001591747944966620271 ) ) ;
#27637 = DIRECTION ( 'NONE',  ( 0.000000000000000000, 0.000000000000000000, -1.000000000000000000 ) ) ;
#27638 = CARTESIAN_POINT ( 'NONE',  ( 1.833485406944043827, 144.2578170162062747, 15.69895494453433393 ) ) ;
#27639 = CARTESIAN_POINT ( 'NONE',  ( 2.108985857320911705, 107.1123114102940690, -98.16869034643197267 ) ) ;
#27640 = CARTESIAN_POINT ( 'NONE',  ( -8.259864102781671491, 52.60025989855203221, -6.590267880897108022 ) ) ;
#27641 = CARTESIAN_POINT ( 'NONE',  ( 2.063896406836609909, 142.3682421260907631, 28.88716984836368695 ) ) ;
#27642 = VERTEX_POINT ( 'NONE', #12884 ) ;
#27643 = DIRECTION ( 'NONE',  ( -0.5914120900931443270, -0.7398809652417984717, -0.3206367055789513532 ) ) ;
#27644 = FACE_OUTER_BOUND ( 'NONE', #1, .T. ) ;
#27645 = CARTESIAN_POINT ( 'NONE',  ( 25.70243777736190438, -11.07690056740789331, -112.4037002646849004 ) ) ;
#27646 = CARTESIAN_POINT ( 'NONE',  ( -28.13707043255157103, -18.06394523322443035, 14.07296284901352479 ) ) ;
#27647 = CARTESIAN_POINT ( 'NONE',  ( 109.1587776205901577, 0.002343968083389357145, -0.006944419901758100769 ) ) ;
#27648 = VERTEX_POINT ( 'NONE', #23583 ) ;
#27649 = CARTESIAN_POINT ( 'NONE',  ( 1.833809397773875638, 145.1096615951801709, 0.1779672212505475359 ) ) ;
#27650 = VECTOR ( 'NONE', #26259, 1000.000000000000114 ) ;
#27651 = CARTESIAN_POINT ( 'NONE',  ( 109.1586900883932856, 0.002810909342002405019, -0.006561743627145274170 ) ) ;
#27652 = VERTEX_POINT ( 'NONE', #1948 ) ;
#27653 = VECTOR ( 'NONE', #5786, 1000.000000000000227 ) ;
#27654 = VERTEX_POINT ( 'NONE', #7148 ) ;
#27655 = EDGE_LOOP ( 'NONE', ( #13479, #4695, #18445, #27901 ) ) ;
#27656 = CONICAL_SURFACE ( 'NONE', #15220, 117.6351876552689504, 0.9945805576725580410 ) ;
#27657 = EDGE_CURVE ( 'NONE', #17196, #22112, #27732, .T. ) ;
#27658 =( BOUNDED_SURFACE ( )  B_SPLINE_SURFACE ( 3, 1, ( 
 ( #17502, #26290 ),
 ( #3990, #6587 ),
 ( #12761, #1819 ),
 ( #10618, #23877 ) ),
 .UNSPECIFIED., .F., .F., .F. ) 
 B_SPLINE_SURFACE_WITH_KNOTS ( ( 4, 4 ),
 ( 2, 2 ),
 ( 0.000000000000000000, 1.000000000000000000 ),
 ( 0.000000000000000000, 1.000000000000000000 ),
 .UNSPECIFIED. ) 
 GEOMETRIC_REPRESENTATION_ITEM ( )  RATIONAL_B_SPLINE_SURFACE ( (
 ( 1.000000000000000000, 1.000000000000000000),
 ( 0.9934239774497837239, 0.8357310067453919133),
 ( 0.9934239774497837239, 0.8357310067453919133),
 ( 1.000000000000000000, 1.000000000000000000) ) ) 
 REPRESENTATION_ITEM ( '' )  SURFACE ( )  );
#27659 = CARTESIAN_POINT ( 'NONE',  ( 16.05277956358206026, -34.34928806929325162, -139.1285124304122292 ) ) ;
#27660 = CARTESIAN_POINT ( 'NONE',  ( 16.75465622695652357, -136.6258322711653648, 39.51671382433896440 ) ) ;
#27661 = ADVANCED_FACE ( 'NONE', ( #11443 ), #6812, .F. ) ;
#27662 = CARTESIAN_POINT ( 'NONE',  ( -90.83090735639699176, 0.000000000000000000, 0.000000000000000000 ) ) ;
#27663 = CARTESIAN_POINT ( 'NONE',  ( -1.058473599757824735, 1.755404039370064950, 45.77379534793241334 ) ) ;
#27664 = ORIENTED_EDGE ( 'NONE', *, *, #10806, .T. ) ;
#27665 = B_SPLINE_CURVE_WITH_KNOTS ( 'NONE', 3,
 ( #27752, #22884, #27593, #12340, #3703, #27310, #8054 ),
 .UNSPECIFIED., .F., .F.,
 ( 4, 3, 4 ),
 ( 0.000000000000000000, 0.02398743853561340067, 0.04000277880656211149 ),
 .UNSPECIFIED. ) ;
#27666 = DIRECTION ( 'NONE',  ( -1.000000000000000000, -0.000000000000000000, -0.000000000000000000 ) ) ;
#27667 = CARTESIAN_POINT ( 'NONE',  ( 32.73300124599735739, -28.19767303745682341, 114.2056417606547285 ) ) ;
#27668 = B_SPLINE_CURVE_WITH_KNOTS ( 'NONE', 3,
 ( #22575, #2543, #13627, #24742 ),
 .UNSPECIFIED., .F., .F.,
 ( 4, 4 ),
 ( 3.372266854755940974E-16, 0.01077107486149835383 ),
 .UNSPECIFIED. ) ;
#27669 = DIRECTION ( 'NONE',  ( -1.000000000000000000, -0.000000000000000000, -0.000000000000000000 ) ) ;
#27670 = CARTESIAN_POINT ( 'NONE',  ( 25.64681081121880624, 102.9795863647034935, -46.30456157731225630 ) ) ;
#27671 = CARTESIAN_POINT ( 'NONE',  ( 26.28373643307416785, 43.35364178852768191, 119.9673604189456739 ) ) ;
#27672 = CARTESIAN_POINT ( 'NONE',  ( 109.1721716018069657, 0.01019541462303493601, 0.01368917435591437623 ) ) ;
#27673 = CIRCLE ( 'NONE', #13876, 151.1787379149930359 ) ;
#27674 = DIRECTION ( 'NONE',  ( 0.7563875759206388771, -0.6104009704506944134, -0.2351350468682844030 ) ) ;
#27675 = CARTESIAN_POINT ( 'NONE',  ( 5.340103556456508471, -146.3832391989195116, -17.70136535450057380 ) ) ;
#27676 = FACE_OUTER_BOUND ( 'NONE', #642, .T. ) ;
#27677 = CARTESIAN_POINT ( 'NONE',  ( 26.11404676487257603, -57.58742681967381571, -97.48350837663670632 ) ) ;
#27678 = CARTESIAN_POINT ( 'NONE',  ( 21.16825799904901828, -106.9139171613931580, 83.13600836828973684 ) ) ;
#27679 = CARTESIAN_POINT ( 'NONE',  ( 25.73574536432418114, 12.61003673872037112, -112.2643803187782936 ) ) ;
#27680 = ORIENTED_EDGE ( 'NONE', *, *, #17130, .T. ) ;
#27681 = CARTESIAN_POINT ( 'NONE',  ( 109.1721716018069515, 0.01699510305643760558, -0.001583175916617861941 ) ) ;
#27682 = EDGE_LOOP ( 'NONE', ( #3639, #7262, #8851, #26955 ) ) ;
#27683 = CARTESIAN_POINT ( 'NONE',  ( 1.831572820252009626, 141.7320553118910027, -31.13525033585354151 ) ) ;
#27684 = B_SPLINE_CURVE_WITH_KNOTS ( 'NONE', 3,
 ( #20762, #11847, #14272, #762, #9687, #20618, #16159, #1055 ),
 .UNSPECIFIED., .F., .F.,
 ( 4, 2, 2, 4 ),
 ( 6.938893903907228378E-18, 0.0002429588503611349287, 0.0004859177007222629185, 0.0009718354014444958045 ),
 .UNSPECIFIED. ) ;
#27686 = VERTEX_POINT ( 'NONE', #4962 ) ;
#27685 = FACE_OUTER_BOUND ( 'NONE', #19574, .T. ) ;
#27687 = EDGE_LOOP ( 'NONE', ( #12386, #4572, #25580, #11685 ) ) ;
#27688 = ORIENTED_EDGE ( 'NONE', *, *, #24527, .T. ) ;
#27689 = VERTEX_POINT ( 'NONE', #13594 ) ;
#27690 = EDGE_CURVE ( 'NONE', #20457, #7798, #22016, .T. ) ;
#27691 = EDGE_CURVE ( 'NONE', #25194, #23301, #18226, .T. ) ;
#27692 = B_SPLINE_CURVE_WITH_KNOTS ( 'NONE', 3,
 ( #9629, #22037, #22894, #18394 ),
 .UNSPECIFIED., .F., .F.,
 ( 4, 4 ),
 ( 6.133075535169769447E-16, 0.008383748772660102461 ),
 .UNSPECIFIED. ) ;
#27693 = VECTOR ( 'NONE', #24719, 1000.000000000000000 ) ;
#27694 = CARTESIAN_POINT ( 'NONE',  ( 60.46576798286869803, -4.195655488513964285E-16, 1.048913872128491071E-16 ) ) ;
#27695 = AXIS2_PLACEMENT_3D ( 'NONE', #17167, #6521, #8401 ) ;
#27696 = ADVANCED_FACE ( 'NONE', ( #26838 ), #13736, .F. ) ;
#27697 = CARTESIAN_POINT ( 'NONE',  ( 1.833838850093440387, -141.9387658801233556, 30.17001957361944520 ) ) ;
#27698 = EDGE_CURVE ( 'NONE', #4083, #28198, #20995, .T. ) ;
#27699 = CARTESIAN_POINT ( 'NONE',  ( -21.41430102051745266, -29.81033373822133470, -7.777552968935644628 ) ) ;
#27700 = CARTESIAN_POINT ( 'NONE',  ( -55.24271866751342941, -0.001425019990778747699, -0.009388511352200236415 ) ) ;
#27701 = CARTESIAN_POINT ( 'NONE',  ( 8.186469777910758694, 63.89871389959457559, 134.9918587298865873 ) ) ;
#27702 = CARTESIAN_POINT ( 'NONE',  ( 1.833485406944057594, 72.09189602597886903, -125.9346397303427665 ) ) ;
#27703 = B_SPLINE_CURVE_WITH_KNOTS ( 'NONE', 3,
 ( #22255, #2512, #2963, #7278 ),
 .UNSPECIFIED., .F., .F.,
 ( 4, 4 ),
 ( 2.928344767506750777E-16, 0.008383748772659755516 ),
 .UNSPECIFIED. ) ;
#27704 = CARTESIAN_POINT ( 'NONE',  ( 55.79472521941428198, 66.16469064668339684, -30.25520714117840626 ) ) ;
#27705 = CARTESIAN_POINT ( 'NONE',  ( 25.69398547355838147, -112.3990349503584980, -11.06723946918872237 ) ) ;
#27706 = ORIENTED_EDGE ( 'NONE', *, *, #16616, .T. ) ;
#27707 = ORIENTED_EDGE ( 'NONE', *, *, #19856, .T. ) ;
#27708 = CARTESIAN_POINT ( 'NONE',  ( 109.1587776205901861, 0.002343968083398739830, 0.006944419901758138065 ) ) ;
#27710 = CARTESIAN_POINT ( 'NONE',  ( -25.21435515916043713, 6.169479169075932745, 34.05351380035326514 ) ) ;
#27709 = CARTESIAN_POINT ( 'NONE',  ( 2.433796855181219243, 133.5135467655526043, -57.85512797797757401 ) ) ;
#27711 = CARTESIAN_POINT ( 'NONE',  ( 26.11404676487257603, -36.06104232266378062, -107.3263591096434197 ) ) ;
#27712 = CARTESIAN_POINT ( 'NONE',  ( 24.22246935314087324, 90.00000000000005684, 39.99999999999999289 ) ) ;
#27713 = CARTESIAN_POINT ( 'NONE',  ( 25.70243777736186530, 90.94412140945959777, 66.98101477609036181 ) ) ;
#27714 = AXIS2_PLACEMENT_3D ( 'NONE', #1399, #1676, #28289 ) ;
#27715 = ORIENTED_EDGE ( 'NONE', *, *, #16475, .F. ) ;
#27716 = DIRECTION ( 'NONE',  ( -0.7637818620346801257, 0.5092696688508612235, -0.3965875333584896190 ) ) ;
#27717 = AXIS2_PLACEMENT_3D ( 'NONE', #19009, #16856, #27790 ) ;
#27718 = CARTESIAN_POINT ( 'NONE',  ( -1.044557008772710960, 36.05793264791386576, 28.22896138707331204 ) ) ;
#27719 = CARTESIAN_POINT ( 'NONE',  ( 2.433796855181219243, -116.8607839509062671, 86.69855925933937613 ) ) ;
#27720 = ORIENTED_EDGE ( 'NONE', *, *, #3330, .F. ) ;
#27721 = ORIENTED_EDGE ( 'NONE', *, *, #25164, .F. ) ;
#27722 = CARTESIAN_POINT ( 'NONE',  ( 55.79472521941428198, -42.17269936297680033, 59.28412330436287192 ) ) ;
#27723 = VERTEX_POINT ( 'NONE', #26549 ) ;
#27724 = B_SPLINE_CURVE_WITH_KNOTS ( 'NONE', 3,
 ( #4987, #530, #13759, #22720, #17928, #26714 ),
 .UNSPECIFIED., .F., .F.,
 ( 4, 2, 4 ),
 ( 1.499206600309199041E-16, 0.003570751334075636992, 0.007141502668151123931 ),
 .UNSPECIFIED. ) ;
#27725 = EDGE_CURVE ( 'NONE', #24971, #22236, #11724, .T. ) ;
#27726 = B_SPLINE_CURVE_WITH_KNOTS ( 'NONE', 3,
 ( #16822, #23173, #25469, #5588 ),
 .UNSPECIFIED., .F., .F.,
 ( 4, 4 ),
 ( 3.770221040707433269E-16, 0.01077107486149843883 ),
 .UNSPECIFIED. ) ;
#27727 = DIRECTION ( 'NONE',  ( 1.000000000000000000, -0.000000000000000000, -0.000000000000000000 ) ) ;
#27728 = VERTEX_POINT ( 'NONE', #18057 ) ;
#27729 = ADVANCED_FACE ( 'NONE', ( #18195 ), #14868, .T. ) ;
#27730 = CARTESIAN_POINT ( 'NONE',  ( 32.73300124599732186, 0.000000000000000000, 0.000000000000000000 ) ) ;
#27731 = CARTESIAN_POINT ( 'NONE',  ( 109.1586900883932856, -0.002810909342002450555, 0.006561743627145253353 ) ) ;
#27732 = CIRCLE ( 'NONE', #23153, 12.50000000000000178 ) ;
#27733 = CARTESIAN_POINT ( 'NONE',  ( -7.078251931573406708, 51.82710018979476985, -5.101176922830847893 ) ) ;
#27734 = VECTOR ( 'NONE', #509, 999.9999999999998863 ) ;
#27735 = B_SPLINE_CURVE_WITH_KNOTS ( 'NONE', 3,
 ( #12809, #6345, #23497, #8638, #6220, #2010, #3763, #16993, #4174, #21316 ),
 .UNSPECIFIED., .F., .F.,
 ( 4, 3, 3, 4 ),
 ( 0.001530725384384652287, 0.001531419946797919589, 0.002296279302920155134, 0.003061450627205758099 ),
 .UNSPECIFIED. ) ;
#27736 = CARTESIAN_POINT ( 'NONE',  ( -28.41354790283022069, 18.00456980371921034, 14.62505768302780851 ) ) ;
#27737 = CARTESIAN_POINT ( 'NONE',  ( -25.21435515916025594, 1.749597353048488237E-16, -4.373993382621220594E-17 ) ) ;
#27738 = CARTESIAN_POINT ( 'NONE',  ( 13.84597867724990294, 146.6243035057529482, 4.782757490006329881 ) ) ;
#27739 = DIRECTION ( 'NONE',  ( -0.7637818620346801257, -0.02150485345385289709, -0.6451161201712178883 ) ) ;
#27740 = VERTEX_POINT ( 'NONE', #20076 ) ;
#27741 = CARTESIAN_POINT ( 'NONE',  ( 30.59141879584285917, -107.2355637993505582, 44.78722686469172487 ) ) ;
#27743 = CARTESIAN_POINT ( 'NONE',  ( -55.25719721206881729, -0.01041086141212241994, -0.004044147484874939351 ) ) ;
#27742 = CARTESIAN_POINT ( 'NONE',  ( 30.58324630866353289, 92.47020419020178394, 77.95273942827370206 ) ) ;
#27744 = CARTESIAN_POINT ( 'NONE',  ( -20.20700224038492010, -0.9908225410480588913, -29.58392382092672435 ) ) ;
#27745 = ORIENTED_EDGE ( 'NONE', *, *, #12823, .F. ) ;
#27746 = ORIENTED_EDGE ( 'NONE', *, *, #21292, .T. ) ;
#27747 = VERTEX_POINT ( 'NONE', #2809 ) ;
#27748 = CARTESIAN_POINT ( 'NONE',  ( -1.031422197589711987, -1.530725436377782467, -45.78027046666441890 ) ) ;
#27749 = LINE ( 'NONE', #23018, #20354 ) ;
#27751 = DIRECTION ( 'NONE',  ( 0.000000000000000000, 0.000000000000000000, 1.000000000000000000 ) ) ;
#27750 = CARTESIAN_POINT ( 'NONE',  ( 109.1589550718174877, -0.007132058561965932270, -0.002553077953671684542 ) ) ;
#27752 = CARTESIAN_POINT ( 'NONE',  ( 32.73300124599735739, 44.31599526637956643, 108.9684813982490539 ) ) ;
#27753 = CARTESIAN_POINT ( 'NONE',  ( -25.21435515916025594, 1.749597353048488237E-16, -4.373993382621220594E-17 ) ) ;
#27754 = EDGE_LOOP ( 'NONE', ( #5475, #14190, #3174, #6487 ) ) ;
#27755 = CARTESIAN_POINT ( 'NONE',  ( -24.53239521893645048, 22.94500969220232633, -24.99972072650149713 ) ) ;
#27756 = FACE_OUTER_BOUND ( 'NONE', #8260, .T. ) ;
#27757 = ORIENTED_EDGE ( 'NONE', *, *, #27194, .F. ) ;
#27758 = CARTESIAN_POINT ( 'NONE',  ( 1.833206310202336820, -0.7447039688715555439, -145.1075835704899362 ) ) ;
#27759 = CARTESIAN_POINT ( 'NONE',  ( 55.79472521941428198, -28.92526238350520273, 66.75682020267520045 ) ) ;
#27760 = CARTESIAN_POINT ( 'NONE',  ( 2.430230287190592531, 137.9371479820468949, -46.34481016236681228 ) ) ;
#27761 = CARTESIAN_POINT ( 'NONE',  ( 25.64692872815575697, 107.2850779876534233, 35.19724814977951866 ) ) ;
#27762 = DIRECTION ( 'NONE',  ( 0.5914120900931444380, -0.07630783613000820254, -0.8027508043202538079 ) ) ;
#27763 = APPLICATION_CONTEXT ( 'automotive_design' ) ;
#27764 = CARTESIAN_POINT ( 'NONE',  ( -55.24728320129491266, 0.01402509393918179546, 0.003868537197316780987 ) ) ;
#27765 = EDGE_LOOP ( 'NONE', ( #15307, #11394, #13297, #11473 ) ) ;
#27766 = CARTESIAN_POINT ( 'NONE',  ( 2.430230287190592531, 13.76600171652835947, -144.8619874886005334 ) ) ;
#27767 =( GEOMETRIC_REPRESENTATION_CONTEXT ( 3 ) GLOBAL_UNCERTAINTY_ASSIGNED_CONTEXT ( ( #7976 ) ) GLOBAL_UNIT_ASSIGNED_CONTEXT ( ( #7605, #22864, #14183 ) ) REPRESENTATION_CONTEXT ( 'NONE', 'WORKASPACE' ) );
#27768 = CARTESIAN_POINT ( 'NONE',  ( 1.834118845439484335, 117.2918069668801024, 85.43746956709887286 ) ) ;
#27769 = CARTESIAN_POINT ( 'NONE',  ( -28.41354790283022069, 21.64275480268748453, -8.345538364877153725 ) ) ;
#27770 = EDGE_CURVE ( 'NONE', #23613, #19718, #5195, .T. ) ;
#27771 = B_SPLINE_CURVE_WITH_KNOTS ( 'NONE', 3,
 ( #14584, #23250, #5678, #22963 ),
 .UNSPECIFIED., .F., .F.,
 ( 4, 4 ),
 ( 4.496917212498578222E-17, 0.008383748772659509185 ),
 .UNSPECIFIED. ) ;
#27772 = VERTEX_POINT ( 'NONE', #26971 ) ;
#27773 = CARTESIAN_POINT ( 'NONE',  ( -1.058197053496169548, 38.06270006878853707, -25.48582931365482906 ) ) ;
#27774 = ORIENTED_EDGE ( 'NONE', *, *, #20614, .F. ) ;
#27775 = EDGE_CURVE ( 'NONE', #6393, #20633, #13883, .T. ) ;
#27776 = ADVANCED_FACE ( 'NONE', ( #20504 ), #11763, .F. ) ;
#27777 = CARTESIAN_POINT ( 'NONE',  ( -1.050229599974462413, -45.79907399707869331, -0.2556477501657915541 ) ) ;
#27778 = CARTESIAN_POINT ( 'NONE',  ( 1.833485406944043827, 73.01664920993141550, -125.4007332306537563 ) ) ;
#27779 = CARTESIAN_POINT ( 'NONE',  ( -1.048996300304477769, -13.42280206896947092, 43.78665266739852058 ) ) ;
#27780 = CARTESIAN_POINT ( 'NONE',  ( 25.64692232868535982, -23.15582834340360918, 110.5112661748244562 ) ) ;
#27781 = CARTESIAN_POINT ( 'NONE',  ( 55.49584447822657296, 62.69727227546452752, -36.50733923851132090 ) ) ;
#27782 = CARTESIAN_POINT ( 'NONE',  ( 2.433796855181233454, 116.8607839509068498, -86.69855925933855190 ) ) ;
#27783 = CARTESIAN_POINT ( 'NONE',  ( 1.833691583653512369, -59.34641645332730064, 132.4191286035304529 ) ) ;
#27784 = CARTESIAN_POINT ( 'NONE',  ( 25.87036335909427365, -74.91347493818321368, 84.67915015758833874 ) ) ;
#27785 = CARTESIAN_POINT ( 'NONE',  ( 2.263178113027036975, -16.59120315151675129, 144.4462808674009580 ) ) ;
#27786 = VERTEX_POINT ( 'NONE', #7864 ) ;
#27787 = VERTEX_POINT ( 'NONE', #27549 ) ;
#27788 = CARTESIAN_POINT ( 'NONE',  ( 25.65782528836479415, -97.50004228081019164, -56.95887699624839939 ) ) ;
#27789 = B_SPLINE_CURVE_WITH_KNOTS ( 'NONE', 3,
 ( #8717, #6160, #28143, #8303, #21956, #2217, #81 ),
 .UNSPECIFIED., .F., .F.,
 ( 4, 3, 4 ),
 ( 0.000000000000000000, 0.02398743853561346312, 0.04000277880656213231 ),
 .UNSPECIFIED. ) ;
#27790 = DIRECTION ( 'NONE',  ( 0.000000000000000000, 5.223019709707975211E-21, -1.000000000000000000 ) ) ;
#27791 = CARTESIAN_POINT ( 'NONE',  ( 2.433796855181205476, -46.34326152018838485, 137.9325382748283744 ) ) ;
#27792 = CARTESIAN_POINT ( 'NONE',  ( 32.73300124599735739, -105.8473486001054482, 51.32617430724869223 ) ) ;
#27793 = FACE_OUTER_BOUND ( 'NONE', #24297, .T. ) ;
#27794 = DIRECTION ( 'NONE',  ( 0.5914120900931444380, 0.7643865440136088374, 0.2567974902965169393 ) ) ;
#27795 = DIRECTION ( 'NONE',  ( 0.5914120900931444380, 0.2415416038592911596, 0.7693434820005559116 ) ) ;
#27796 = ORIENTED_EDGE ( 'NONE', *, *, #1030, .F. ) ;
#27797 = CARTESIAN_POINT ( 'NONE',  ( 1.833721034905636982, -144.2772269874177482, 15.52204855105793158 ) ) ;
#27798 = FACE_OUTER_BOUND ( 'NONE', #24042, .T. ) ;
#27799 = CARTESIAN_POINT ( 'NONE',  ( 5.340103579038177450, 88.52145169228961663, 117.9209211655060443 ) ) ;
#27800 = CARTESIAN_POINT ( 'NONE',  ( 2.433796855181219243, -137.9325382748288291, 46.34326152018696376 ) ) ;
#27801 = CARTESIAN_POINT ( 'NONE',  ( 109.1592201516379674, -0.007748443302128564178, 0.001331853079208289697 ) ) ;
#27802 = EDGE_CURVE ( 'NONE', #12568, #14056, #8012, .T. ) ;
#27803 = ORIENTED_EDGE ( 'NONE', *, *, #3156, .T. ) ;
#27804 = CARTESIAN_POINT ( 'NONE',  ( 32.73300124599738581, 32.68291970228383292, -113.0038235389598782 ) ) ;
#27805 = DIRECTION ( 'NONE',  ( 0.000000000000000000, 0.000000000000000000, 1.000000000000000000 ) ) ;
#27806 = ORIENTED_EDGE ( 'NONE', *, *, #26125, .T. ) ;
#27807 = EDGE_CURVE ( 'NONE', #14489, #24734, #14471, .T. ) ;
#27808 = ORIENTED_EDGE ( 'NONE', *, *, #24732, .F. ) ;
#27809 = ORIENTED_EDGE ( 'NONE', *, *, #28375, .F. ) ;
#27810 = CARTESIAN_POINT ( 'NONE',  ( 25.65782528836479770, -107.5689571161381366, 34.34372400279215753 ) ) ;
#27811 = CARTESIAN_POINT ( 'NONE',  ( 109.1586900883932856, 0.006960773163852190457, -0.001582822706032850245 ) ) ;
#27812 = CARTESIAN_POINT ( 'NONE',  ( 2.430230287190581429, -57.85706160874058668, -133.5180086894997089 ) ) ;
#27813 = CARTESIAN_POINT ( 'NONE',  ( -1.583189561560255143, 11.94859433442965546, 44.83405390829658188 ) ) ;
#27814 = FACE_OUTER_BOUND ( 'NONE', #13586, .T. ) ;
#27815 = CARTESIAN_POINT ( 'NONE',  ( -1.155031165708874097, 45.85732438018715129, -2.068616213631106593 ) ) ;
#27816 = CARTESIAN_POINT ( 'NONE',  ( -24.53237795827026346, 24.99972053297905461, -22.94498492516348520 ) ) ;
#27817 = CARTESIAN_POINT ( 'NONE',  ( 55.49584447822657296, 53.73688382046265843, 48.74506217377899731 ) ) ;
#27818 = CARTESIAN_POINT ( 'NONE',  ( 109.1586059443104944, -0.003930911098385119970, 0.005881369279880081791 ) ) ;
#27819 = CARTESIAN_POINT ( 'NONE',  ( 25.64700659047694131, -12.02873506870245457, 112.2686754657454600 ) ) ;
#27820 = CARTESIAN_POINT ( 'NONE',  ( -28.41354790283022069, -21.64275480268754137, -8.345538364876993853 ) ) ;
#27821 = CARTESIAN_POINT ( 'NONE',  ( 16.05277956358234448, 118.6216415718956796, 80.40847413522560316 ) ) ;
#27822 = LINE ( 'NONE', #18756, #16828 ) ;
#27823 = CARTESIAN_POINT ( 'NONE',  ( 16.75465622695648804, 141.8562168210796415, -10.24707101927895181 ) ) ;
#27824 = CARTESIAN_POINT ( 'NONE',  ( -55.24390624410018802, -0.009209468562452135382, -0.004896917417131697002 ) ) ;
#27825 = EDGE_CURVE ( 'NONE', #3085, #20088, #12731, .T. ) ;
#27826 = ORIENTED_EDGE ( 'NONE', *, *, #3755, .F. ) ;
#27827 = EDGE_CURVE ( 'NONE', #16498, #2445, #26791, .T. ) ;
#27828 = ORIENTED_EDGE ( 'NONE', *, *, #3462, .F. ) ;
#27829 = CARTESIAN_POINT ( 'NONE',  ( 1.832998868059890096, 15.69902610990563474, -144.2584710144578821 ) ) ;
#27830 = CARTESIAN_POINT ( 'NONE',  ( 2.433796855181219243, -31.67151202412867761, -142.0211193075559493 ) ) ;
#27831 = VERTEX_POINT ( 'NONE', #24995 ) ;
#27832 =( BOUNDED_SURFACE ( )  B_SPLINE_SURFACE ( 3, 1, ( 
 ( #23485, #12520 ),
 ( #8221, #4088 ),
 ( #2193, #17319 ),
 ( #19761, #26390 ) ),
 .UNSPECIFIED., .F., .F., .F. ) 
 B_SPLINE_SURFACE_WITH_KNOTS ( ( 4, 4 ),
 ( 2, 2 ),
 ( 0.000000000000000000, 1.000000000000000000 ),
 ( 0.000000000000000000, 1.000000000000000000 ),
 .UNSPECIFIED. ) 
 GEOMETRIC_REPRESENTATION_ITEM ( )  RATIONAL_B_SPLINE_SURFACE ( (
 ( 1.000000000000000000, 1.000000000000000000),
 ( 0.9593753223639863714, 0.9995975284513187731),
 ( 0.9593753223639863714, 0.9995975284513187731),
 ( 1.000000000000000000, 1.000000000000000000) ) ) 
 REPRESENTATION_ITEM ( '' )  SURFACE ( )  );
#27833 = VERTEX_POINT ( 'NONE', #25558 ) ;
#27834 = VERTEX_POINT ( 'NONE', #5250 ) ;
#27835 = CARTESIAN_POINT ( 'NONE',  ( -28.13707043255157103, -18.96624908365836859, 12.83104814250474668 ) ) ;
#27836 = CARTESIAN_POINT ( 'NONE',  ( 2.108393763691174705, -73.75286979200549808, 125.1820217068194410 ) ) ;
#27837 = AXIS2_PLACEMENT_3D ( 'NONE', #20913, #9994, #9374 ) ;
#27838 = CARTESIAN_POINT ( 'NONE',  ( 32.73300124599737870, -117.5726003567929041, -3.836798148480059734 ) ) ;
#27839 = CARTESIAN_POINT ( 'NONE',  ( -20.20700224038492721, 0.9908225410482660589, 29.58392382092671724 ) ) ;
#27840 = CARTESIAN_POINT ( 'NONE',  ( 2.108985857320948565, 71.53406810961664064, -126.4634971826977505 ) ) ;
#27841 = CARTESIAN_POINT ( 'NONE',  ( -1.045287976400365970, 45.76855895860946077, 1.530335034933974381 ) ) ;
#27842 = B_SPLINE_CURVE_WITH_KNOTS ( 'NONE', 3,
 ( #26639, #13548, #18000, #8817 ),
 .UNSPECIFIED., .F., .F.,
 ( 4, 4 ),
 ( 0.000000000000000000, 0.008383560773332705135 ),
 .UNSPECIFIED. ) ;
#27843 = CARTESIAN_POINT ( 'NONE',  ( -22.23342874802668234, 29.33662284748876914, 11.82490389046284029 ) ) ;
#27844 = CARTESIAN_POINT ( 'NONE',  ( -1.539760825549682188, -44.72358953107742252, -11.93465943778497262 ) ) ;
#27845 = CARTESIAN_POINT ( 'NONE',  ( -8.786685647604890903, -9.545808661480235102, 52.67761315067295413 ) ) ;
#27846 = EDGE_CURVE ( 'NONE', #20232, #4864, #4519, .T. ) ;
#27847 = ORIENTED_EDGE ( 'NONE', *, *, #10379, .T. ) ;
#27848 = EDGE_LOOP ( 'NONE', ( #4483, #19485, #25457, #4420 ) ) ;
#27849 = CARTESIAN_POINT ( 'NONE',  ( 25.64681081121879203, -107.2555980796238657, -35.28660243342658731 ) ) ;
#27850 = EDGE_CURVE ( 'NONE', #15703, #7068, #4176, .T. ) ;
#27852 = CARTESIAN_POINT ( 'NONE',  ( 109.1778270068192853, -0.001322180554006250003, 0.009220257877172547203 ) ) ;
#27851 = CARTESIAN_POINT ( 'NONE',  ( -1.058473599757817185, 28.32531354681336566, 35.99997772736180224 ) ) ;
#27853 = CARTESIAN_POINT ( 'NONE',  ( -21.81686047589429833, -37.90526371014251339, 6.867757412721077870 ) ) ;
#27854 = CARTESIAN_POINT ( 'NONE',  ( 25.65782528836479059, 91.01210296572949687, 66.83837989650099587 ) ) ;
#27855 = ORIENTED_EDGE ( 'NONE', *, *, #23549, .T. ) ;
#27856 = CARTESIAN_POINT ( 'NONE',  ( 10.93730112726005999, 128.3908183996603327, -79.81734490845792607 ) ) ;
#27857 = EDGE_CURVE ( 'NONE', #22381, #28052, #3164, .T. ) ;
#27858 = ORIENTED_EDGE ( 'NONE', *, *, #1361, .T. ) ;
#27859 = ORIENTED_EDGE ( 'NONE', *, *, #25101, .F. ) ;
#27860 = CARTESIAN_POINT ( 'NONE',  ( 2.430230287190581429, -125.2872625092157364, -74.01081053031229828 ) ) ;
#27861 = ADVANCED_FACE ( 'NONE', ( #16476 ), #17450, .F. ) ;
#27862 = ORIENTED_EDGE ( 'NONE', *, *, #21877, .F. ) ;
#27863 =( BOUNDED_SURFACE ( )  B_SPLINE_SURFACE ( 3, 1, ( 
 ( #18247, #11216 ),
 ( #6910, #24472 ),
 ( #13511, #26891 ),
 ( #22306, #15818 ) ),
 .UNSPECIFIED., .F., .F., .F. ) 
 B_SPLINE_SURFACE_WITH_KNOTS ( ( 4, 4 ),
 ( 2, 2 ),
 ( 0.000000000000000000, 1.000000000000000000 ),
 ( 0.000000000000000000, 1.000000000000000000 ),
 .UNSPECIFIED. ) 
 GEOMETRIC_REPRESENTATION_ITEM ( )  RATIONAL_B_SPLINE_SURFACE ( (
 ( 1.000000000000000000, 1.000000000000000000),
 ( 0.6386103224230302855, 0.9954351624131538845),
 ( 0.6386103224230302855, 0.9954351624131538845),
 ( 1.000000000000000000, 1.000000000000000000) ) ) 
 REPRESENTATION_ITEM ( '' )  SURFACE ( )  );
#27864 = ORIENTED_EDGE ( 'NONE', *, *, #11089, .F. ) ;
#27865 = CARTESIAN_POINT ( 'NONE',  ( 9.884929003653626367, -19.90991253123145910, -149.2134106160918066 ) ) ;
#27866 = VERTEX_POINT ( 'NONE', #3238 ) ;
#27867 = DIRECTION ( 'NONE',  ( 0.000000000000000000, 0.000000000000000000, 1.000000000000000000 ) ) ;
#27868 = DIRECTION ( 'NONE',  ( 1.000000000000000000, -6.938893903907226837E-18, 1.734723475976806709E-18 ) ) ;
#27869 = B_SPLINE_CURVE_WITH_KNOTS ( 'NONE', 3,
 ( #17175, #5973, #23539, #25828, #14874, #15005 ),
 .UNSPECIFIED., .F., .F.,
 ( 4, 2, 4 ),
 ( 0.000000000000000000, 0.0004335184443140232147, 0.0008670368886280464295 ),
 .UNSPECIFIED. ) ;
#27870 = CARTESIAN_POINT ( 'NONE',  ( 32.73300124599731475, 117.5726003567930036, -3.836798148479248827 ) ) ;
#27871 = CARTESIAN_POINT ( 'NONE',  ( -9.156249394959713683, -38.89149400288378899, 38.17928057392034447 ) ) ;
#27872 = CARTESIAN_POINT ( 'NONE',  ( 26.11404676487257603, -107.3263591096432776, 36.06104232266415721 ) ) ;
#27873 = CARTESIAN_POINT ( 'NONE',  ( 1.833691583653583423, 0.3559373310815163172, -145.1092556475513220 ) ) ;
#27874 = DIRECTION ( 'NONE',  ( -1.000000000000000000, 6.938893903907227607E-18, -1.734723475976806902E-18 ) ) ;
#27875 = CARTESIAN_POINT ( 'NONE',  ( 10.93730112725996051, -4.928439153519255989, -151.0983828010092793 ) ) ;
#27877 = CARTESIAN_POINT ( 'NONE',  ( 5.340103579038222747, -146.3832392131352833, 17.70136536264617533 ) ) ;
#27876 = CARTESIAN_POINT ( 'NONE',  ( 2.433796855181233454, -118.5671979538051062, -84.34988187691051564 ) ) ;
#27878 = CARTESIAN_POINT ( 'NONE',  ( -20.47566338032517663, -1.586617869344095322, -29.82700953060487592 ) ) ;
#27879 = ORIENTED_EDGE ( 'NONE', *, *, #12637, .T. ) ;
#27880 = ORIENTED_EDGE ( 'NONE', *, *, #10894, .F. ) ;
#27881 = DIRECTION ( 'NONE',  ( 1.000000000000000000, -6.938893903907226837E-18, 1.734723475976806709E-18 ) ) ;
#27882 = CARTESIAN_POINT ( 'NONE',  ( 109.1586059443104944, 0.001198897580738995505, -0.006971743774739763526 ) ) ;
#27883 = ADVANCED_FACE ( 'NONE', ( #12020 ), #28470, .F. ) ;
#27885 = CARTESIAN_POINT ( 'NONE',  ( 2.433796855181233454, 46.34326152018744693, 137.9325382748286870 ) ) ;
#27884 = CARTESIAN_POINT ( 'NONE',  ( -4.162674018437145129, -47.46216648493545875, 11.82104147411610207 ) ) ;
#27886 = CARTESIAN_POINT ( 'NONE',  ( -25.21435515916025594, 1.749597353048488237E-16, -4.373993382621220594E-17 ) ) ;
#27887 = CARTESIAN_POINT ( 'NONE',  ( 26.28373643307413587, -9.189598927292804476, 127.2291519022771524 ) ) ;
#27888 = CARTESIAN_POINT ( 'NONE',  ( -12.82751273423879113, -21.21958768041828947, -44.03362901247000138 ) ) ;
#27889 = DIRECTION ( 'NONE',  ( -1.000000000000000000, 6.938893903907226837E-18, 5.541455922705464902E-20 ) ) ;
#27890 = ORIENTED_EDGE ( 'NONE', *, *, #11022, .F. ) ;
#27891 = CARTESIAN_POINT ( 'NONE',  ( 30.59141879584276325, 99.26511058698885392, 60.43012207290984605 ) ) ;
#27892 = CARTESIAN_POINT ( 'NONE',  ( 1.833485406944057594, -145.1085452359073429, 0.5339064996879626657 ) ) ;
#27893 = CARTESIAN_POINT ( 'NONE',  ( 55.79472521941428198, 71.31192372336674623, 14.41365263906578242 ) ) ;
#27894 = EDGE_CURVE ( 'NONE', #7710, #18844, #25802, .T. ) ;
#27895 = DIRECTION ( 'NONE',  ( -1.000000000000000000, -0.000000000000000000, -0.000000000000000000 ) ) ;
#27896 = CARTESIAN_POINT ( 'NONE',  ( -9.156249394959706578, -38.89149400288433611, -38.17928057391977603 ) ) ;
#27897 = CARTESIAN_POINT ( 'NONE',  ( 1.833485406944057594, 117.7091014914950193, 84.86072343962607079 ) ) ;
#27898 = ORIENTED_EDGE ( 'NONE', *, *, #15143, .T. ) ;
#27899 = CARTESIAN_POINT ( 'NONE',  ( 109.1624594426973260, -0.01570508117119675737, 0.002863932759303782632 ) ) ;
#27900 = CARTESIAN_POINT ( 'NONE',  ( 1.894214914920935744, -137.7482714433626541, 45.75988301372592559 ) ) ;
#27901 = ORIENTED_EDGE ( 'NONE', *, *, #11628, .F. ) ;
#27902 = DIRECTION ( 'NONE',  ( -1.000000000000000000, -0.000000000000000000, -0.000000000000000000 ) ) ;
#27903 = VERTEX_POINT ( 'NONE', #21363 ) ;
#27904 = B_SPLINE_CURVE_WITH_KNOTS ( 'NONE', 3,
 ( #20005, #19865, #22473, #24205, #6926, #2149, #17419, #26763 ),
 .UNSPECIFIED., .F., .F.,
 ( 4, 2, 2, 4 ),
 ( 2.194186273941487696E-16, 0.002761568181852869838, 0.005523136363705520233, 0.01104627272741081495 ),
 .UNSPECIFIED. ) ;
#27905 = LINE ( 'NONE', #14804, #11650 ) ;
#27906 = CARTESIAN_POINT ( 'NONE',  ( -1.048172774974286403, -43.86067135048628529, -13.17853518375281041 ) ) ;
#27907 = CARTESIAN_POINT ( 'NONE',  ( 1.834118845439484335, 144.3336252355298939, -14.99112450600100921 ) ) ;
#27908 = CARTESIAN_POINT ( 'NONE',  ( 109.1586059443104944, -0.001014167950290020132, -0.007001002073869782780 ) ) ;
#27909 = CARTESIAN_POINT ( 'NONE',  ( 10.93730112726003156, 119.3442956573285443, -92.80059208661575099 ) ) ;
#27910 = CARTESIAN_POINT ( 'NONE',  ( -8.786685647604890903, 38.68584556812300690, -37.00619870957947910 ) ) ;
#27911 = CARTESIAN_POINT ( 'NONE',  ( -25.21435515916043713, -23.92354251275954979, -25.00736669481013053 ) ) ;
#27912 = CARTESIAN_POINT ( 'NONE',  ( -1.155031165708883423, 28.62780465193363355, 35.88345263711016031 ) ) ;
#27913 = ORIENTED_EDGE ( 'NONE', *, *, #7800, .T. ) ;
#27914 = ORIENTED_EDGE ( 'NONE', *, *, #7388, .T. ) ;
#27915 = B_SPLINE_CURVE_WITH_KNOTS ( 'NONE', 3,
 ( #4045, #12817, #26066, #8646 ),
 .UNSPECIFIED., .F., .F.,
 ( 4, 4 ),
 ( 5.279490611805676199E-16, 0.008383748772660024398 ),
 .UNSPECIFIED. ) ;
#27916 = CARTESIAN_POINT ( 'NONE',  ( 1.832998868059890096, -15.69902610990276948, -144.2584710144581948 ) ) ;
#27917 = CARTESIAN_POINT ( 'NONE',  ( 26.11404676487257603, 113.2169081140373947, 1.130420376097532653 ) ) ;
#27918 = EDGE_CURVE ( 'NONE', #1343, #28093, #10373, .T. ) ;
#27919 = CARTESIAN_POINT ( 'NONE',  ( -28.13707043255157103, 21.52861750560939313, -7.802116958609079056 ) ) ;
#27920 = CARTESIAN_POINT ( 'NONE',  ( -1.058473599757823180, 12.47539220917862934, -44.07591602137159725 ) ) ;
#27921 = CARTESIAN_POINT ( 'NONE',  ( -1.155031165708874985, 42.97366960678603931, -16.13806347973012834 ) ) ;
#27922 = CARTESIAN_POINT ( 'NONE',  ( -40.00000000000000000, 0.000000000000000000, 0.000000000000000000 ) ) ;
#27923 = CARTESIAN_POINT ( 'NONE',  ( -1.583189561560253589, -44.83405390829680215, -11.94859433442884189 ) ) ;
#27924 = ORIENTED_EDGE ( 'NONE', *, *, #8363, .F. ) ;
#27925 = LINE ( 'NONE', #8223, #1755 ) ;
#27926 = CARTESIAN_POINT ( 'NONE',  ( -1.583189561560256253, 29.24830400313217282, 36.01941156322756399 ) ) ;
#27927 = DIRECTION ( 'NONE',  ( 0.5914120900931445490, 0.8063295922669343474, 0.008020494143004668411 ) ) ;
#27928 = ADVANCED_FACE ( 'NONE', ( #6126 ), #27392, .F. ) ;
#27929 = ADVANCED_FACE ( 'NONE', ( #14879 ), #16388, .F. ) ;
#27930 = DIRECTION ( 'NONE',  ( 0.000000000000000000, -0.000000000000000000, -1.000000000000000000 ) ) ;
#27931 = VERTEX_POINT ( 'NONE', #28385 ) ;
#27932 = CARTESIAN_POINT ( 'NONE',  ( 2.433796855181205476, -144.5536872373190818, -16.65276281464712582 ) ) ;
#27933 = CARTESIAN_POINT ( 'NONE',  ( 25.64681081121879203, -97.57530875170644435, 56.81519825470720519 ) ) ;
#27934 = ORIENTED_EDGE ( 'NONE', *, *, #21518, .T. ) ;
#27935 = ORIENTED_EDGE ( 'NONE', *, *, #10421, .F. ) ;
#27936 = ORIENTED_EDGE ( 'NONE', *, *, #28101, .T. ) ;
#27937 = CARTESIAN_POINT ( 'NONE',  ( -9.156249394959706578, -25.18996226954649131, -48.32878616081000445 ) ) ;
#27938 = ADVANCED_FACE ( 'NONE', ( #21641 ), #21346, .F. ) ;
#27939 = CARTESIAN_POINT ( 'NONE',  ( 2.063896406836609909, -132.1577797566310153, 60.31174178979762246 ) ) ;
#27940 = CARTESIAN_POINT ( 'NONE',  ( 2.063896406836605024, -57.85593781835329708, -133.2511741302126325 ) ) ;
#27941 = ADVANCED_FACE ( 'NONE', ( #8415 ), #13941, .T. ) ;
#27942 = FACE_OUTER_BOUND ( 'NONE', #8579, .T. ) ;
#27943 = ORIENTED_EDGE ( 'NONE', *, *, #18737, .T. ) ;
#27944 = DIRECTION ( 'NONE',  ( 0.000000000000000000, 0.000000000000000000, -1.000000000000000000 ) ) ;
#27945 = B_SPLINE_CURVE_WITH_KNOTS ( 'NONE', 3,
 ( #23822, #19332, #25829, #21218 ),
 .UNSPECIFIED., .F., .F.,
 ( 4, 4 ),
 ( 0.000000000000000000, 0.008383560773332724217 ),
 .UNSPECIFIED. ) ;
#27946 = ORIENTED_EDGE ( 'NONE', *, *, #7300, .T. ) ;
#27947 = CARTESIAN_POINT ( 'NONE',  ( 6.224689322667647851, 2.565137105443750620, 148.0369967195762797 ) ) ;
#27948 = CARTESIAN_POINT ( 'NONE',  ( 26.11404676487259024, 107.3263591096435476, -36.06104232266339693 ) ) ;
#27949 = ADVANCED_FACE ( 'NONE', ( #19482 ), #4602, .F. ) ;
#27950 = CARTESIAN_POINT ( 'NONE',  ( -1.046936909428679119, 45.77873603877006303, -1.275306677858401905 ) ) ;
#27951 = CARTESIAN_POINT ( 'NONE',  ( -1.031422197589716205, 36.13727897780168519, 28.14735071801704436 ) ) ;
#27952 = CARTESIAN_POINT ( 'NONE',  ( 109.1624594426973260, -0.01503296564240493884, -0.005372302061310853770 ) ) ;
#27953 = CARTESIAN_POINT ( 'NONE',  ( 2.430230287190581429, 74.01081053031275303, -125.2872625092154522 ) ) ;
#27954 = CARTESIAN_POINT ( 'NONE',  ( -20.47566262905010248, -10.72601569609877536, 27.87687924095557435 ) ) ;
#27955 = CARTESIAN_POINT ( 'NONE',  ( 5.340103579038286696, 126.5279493327095821, -75.71042924122917839 ) ) ;
#27956 = FACE_OUTER_BOUND ( 'NONE', #23106, .T. ) ;
#27957 = CARTESIAN_POINT ( 'NONE',  ( 32.73300124599739291, -20.69176323058542621, -115.8010721414085538 ) ) ;
#27958 = ORIENTED_EDGE ( 'NONE', *, *, #20876, .T. ) ;
#27959 = CONICAL_SURFACE ( 'NONE', #2657, 117.6351876552689504, 0.9945805576725580410 ) ;
#27960 = VERTEX_POINT ( 'NONE', #22218 ) ;
#27961 = CARTESIAN_POINT ( 'NONE',  ( 5.340103579038161463, 75.71042924123044315, 126.5279493327087152 ) ) ;
#27962 = CARTESIAN_POINT ( 'NONE',  ( -1.046936909428679119, 45.77873603877006303, -1.275306677858401905 ) ) ;
#27963 = ORIENTED_EDGE ( 'NONE', *, *, #20905, .F. ) ;
#27964 = ORIENTED_EDGE ( 'NONE', *, *, #7823, .T. ) ;
#27965 = ORIENTED_EDGE ( 'NONE', *, *, #26528, .F. ) ;
#27966 = CARTESIAN_POINT ( 'NONE',  ( 2.433796855181233454, 43.58222566461826375, -138.8296532063083646 ) ) ;
#27967 = B_SPLINE_CURVE_WITH_KNOTS ( 'NONE', 3,
 ( #10161, #1084, #25560, #18929, #1501, #25421 ),
 .UNSPECIFIED., .F., .F.,
 ( 4, 2, 4 ),
 ( 0.000000000000000000, 0.003570751334075638293, 0.007141502668151276587 ),
 .UNSPECIFIED. ) ;
#27968 = CARTESIAN_POINT ( 'NONE',  ( 1.833485406944043827, -142.0485807715647297, 29.64752363041495542 ) ) ;
#27969 = AXIS2_PLACEMENT_3D ( 'NONE', #10222, #25479, #23029 ) ;
#27970 = EDGE_CURVE ( 'NONE', #3161, #22601, #15850, .T. ) ;
#27971 = CONICAL_SURFACE ( 'NONE', #15547, 117.6351876552689504, 0.9945805576725580410 ) ;
#27972 = CARTESIAN_POINT ( 'NONE',  ( 55.79472521941428198, -72.75035398477136539, 0.7279028900791078005 ) ) ;
#27973 = EDGE_CURVE ( 'NONE', #25128, #5199, #9335, .T. ) ;
#27974 = CARTESIAN_POINT ( 'NONE',  ( 13.36082413113061307, 147.2768864064173329, -41.18148072373461588 ) ) ;
#27975 = CARTESIAN_POINT ( 'NONE',  ( 5.340103556456581302, 144.6887562347053517, -28.39990973639923055 ) ) ;
#27976 = EDGE_CURVE ( 'NONE', #2725, #23109, #392, .T. ) ;
#27977 = CARTESIAN_POINT ( 'NONE',  ( -24.53239521893653929, 30.86654523348686041, 14.09666242510765954 ) ) ;
#27978 = VERTEX_POINT ( 'NONE', #18021 ) ;
#27979 = ORIENTED_EDGE ( 'NONE', *, *, #17979, .F. ) ;
#27981 = CARTESIAN_POINT ( 'NONE',  ( 24.01988960052044675, 36.40943914739906972, 125.8850824254503777 ) ) ;
#27980 = CARTESIAN_POINT ( 'NONE',  ( 1.833485406944043827, 144.3694338680886915, -14.63699153649211127 ) ) ;
#27982 = CARTESIAN_POINT ( 'NONE',  ( 26.11404676487259024, 22.43340081644921113, -110.9778746459744667 ) ) ;
#27983 = CARTESIAN_POINT ( 'NONE',  ( -28.13707043255157103, -22.00298671236744497, -6.342158660426917116 ) ) ;
#27984 = CARTESIAN_POINT ( 'NONE',  ( 2.263178607246701279, 96.24282447295591680, -108.9830946142703567 ) ) ;
#27985 =( BOUNDED_SURFACE ( )  B_SPLINE_SURFACE ( 3, 1, ( 
 ( #1857, #27923 ),
 ( #16862, #8630 ),
 ( #25919, #19563 ),
 ( #10660, #6212 ) ),
 .UNSPECIFIED., .F., .F., .F. ) 
 B_SPLINE_SURFACE_WITH_KNOTS ( ( 4, 4 ),
 ( 2, 2 ),
 ( 0.000000000000000000, 1.000000000000000000 ),
 ( 0.000000000000000000, 1.000000000000000000 ),
 .UNSPECIFIED. ) 
 GEOMETRIC_REPRESENTATION_ITEM ( )  RATIONAL_B_SPLINE_SURFACE ( (
 ( 1.000000000000000000, 1.000000000000000000),
 ( 0.7789835883360576307, 0.9689951854195403280),
 ( 0.7789835883360576307, 0.9689951854195403280),
 ( 1.000000000000000000, 1.000000000000000000) ) ) 
 REPRESENTATION_ITEM ( '' )  SURFACE ( )  );
#27986 = ORIENTED_EDGE ( 'NONE', *, *, #25694, .T. ) ;
#27987 = CARTESIAN_POINT ( 'NONE',  ( 25.64700659047697684, 91.48068002582108704, -66.18331466615464365 ) ) ;
#27988 = CARTESIAN_POINT ( 'NONE',  ( 19.66333377628684431, 95.46107873289045642, -99.30798531455279488 ) ) ;
#27989 = CARTESIAN_POINT ( 'NONE',  ( -1.046935749539997573, -25.87617179820943036, -37.78548154587986119 ) ) ;
#27990 = ORIENTED_EDGE ( 'NONE', *, *, #11157, .F. ) ;
#27991 = ORIENTED_EDGE ( 'NONE', *, *, #12642, .T. ) ;
#27992 = CARTESIAN_POINT ( 'NONE',  ( -25.21435515916025594, 1.749597353048488237E-16, -4.373993382621220594E-17 ) ) ;
#27993 = ORIENTED_EDGE ( 'NONE', *, *, #10633, .T. ) ;
#27994 = ORIENTED_EDGE ( 'NONE', *, *, #17599, .F. ) ;
#27995 = CARTESIAN_POINT ( 'NONE',  ( 21.16825799904898631, 106.9139171613937833, -83.13600836828904050 ) ) ;
#27996 = EDGE_CURVE ( 'NONE', #21108, #23498, #2329, .T. ) ;
#27997 = ORIENTED_EDGE ( 'NONE', *, *, #16647, .T. ) ;
#27998 = CARTESIAN_POINT ( 'NONE',  ( -8.786685647604931759, 47.14957014837394667, 25.35688121747446999 ) ) ;
#27999 = CARTESIAN_POINT ( 'NONE',  ( -20.37983603106073005, 18.69865230096527142, -23.16947629293368038 ) ) ;
#28000 = EDGE_CURVE ( 'NONE', #10778, #15181, #14108, .T. ) ;
#28001 = CARTESIAN_POINT ( 'NONE',  ( -1.049817751779873021, 13.66628317065048392, 43.71287583013712208 ) ) ;
#28002 = CARTESIAN_POINT ( 'NONE',  ( 10.93730112725943471, 133.3192575531795683, 71.28103789254991796 ) ) ;
#28003 = CARTESIAN_POINT ( 'NONE',  ( -55.25719721206881729, 0.009391134844733637840, 0.006045473558784292267 ) ) ;
#28004 = DIRECTION ( 'NONE',  ( -1.000000000000000000, -0.000000000000000000, -0.000000000000000000 ) ) ;
#28005 = EDGE_CURVE ( 'NONE', #7362, #28115, #2797, .T. ) ;
#28007 = DIRECTION ( 'NONE',  ( 0.000000000000000000, 0.000000000000000000, 1.000000000000000000 ) ) ;
#28006 = CARTESIAN_POINT ( 'NONE',  ( -55.24271866751342941, -0.004256484107795216812, 0.008488649505342837909 ) ) ;
#28008 = CARTESIAN_POINT ( 'NONE',  ( 94.22246935314088034, 70.00000000000002842, -6.938893903907228378E-15 ) ) ;
#28009 = ORIENTED_EDGE ( 'NONE', *, *, #15521, .F. ) ;
#28010 = DIRECTION ( 'NONE',  ( -0.7563875759206388771, 0.6320336713238511317, 0.1685564395263317583 ) ) ;
#28011 = B_SPLINE_CURVE_WITH_KNOTS ( 'NONE', 3,
 ( #10636, #28313, #2653, #3876, #22247, #23891, #21427, #1835, #19405, #11297, #21709, #28038, #6457 ),
 .UNSPECIFIED., .F., .F.,
 ( 4, 3, 3, 3, 4 ),
 ( 1.250926888277100303E-17, 0.0007657099931970619711, 0.001531419946797935418, 0.002296279302920161639, 0.003061450627205739884 ),
 .UNSPECIFIED. ) ;
#28012 = CARTESIAN_POINT ( 'NONE',  ( -25.21435515916043713, -23.92354251275918031, 25.00736669481048224 ) ) ;
#28014 = CARTESIAN_POINT ( 'NONE',  ( 10.93730112725971715, 20.69552240458328995, 149.7554878793148703 ) ) ;
#28013 = CARTESIAN_POINT ( 'NONE',  ( 109.1587776205901577, -0.007151389024634725866, -0.001605238040359110302 ) ) ;
#28015 = CARTESIAN_POINT ( 'NONE',  ( 25.87036335909428075, -76.38467849957089584, -83.35447252092937731 ) ) ;
#28016 = CARTESIAN_POINT ( 'NONE',  ( 26.11404676487259024, -90.92995828888244603, 67.46175819463337575 ) ) ;
#28017 = ORIENTED_EDGE ( 'NONE', *, *, #21964, .F. ) ;
#28018 = LINE ( 'NONE', #1815, #6511 ) ;
#28019 = FACE_OUTER_BOUND ( 'NONE', #9031, .T. ) ;
#28020 = ORIENTED_EDGE ( 'NONE', *, *, #7419, .T. ) ;
#28021 = CARTESIAN_POINT ( 'NONE',  ( -55.24271866751342941, -0.006757859501005985571, -0.006671293903669251422 ) ) ;
#28022 =( BOUNDED_SURFACE ( )  B_SPLINE_SURFACE ( 3, 1, ( 
 ( #9616, #12066 ),
 ( #22881, #20841 ),
 ( #25038, #20970 ),
 ( #1125, #18378 ) ),
 .UNSPECIFIED., .F., .F., .F. ) 
 B_SPLINE_SURFACE_WITH_KNOTS ( ( 4, 4 ),
 ( 2, 2 ),
 ( 0.000000000000000000, 1.000000000000000000 ),
 ( 0.000000000000000000, 1.000000000000000000 ),
 .UNSPECIFIED. ) 
 GEOMETRIC_REPRESENTATION_ITEM ( )  RATIONAL_B_SPLINE_SURFACE ( (
 ( 1.000000000000000000, 1.000000000000000000),
 ( 0.9934239774497838349, 0.8357310067453913582),
 ( 0.9934239774497838349, 0.8357310067453913582),
 ( 1.000000000000000000, 1.000000000000000000) ) ) 
 REPRESENTATION_ITEM ( '' )  SURFACE ( )  );
#28023 = CARTESIAN_POINT ( 'NONE',  ( -2.904412668506668016, 25.64203923793632356, 40.16685646686180178 ) ) ;
#28024 = CARTESIAN_POINT ( 'NONE',  ( 109.1586900883932856, -0.007002774699553647453, -0.001385221016527435301 ) ) ;
#28025 = CARTESIAN_POINT ( 'NONE',  ( 1.832998868059858122, -125.9352106559989153, 72.09222286251038270 ) ) ;
#28026 = CARTESIAN_POINT ( 'NONE',  ( -20.24399999263415140, -1.282322917263260198, 29.60996018918694617 ) ) ;
#28027 = VERTEX_POINT ( 'NONE', #19752 ) ;
#28028 = CARTESIAN_POINT ( 'NONE',  ( 2.433796855181219243, -137.9325382748288291, 46.34326152018696376 ) ) ;
#28029 = ORIENTED_EDGE ( 'NONE', *, *, #19278, .F. ) ;
#28030 = CARTESIAN_POINT ( 'NONE',  ( -9.156249394959706578, -9.022661520478157726, -53.74753343182698728 ) ) ;
#28031 = ORIENTED_EDGE ( 'NONE', *, *, #22128, .T. ) ;
#28032 = EDGE_CURVE ( 'NONE', #27179, #12283, #2432, .T. ) ;
#28033 = CARTESIAN_POINT ( 'NONE',  ( -1.259920593601977057, -35.85909937955943860, -28.82601305773640732 ) ) ;
#28034 = EDGE_CURVE ( 'NONE', #8194, #23751, #13444, .T. ) ;
#28035 = B_SPLINE_CURVE_WITH_KNOTS ( 'NONE', 3,
 ( #4391, #6151, #23715, #15034, #2211, #4105, #12871, #6416, #4211, #17029 ),
 .UNSPECIFIED., .F., .F.,
 ( 4, 2, 2, 2, 4 ),
 ( 2.877728285596781101E-16, 0.0003346187017559061659, 0.0006692374035115240425, 0.001003856105267141811, 0.001338474807022759687 ),
 .UNSPECIFIED. ) ;
#28036 = CARTESIAN_POINT ( 'NONE',  ( -20.20612091757416451, -8.058516044219402374, -28.48192249925589792 ) ) ;
#28037 = B_SPLINE_CURVE_WITH_KNOTS ( 'NONE', 3,
 ( #19045, #27821, #8121, #19184, #12692, #21478, #19311 ),
 .UNSPECIFIED., .F., .F.,
 ( 4, 3, 4 ),
 ( 8.673617379884035472E-18, 0.02816610861753243711, 0.04000277880656209761 ),
 .UNSPECIFIED. ) ;
#28038 = CARTESIAN_POINT ( 'NONE',  ( -1.046935749539997129, 36.28605774377803073, 27.93995161054655085 ) ) ;
#28039 = CARTESIAN_POINT ( 'NONE',  ( 10.93730112725983439, -146.7718404940644916, 36.23586118136483236 ) ) ;
#28040 = EDGE_CURVE ( 'NONE', #21976, #8964, #19611, .T. ) ;
#28041 = CARTESIAN_POINT ( 'NONE',  ( 10.93730112725943471, 133.3192575531795683, 71.28103789254991796 ) ) ;
#28042 = CARTESIAN_POINT ( 'NONE',  ( 109.1586059443104944, -0.001921075557427598824, -0.006808232911144234713 ) ) ;
#28043 = CARTESIAN_POINT ( 'NONE',  ( -23.79248802219730052, 16.82188324679482605, -28.61009539422389381 ) ) ;
#28044 = LINE ( 'NONE', #8906, #1889 ) ;
#28045 = CARTESIAN_POINT ( 'NONE',  ( 1.833485406944057594, -58.53321471326971448, 132.7804117027886548 ) ) ;
#28046 = EDGE_CURVE ( 'NONE', #14332, #26638, #7835, .T. ) ;
#28047 = CARTESIAN_POINT ( 'NONE',  ( 109.1592201516379674, -0.007780772729122749191, 0.001127733110588196924 ) ) ;
#28048 = CARTESIAN_POINT ( 'NONE',  ( 109.1778270068192853, -0.007323887274081492156, 0.005755170886745393684 ) ) ;
#28049 = CARTESIAN_POINT ( 'NONE',  ( 25.64708010899963853, 34.83947233573820768, -107.4019003251853235 ) ) ;
#28050 = ORIENTED_EDGE ( 'NONE', *, *, #7030, .F. ) ;
#28051 = VECTOR ( 'NONE', #21762, 1000.000000000000114 ) ;
#28052 = VERTEX_POINT ( 'NONE', #22949 ) ;
#28053 = CARTESIAN_POINT ( 'NONE',  ( -1.259972190295305827, -43.01178231151318698, 16.33417789844418522 ) ) ;
#28054 = LINE ( 'NONE', #14953, #17149 ) ;
#28055 = DIRECTION ( 'NONE',  ( -0.7637818620346800147, -0.6068965246771030886, 0.2198041754873903408 ) ) ;
#28056 = CIRCLE ( 'NONE', #2289, 151.1787379149930359 ) ;
#28057 = DIRECTION ( 'NONE',  ( -0.7563875759206388771, -0.6531865459554678788, 0.03500244528122777032 ) ) ;
#28058 = DIRECTION ( 'NONE',  ( 1.000000000000000000, -6.938893903907226837E-18, 1.734723475976806709E-18 ) ) ;
#28059 = FACE_OUTER_BOUND ( 'NONE', #19498, .T. ) ;
#28060 = CARTESIAN_POINT ( 'NONE',  ( 21.16825799904898986, -51.02216409572659472, 125.4548537968712623 ) ) ;
#28061 = ORIENTED_EDGE ( 'NONE', *, *, #7365, .T. ) ;
#28062 = DIRECTION ( 'NONE',  ( 1.000000000000000000, -6.938893903907226837E-18, 1.734723475976806709E-18 ) ) ;
#28063 = CARTESIAN_POINT ( 'NONE',  ( -55.24198130335446422, 0.004276389980780370345, -0.008252882783649044540 ) ) ;
#28064 = AXIS2_PLACEMENT_3D ( 'NONE', #22906, #7498, #4893 ) ;
#28065 = CARTESIAN_POINT ( 'NONE',  ( 28.37599760073043242, -58.91309773266217320, 98.45181492308101667 ) ) ;
#28066 = EDGE_LOOP ( 'NONE', ( #27537, #1264, #27497, #23456 ) ) ;
#28067 = CARTESIAN_POINT ( 'NONE',  ( -20.57838717382308147, -1.611677988432151709, 29.92853265176832878 ) ) ;
#28068 = CARTESIAN_POINT ( 'NONE',  ( 25.64692232868534560, -12.12735788170734708, -112.2580042965358444 ) ) ;
#28069 = ORIENTED_EDGE ( 'NONE', *, *, #28164, .T. ) ;
#28070 =( BOUNDED_SURFACE ( )  B_SPLINE_SURFACE ( 3, 1, ( 
 ( #5766, #9944 ),
 ( #3310, #14664 ),
 ( #10234, #14524 ),
 ( #14223, #23467 ) ),
 .UNSPECIFIED., .F., .F., .F. ) 
 B_SPLINE_SURFACE_WITH_KNOTS ( ( 4, 4 ),
 ( 2, 2 ),
 ( 0.000000000000000000, 1.000000000000000000 ),
 ( 0.000000000000000000, 1.000000000000000000 ),
 .UNSPECIFIED. ) 
 GEOMETRIC_REPRESENTATION_ITEM ( )  RATIONAL_B_SPLINE_SURFACE ( (
 ( 1.000000000000000000, 1.000000000000000000),
 ( 0.9956975270656954757, 0.8568959468854893125),
 ( 0.9956975270656954757, 0.8568959468854893125),
 ( 1.000000000000000000, 1.000000000000000000) ) ) 
 REPRESENTATION_ITEM ( '' )  SURFACE ( )  );
#28071 = ORIENTED_EDGE ( 'NONE', *, *, #23921, .T. ) ;
#28072 = ORIENTED_EDGE ( 'NONE', *, *, #16617, .T. ) ;
#28073 = AXIS2_PLACEMENT_3D ( 'NONE', #6836, #20055, #17754 ) ;
#28074 = B_SPLINE_CURVE_WITH_KNOTS ( 'NONE', 3,
 ( #19167, #27659, #8107, #5653, #5802, #14559, #6091 ),
 .UNSPECIFIED., .F., .F.,
 ( 4, 3, 4 ),
 ( 4.776383977182116463E-16, 0.02816610861753245099, 0.04000277880656272905 ),
 .UNSPECIFIED. ) ;
#28075 = EDGE_CURVE ( 'NONE', #14894, #25403, #7984, .T. ) ;
#28076 = CARTESIAN_POINT ( 'NONE',  ( -20.47566338032525124, 10.72601609985066062, 27.87687989047296711 ) ) ;
#28077 = CONICAL_SURFACE ( 'NONE', #15654, 117.6351876552689504, 0.9945805576725580410 ) ;
#28078 = EDGE_CURVE ( 'NONE', #11177, #28126, #17224, .T. ) ;
#28079 = PRODUCT_DEFINITION_CONTEXT ( 'detailed design', #21866, 'design' ) ;
#28080 = CARTESIAN_POINT ( 'NONE',  ( 13.36082413113063083, -94.94363694443971724, -119.8836995922736151 ) ) ;
#28081 = EDGE_CURVE ( 'NONE', #11834, #17615, #8316, .T. ) ;
#28082 = CARTESIAN_POINT ( 'NONE',  ( 5.340103579038189885, -43.36842539899472371, 140.9275371836309887 ) ) ;
#28083 = ORIENTED_EDGE ( 'NONE', *, *, #3714, .T. ) ;
#28084 = CARTESIAN_POINT ( 'NONE',  ( 2.430230287190592531, 98.44218333480770866, 107.1617224697467634 ) ) ;
#28085 = LINE ( 'NONE', #27817, #17608 ) ;
#28086 = CARTESIAN_POINT ( 'NONE',  ( -8.259864102781710571, 46.42816643551610412, 25.58601832199028436 ) ) ;
#28087 = CARTESIAN_POINT ( 'NONE',  ( 6.224689322667630975, 129.4863684118297442, -71.79702446228166934 ) ) ;
#28088 = VECTOR ( 'NONE', #1115, 1000.000000000000000 ) ;
#28089 = CONICAL_SURFACE ( 'NONE', #21638, 117.6351876552689504, 0.9945805576725580410 ) ;
#28090 = CARTESIAN_POINT ( 'NONE',  ( -55.25719721206881729, -0.009391134844728631428, 0.006045473558784497832 ) ) ;
#28091 = B_SPLINE_CURVE_WITH_KNOTS ( 'NONE', 3,
 ( #23023, #14203, #7192, #9485, #16527, #27013, #9621, #18104, #2858, #11637 ),
 .UNSPECIFIED., .F., .F.,
 ( 4, 3, 3, 4 ),
 ( 0.000000000000000000, 0.0002669560319015905239, 0.0005492286108966571746, 0.0008315040496093635460 ),
 .UNSPECIFIED. ) ;
#28092 = FACE_OUTER_BOUND ( 'NONE', #7185, .T. ) ;
#28093 = VERTEX_POINT ( 'NONE', #27670 ) ;
#28094 = VECTOR ( 'NONE', #21081, 1000.000000000000000 ) ;
#28095 = VERTEX_POINT ( 'NONE', #24957 ) ;
#28096 = CARTESIAN_POINT ( 'NONE',  ( 25.64681081121880624, -23.88203588908001507, -110.3564950173084185 ) ) ;
#28097 = CARTESIAN_POINT ( 'NONE',  ( 1.833485406944043827, 117.0814567582544612, 85.72460230293732764 ) ) ;
#28098 = ORIENTED_EDGE ( 'NONE', *, *, #2602, .F. ) ;
#28099 = ORIENTED_EDGE ( 'NONE', *, *, #24378, .F. ) ;
#28100 = ORIENTED_EDGE ( 'NONE', *, *, #17130, .F. ) ;
#28101 = EDGE_CURVE ( 'NONE', #10864, #5699, #10710, .T. ) ;
#28102 = EDGE_CURVE ( 'NONE', #3978, #7877, #5662, .T. ) ;
#28103 = CIRCLE ( 'NONE', #19825, 37.50000000000001421 ) ;
#28104 = CARTESIAN_POINT ( 'NONE',  ( 94.22246935314088034, -69.99999999999998579, 12.49999999999999467 ) ) ;
#28105 = EDGE_CURVE ( 'NONE', #2445, #25504, #23370, .T. ) ;
#28106 = AXIS2_PLACEMENT_3D ( 'NONE', #17421, #13111, #6503 ) ;
#28107 = CARTESIAN_POINT ( 'NONE',  ( -55.24198130335446422, 0.006617369590172447053, -0.006527480770973747085 ) ) ;
#28108 = CARTESIAN_POINT ( 'NONE',  ( -20.57838717382308502, 25.16001208503106668, -16.28767523336130196 ) ) ;
#28109 = CARTESIAN_POINT ( 'NONE',  ( -23.77929240705204705, 26.20227034809557054, -25.06639637888430272 ) ) ;
#28110 = APPLICATION_CONTEXT ( 'automotive_design' ) ;
#28111 = CARTESIAN_POINT ( 'NONE',  ( -4.162674018437137136, 45.34593312138912324, 18.33413805792392992 ) ) ;
#28112 = CARTESIAN_POINT ( 'NONE',  ( -55.24271866751342941, -0.006671293903668846365, 0.006757859501006202411 ) ) ;
#28113 = CARTESIAN_POINT ( 'NONE',  ( 2.430230287190592531, -132.3371620660954875, 60.50928654924707928 ) ) ;
#28114 = DIRECTION ( 'NONE',  ( -0.5914120900931443270, -0.7903769105750333424, -0.1598001217819445263 ) ) ;
#28115 = VERTEX_POINT ( 'NONE', #9685 ) ;
#28116 = EDGE_LOOP ( 'NONE', ( #6063, #20634, #14752, #25661 ) ) ;
#28118 = CARTESIAN_POINT ( 'NONE',  ( 25.64681081121880624, -56.81519825470823548, 97.57530875170583329 ) ) ;
#28117 = CARTESIAN_POINT ( 'NONE',  ( -1.259972190295307382, 28.82609802125311660, 35.85909728507018457 ) ) ;
#28119 = CARTESIAN_POINT ( 'NONE',  ( -25.21435515916043713, -6.169479169075696490, -34.05351380035330777 ) ) ;
#28120 = CARTESIAN_POINT ( 'NONE',  ( -28.41354790283022069, 12.60397206714860729, 19.47297445639535596 ) ) ;
#28121 = CARTESIAN_POINT ( 'NONE',  ( -7.078251931573406708, 34.59014398252973166, 38.93060825814192327 ) ) ;
#28122 = ORIENTED_EDGE ( 'NONE', *, *, #28349, .F. ) ;
#28123 = CARTESIAN_POINT ( 'NONE',  ( 2.433796855181219243, 144.5536872373194228, -16.65276281464415575 ) ) ;
#28124 = CARTESIAN_POINT ( 'NONE',  ( -4.178947244162629637, 25.96944194166794162, -41.47292084251642308 ) ) ;
#28125 = CARTESIAN_POINT ( 'NONE',  ( -1.049817751779873909, -36.75003908324312363, -27.33161971822185876 ) ) ;
#28126 = VERTEX_POINT ( 'NONE', #23090 ) ;
#28127 = EDGE_LOOP ( 'NONE', ( #10766, #17636, #568, #6987 ) ) ;
#28128 = CONICAL_SURFACE ( 'NONE', #7962, 117.6351876552689504, 0.9945805576725580410 ) ;
#28129 = EDGE_CURVE ( 'NONE', #309, #10148, #14770, .T. ) ;
#28130 = ORIENTED_EDGE ( 'NONE', *, *, #12677, .F. ) ;
#28131 = AXIS2_PLACEMENT_3D ( 'NONE', #28223, #8657, #4468 ) ;
#28132 = VERTEX_POINT ( 'NONE', #7545 ) ;
#28133 = B_SPLINE_CURVE_WITH_KNOTS ( 'NONE', 3,
 ( #3637, #23386, #22962, #1340 ),
 .UNSPECIFIED., .F., .F.,
 ( 4, 4 ),
 ( 1.386477127738322940E-16, 0.008383748772659576839 ),
 .UNSPECIFIED. ) ;
#28134 = EDGE_CURVE ( 'NONE', #26877, #18004, #18917, .T. ) ;
#28135 = EDGE_CURVE ( 'NONE', #14412, #23015, #10007, .T. ) ;
#28136 = CARTESIAN_POINT ( 'NONE',  ( 2.108985857320888169, -86.43462668039059338, -116.7869613039528929 ) ) ;
#28137 = VERTEX_POINT ( 'NONE', #25239 ) ;
#28138 =( BOUNDED_SURFACE ( )  B_SPLINE_SURFACE ( 3, 1, ( 
 ( #5143, #15632 ),
 ( #18229, #2699 ),
 ( #395, #24452 ),
 ( #15800, #4719 ) ),
 .UNSPECIFIED., .F., .F., .F. ) 
 B_SPLINE_SURFACE_WITH_KNOTS ( ( 4, 4 ),
 ( 2, 2 ),
 ( 0.000000000000000000, 1.000000000000000000 ),
 ( 0.000000000000000000, 1.000000000000000000 ),
 .UNSPECIFIED. ) 
 GEOMETRIC_REPRESENTATION_ITEM ( )  RATIONAL_B_SPLINE_SURFACE ( (
 ( 1.000000000000000000, 1.000000000000000000),
 ( 0.7789835883360576307, 0.9689951854195403280),
 ( 0.7789835883360576307, 0.9689951854195403280),
 ( 1.000000000000000000, 1.000000000000000000) ) ) 
 REPRESENTATION_ITEM ( '' )  SURFACE ( )  );
#28139 = CARTESIAN_POINT ( 'NONE',  ( 28.37644542392837010, 120.7150203538609645, 29.80435743553996275 ) ) ;
#28140 = CARTESIAN_POINT ( 'NONE',  ( 109.1624594426973118, -0.01551217196237748668, 0.003771499231554245168 ) ) ;
#28141 = CARTESIAN_POINT ( 'NONE',  ( -55.24300891470648622, -0.008142823778061756071, 0.005486913146696262289 ) ) ;
#28142 = CARTESIAN_POINT ( 'NONE',  ( 2.433796855181219243, 144.5536872373194228, -16.65276281464415575 ) ) ;
#28143 = CARTESIAN_POINT ( 'NONE',  ( 24.01988960052062438, -4.273195451969565184, 130.9749633972837159 ) ) ;
#28145 =( BOUNDED_SURFACE ( )  B_SPLINE_SURFACE ( 3, 1, ( 
 ( #1128, #21113 ),
 ( #3143, #23441 ),
 ( #5590, #14201 ),
 ( #14502, #3429 ) ),
 .UNSPECIFIED., .F., .F., .F. ) 
 B_SPLINE_SURFACE_WITH_KNOTS ( ( 4, 4 ),
 ( 2, 2 ),
 ( 0.000000000000000000, 1.000000000000000000 ),
 ( 0.000000000000000000, 1.000000000000000000 ),
 .UNSPECIFIED. ) 
 GEOMETRIC_REPRESENTATION_ITEM ( )  RATIONAL_B_SPLINE_SURFACE ( (
 ( 1.000000000000000000, 1.000000000000000000),
 ( 0.9934239774497838349, 0.8357310067453913582),
 ( 0.9934239774497838349, 0.8357310067453913582),
 ( 1.000000000000000000, 1.000000000000000000) ) ) 
 REPRESENTATION_ITEM ( '' )  SURFACE ( )  );
#28144 = CIRCLE ( 'NONE', #7029, 117.6351876552689504 ) ;
#28146 = DIRECTION ( 'NONE',  ( 0.000000000000000000, 0.000000000000000000, 1.000000000000000000 ) ) ;
#28147 = CARTESIAN_POINT ( 'NONE',  ( 2.263178113027034755, -118.4461880110609115, 84.32376073259185034 ) ) ;
#28148 = CARTESIAN_POINT ( 'NONE',  ( -20.21097721650787804, 23.76068422213757714, -17.67178726257366606 ) ) ;
#28149 = VERTEX_POINT ( 'NONE', #5506 ) ;
#28150 = VERTEX_POINT ( 'NONE', #14269 ) ;
#28151 = CARTESIAN_POINT ( 'NONE',  ( 25.64681081121879203, 56.81519825470891760, -97.57530875170544959 ) ) ;
#28152 = CARTESIAN_POINT ( 'NONE',  ( 1.894214914920984372, 117.9869255019031868, 84.54370816135612188 ) ) ;
#28154 = CARTESIAN_POINT ( 'NONE',  ( 30.58324630866335880, 16.55818995381147829, 119.8048187378265652 ) ) ;
#28153 = CARTESIAN_POINT ( 'NONE',  ( -1.619063947482201282, -44.80407745103776307, 11.94059994246206635 ) ) ;
#28155 = CARTESIAN_POINT ( 'NONE',  ( -1.619063947482197729, -43.26576862488421682, 16.67502769180607203 ) ) ;
#28156 = CARTESIAN_POINT ( 'NONE',  ( 25.87036335909427720, -90.88222105969110487, 67.25332031939115041 ) ) ;
#28157 = CARTESIAN_POINT ( 'NONE',  ( 1.833485406944043827, -97.49333871408762775, 107.4794113447406119 ) ) ;
#28158 = ORIENTED_EDGE ( 'NONE', *, *, #14661, .T. ) ;
#28159 = CARTESIAN_POINT ( 'NONE',  ( 10.93730112725994275, -26.59437931460641025, -148.8212007290665042 ) ) ;
#28160 = EDGE_CURVE ( 'NONE', #22027, #11495, #18179, .T. ) ;
#28161 = DIRECTION ( 'NONE',  ( -1.000000000000000000, -0.000000000000000000, -0.000000000000000000 ) ) ;
#28162 = CARTESIAN_POINT ( 'NONE',  ( -8.259864102781676820, 36.24929574824966494, 38.68084189741909995 ) ) ;
#28163 = EDGE_LOOP ( 'NONE', ( #17653, #3385, #6736, #14616 ) ) ;
#28164 = EDGE_CURVE ( 'NONE', #16763, #21239, #10665, .T. ) ;
#28165 = EDGE_CURVE ( 'NONE', #9286, #2734, #15788, .T. ) ;
#28166 = VECTOR ( 'NONE', #18399, 999.9999999999998863 ) ;
#28167 = FACE_OUTER_BOUND ( 'NONE', #26005, .T. ) ;
#28168 = VECTOR ( 'NONE', #11734, 1000.000000000000000 ) ;
#28169 = ORIENTED_EDGE ( 'NONE', *, *, #21877, .T. ) ;
#28170 = CARTESIAN_POINT ( 'NONE',  ( 2.263178607246715490, -28.85718361841014712, 142.5035407554793210 ) ) ;
#28171 = VECTOR ( 'NONE', #24461, 1000.000000000000114 ) ;
#28172 = CARTESIAN_POINT ( 'NONE',  ( 109.1721716018069657, 0.01467989464939309721, -0.008708654716139472077 ) ) ;
#28173 = CARTESIAN_POINT ( 'NONE',  ( 109.1589550718174877, 0.002126635388725465863, 0.007270618150629040016 ) ) ;
#28175 = B_SPLINE_CURVE_WITH_KNOTS ( 'NONE', 3,
 ( #3582, #1424, #10232, #27477 ),
 .UNSPECIFIED., .F., .F.,
 ( 4, 4 ),
 ( 0.000000000000000000, 0.008383560773332722482 ),
 .UNSPECIFIED. ) ;
#28174 = CARTESIAN_POINT ( 'NONE',  ( 25.64708228042119842, 97.76433875577640720, 56.48974615488955919 ) ) ;
#28176 = CARTESIAN_POINT ( 'NONE',  ( 1.833485406944043827, 125.4007332306545379, 73.01664920993009389 ) ) ;
#28177 = CARTESIAN_POINT ( 'NONE',  ( 25.64681081121879203, 56.09509703373481670, -97.99105938547863559 ) ) ;
#28178 = CARTESIAN_POINT ( 'NONE',  ( -12.82751273423883198, -35.32125660155422509, 33.78816682541326344 ) ) ;
#28179 = CARTESIAN_POINT ( 'NONE',  ( -55.24271866751342941, 0.009369360294294836952, -0.001545935011626992572 ) ) ;
#28180 = LINE ( 'NONE', #15213, #8327 ) ;
#28181 = CARTESIAN_POINT ( 'NONE',  ( 1.833750490713712322, -132.6726660571947889, 58.77746103890230955 ) ) ;
#28182 = LINE ( 'NONE', #24168, #24014 ) ;
#28183 = CARTESIAN_POINT ( 'NONE',  ( -25.21435515916043357, -6.169479169075226643, 34.05351380035340014 ) ) ;
#28184 = DIRECTION ( 'NONE',  ( 0.7637818620346800147, -0.6068965246771045319, -0.2198041754873859832 ) ) ;
#28185 = CARTESIAN_POINT ( 'NONE',  ( -1.155001620486255209, -45.85729774065936937, -2.068551059060163677 ) ) ;
#28186 = VERTEX_POINT ( 'NONE', #19040 ) ;
#28187 =( BOUNDED_SURFACE ( )  B_SPLINE_SURFACE ( 3, 1, ( 
 ( #8868, #79 ),
 ( #4393, #24268 ),
 ( #15171, #17207 ),
 ( #13165, #2076 ) ),
 .UNSPECIFIED., .F., .F., .F. ) 
 B_SPLINE_SURFACE_WITH_KNOTS ( ( 4, 4 ),
 ( 2, 2 ),
 ( 0.000000000000000000, 1.000000000000000000 ),
 ( 0.000000000000000000, 1.000000000000000000 ),
 .UNSPECIFIED. ) 
 GEOMETRIC_REPRESENTATION_ITEM ( )  RATIONAL_B_SPLINE_SURFACE ( (
 ( 1.000000000000000000, 1.000000000000000000),
 ( 0.9956975270656954757, 0.8568959468854893125),
 ( 0.9956975270656954757, 0.8568959468854893125),
 ( 1.000000000000000000, 1.000000000000000000) ) ) 
 REPRESENTATION_ITEM ( '' )  SURFACE ( )  );
#28188 = ORIENTED_EDGE ( 'NONE', *, *, #7108, .F. ) ;
#28189 = ORIENTED_EDGE ( 'NONE', *, *, #4888, .F. ) ;
#28190 = CARTESIAN_POINT ( 'NONE',  ( 26.11404676487257603, -97.48350837663569735, -57.58742681967552102 ) ) ;
#28191 = CARTESIAN_POINT ( 'NONE',  ( -1.259972190295300054, 16.33417789844434509, 43.01178231151312303 ) ) ;
#28192 = CARTESIAN_POINT ( 'NONE',  ( -2.265401668238146371, -29.73100299756539755, 36.42007794497283157 ) ) ;
#28193 = CARTESIAN_POINT ( 'NONE',  ( 109.1592201516379674, 0.007302213399779926284, -0.002913740842108661615 ) ) ;
#28194 = DIRECTION ( 'NONE',  ( 0.000000000000000000, 5.223019709707975211E-21, -1.000000000000000000 ) ) ;
#28195 = PRODUCT_DEFINITION_FORMATION_WITH_SPECIFIED_SOURCE ( 'ANY', '', #16651, .NOT_KNOWN. ) ;
#28196 = CARTESIAN_POINT ( 'NONE',  ( 109.1586900883932856, -0.005833932871487544462, 0.004113747441000897322 ) ) ;
#28197 = CARTESIAN_POINT ( 'NONE',  ( 1.832998868059858122, -0.5339089137737902391, -145.1092030902949830 ) ) ;
#28198 = VERTEX_POINT ( 'NONE', #8526 ) ;
#28199 = CARTESIAN_POINT ( 'NONE',  ( -20.57838717382308147, -23.26537097894090778, 18.89542499756525729 ) ) ;
#28200 = CARTESIAN_POINT ( 'NONE',  ( 1.833485406944043827, -145.1085452359073145, -0.5339064996899981486 ) ) ;
#28201 = VECTOR ( 'NONE', #2711, 1000.000000000000000 ) ;
#28202 = CARTESIAN_POINT ( 'NONE',  ( 25.64704443564080805, 23.60610532597107181, -110.4160069635930626 ) ) ;
#28203 = EDGE_CURVE ( 'NONE', #13865, #11082, #23635, .T. ) ;
#28204 = EDGE_CURVE ( 'NONE', #17409, #19804, #18055, .T. ) ;
#28205 = CARTESIAN_POINT ( 'NONE',  ( -20.38016308990358638, -28.74660391518349911, -7.753479680700832155 ) ) ;
#28206 = B_SPLINE_CURVE_WITH_KNOTS ( 'NONE', 3,
 ( #19124, #8469, #23747, #15055, #25885, #14795, #12763, #15196 ),
 .UNSPECIFIED., .F., .F.,
 ( 4, 2, 2, 4 ),
 ( 6.938893903907228378E-18, 0.0002429592666046707157, 0.0004859185332093344926, 0.0009718370664186905608 ),
 .UNSPECIFIED. ) ;
#28207 = ORIENTED_EDGE ( 'NONE', *, *, #5392, .F. ) ;
#28209 = ADVANCED_FACE ( 'NONE', ( #5812 ), #25401, .F. ) ;
#28208 = CARTESIAN_POINT ( 'NONE',  ( -4.780792508754314163, 32.07473752860781246, -37.74278713234406979 ) ) ;
#28210 = CARTESIAN_POINT ( 'NONE',  ( -7.711401346138398338, -10.36923727626085423, 51.42722225669433556 ) ) ;
#28211 = VERTEX_POINT ( 'NONE', #17288 ) ;
#28212 = EDGE_CURVE ( 'NONE', #8318, #24769, #28085, .T. ) ;
#28213 = ORIENTED_EDGE ( 'NONE', *, *, #6738, .F. ) ;
#28214 = ORIENTED_EDGE ( 'NONE', *, *, #24916, .F. ) ;
#28215 = DIRECTION ( 'NONE',  ( 0.000000000000000000, 5.223019709707975211E-21, -1.000000000000000000 ) ) ;
#28216 = CARTESIAN_POINT ( 'NONE',  ( -1.056502255334265339, -36.75727364034752043, -27.33667001641156702 ) ) ;
#28217 = CARTESIAN_POINT ( 'NONE',  ( 2.430230287190592531, -1.451610819316726975, -145.5073573687467103 ) ) ;
#28218 = ORIENTED_EDGE ( 'NONE', *, *, #14754, .T. ) ;
#28219 = B_SPLINE_CURVE_WITH_KNOTS ( 'NONE', 3,
 ( #23710, #3826, #18797, #23279, #5716, #7741, #14326, #8157 ),
 .UNSPECIFIED., .F., .F.,
 ( 4, 2, 2, 4 ),
 ( 0.000000000000000000, 0.002761524886576652380, 0.005523049773153304760, 0.01104609954630660952 ),
 .UNSPECIFIED. ) ;
#28220 = CARTESIAN_POINT ( 'NONE',  ( 26.11404676487257603, 92.25884714080498838, -65.63269960453146723 ) ) ;
#28221 = CARTESIAN_POINT ( 'NONE',  ( -1.583189561560256253, -29.24830400313190637, -36.01941156322777715 ) ) ;
#28222 = CARTESIAN_POINT ( 'NONE',  ( -1.031422197589716205, -15.60268798220668174, -43.06660437151303711 ) ) ;
#28223 = CARTESIAN_POINT ( 'NONE',  ( 32.73300124599732186, 0.000000000000000000, 0.000000000000000000 ) ) ;
#28224 = CARTESIAN_POINT ( 'NONE',  ( 109.1586900883932856, -0.007109207791181747921, 0.0006456433529163218155 ) ) ;
#28225 = CARTESIAN_POINT ( 'NONE',  ( -20.90916690077960638, 7.054312691028996163, -38.93431874629079203 ) ) ;
#28226 = CARTESIAN_POINT ( 'NONE',  ( -1.583189561560255143, 36.01941156322830295, 29.24830400313125267 ) ) ;
#28227 = EDGE_CURVE ( 'NONE', #20045, #26004, #4112, .T. ) ;
#28228 = CARTESIAN_POINT ( 'NONE',  ( -25.21435515916043713, -4.655591116594118617, 34.29329011225960500 ) ) ;
#28229 = CARTESIAN_POINT ( 'NONE',  ( 109.1586900883932856, -0.002301750759607945531, -0.006757191295056121962 ) ) ;
#28230 =( BOUNDED_SURFACE ( )  B_SPLINE_SURFACE ( 3, 1, ( 
 ( #22022, #25935 ),
 ( #19583, #6354 ),
 ( #13232, #24066 ),
 ( #13105, #2284 ) ),
 .UNSPECIFIED., .F., .F., .F. ) 
 B_SPLINE_SURFACE_WITH_KNOTS ( ( 4, 4 ),
 ( 2, 2 ),
 ( 0.000000000000000000, 1.000000000000000000 ),
 ( 0.000000000000000000, 1.000000000000000000 ),
 .UNSPECIFIED. ) 
 GEOMETRIC_REPRESENTATION_ITEM ( )  RATIONAL_B_SPLINE_SURFACE ( (
 ( 1.000000000000000000, 1.000000000000000000),
 ( 0.6386103224230302855, 0.9954351624131538845),
 ( 0.6386103224230302855, 0.9954351624131538845),
 ( 1.000000000000000000, 1.000000000000000000) ) ) 
 REPRESENTATION_ITEM ( '' )  SURFACE ( )  );
#28231 = CARTESIAN_POINT ( 'NONE',  ( 9.884929003653608603, -146.3148513795964334, -35.39789245780480087 ) ) ;
#28232 = EDGE_LOOP ( 'NONE', ( #4252, #16604, #18282, #15449 ) ) ;
#28233 = ORIENTED_EDGE ( 'NONE', *, *, #10002, .F. ) ;
#28235 = EDGE_CURVE ( 'NONE', #26786, #20356, #25458, .T. ) ;
#28234 = CARTESIAN_POINT ( 'NONE',  ( -4.178947244162641184, -48.81675275154074001, 3.367451375481625320 ) ) ;
#28236 = CARTESIAN_POINT ( 'NONE',  ( 25.81918753295377300, 35.81374485821615394, 107.2019194967336801 ) ) ;
#28237 = ORIENTED_EDGE ( 'NONE', *, *, #2285, .F. ) ;
#28238 = EDGE_LOOP ( 'NONE', ( #15092, #23233, #21997, #4350 ) ) ;
#28239 = ORIENTED_EDGE ( 'NONE', *, *, #2134, .T. ) ;
#28240 = B_SPLINE_CURVE_WITH_KNOTS ( 'NONE', 3,
 ( #10089, #19142, #617, #12369, #16975, #25766, #27630, #21149, #25501, #8083 ),
 .UNSPECIFIED., .F., .F.,
 ( 4, 3, 3, 4 ),
 ( 6.938893903907228378E-18, 0.0002669560319015735019, 0.0005492286108966399358, 0.0008315040496093465240 ),
 .UNSPECIFIED. ) ;
#28241 = B_SPLINE_CURVE_WITH_KNOTS ( 'NONE', 3,
 ( #15368, #21867, #11065, #4021, #15224, #12935 ),
 .UNSPECIFIED., .F., .F.,
 ( 4, 2, 4 ),
 ( 4.982613841084487634E-18, 0.0004335151646191476174, 0.0008670303292382917654 ),
 .UNSPECIFIED. ) ;
#28242 = CARTESIAN_POINT ( 'NONE',  ( -1.619063947482194177, 25.20140673341374438, -38.92136151114915066 ) ) ;
#28243 = CARTESIAN_POINT ( 'NONE',  ( 119.2224693531408803, 70.00000000000004263, 19.99999999999997513 ) ) ;
#28244 = CARTESIAN_POINT ( 'NONE',  ( -25.21435515916043002, -4.655591116594591128, -34.29329011225954105 ) ) ;
#28245 = CARTESIAN_POINT ( 'NONE',  ( 25.64704443564076186, -110.4715096490034654, 23.34498572103285241 ) ) ;
#28246 = CARTESIAN_POINT ( 'NONE',  ( -21.41427618760457818, 28.68857606049983744, 11.22988868156155640 ) ) ;
#28247 = CARTESIAN_POINT ( 'NONE',  ( -25.21435515916043002, 4.655591116594353984, -34.29329011225956947 ) ) ;
#28248 = EDGE_LOOP ( 'NONE', ( #23943, #11688, #14213, #3080 ) ) ;
#28249 = ORIENTED_EDGE ( 'NONE', *, *, #26157, .F. ) ;
#28250 = B_SPLINE_CURVE_WITH_KNOTS ( 'NONE', 3,
 ( #4139, #25757, #2243, #10631 ),
 .UNSPECIFIED., .F., .F.,
 ( 4, 4 ),
 ( 0.000000000000000000, 0.008383560773332725952 ),
 .UNSPECIFIED. ) ;
#28251 = CARTESIAN_POINT ( 'NONE',  ( 25.70243777736190793, -57.10783651465036570, 97.44734253939064672 ) ) ;
#28252 = ADVANCED_FACE ( 'NONE', ( #5906 ), #19317, .F. ) ;
#28253 = CARTESIAN_POINT ( 'NONE',  ( -55.24390624410018802, 0.001811362924362862900, -0.01027195578988028025 ) ) ;
#28254 = CARTESIAN_POINT ( 'NONE',  ( -55.24271866751342941, 0.004256484107795918508, -0.008488649505343059953 ) ) ;
#28255 = CARTESIAN_POINT ( 'NONE',  ( 109.1592201516379674, -0.004368284148525305825, 0.006536841731961986514 ) ) ;
#28256 = LINE ( 'NONE', #15019, #21547 ) ;
#28257 = EDGE_LOOP ( 'NONE', ( #16464, #12393, #9098, #19107 ) ) ;
#28258 = CARTESIAN_POINT ( 'NONE',  ( -2.265401668238151256, -2.645701981445478079, 46.93990709177546705 ) ) ;
#28259 =( BOUNDED_SURFACE ( )  B_SPLINE_SURFACE ( 3, 1, ( 
 ( #22749, #3014 ),
 ( #1555, #1137 ),
 ( #5448, #25322 ),
 ( #3569, #10359 ) ),
 .UNSPECIFIED., .F., .F., .F. ) 
 B_SPLINE_SURFACE_WITH_KNOTS ( ( 4, 4 ),
 ( 2, 2 ),
 ( 0.000000000000000000, 1.000000000000000000 ),
 ( 0.000000000000000000, 1.000000000000000000 ),
 .UNSPECIFIED. ) 
 GEOMETRIC_REPRESENTATION_ITEM ( )  RATIONAL_B_SPLINE_SURFACE ( (
 ( 1.000000000000000000, 1.000000000000000000),
 ( 0.9960225298536222738, 0.9999952330161893110),
 ( 0.9960225298536222738, 0.9999952330161893110),
 ( 1.000000000000000000, 1.000000000000000000) ) ) 
 REPRESENTATION_ITEM ( '' )  SURFACE ( )  );
#28261 = EDGE_CURVE ( 'NONE', #4663, #1581, #21755, .T. ) ;
#28260 = CARTESIAN_POINT ( 'NONE',  ( -28.13707043255157103, -12.83104814250467562, -18.96624908365841478 ) ) ;
#28262 = CARTESIAN_POINT ( 'NONE',  ( 30.58324630866338723, -83.81536267638887239, -87.19147450740442196 ) ) ;
#28263 = VERTEX_POINT ( 'NONE', #22903 ) ;
#28264 = ORIENTED_EDGE ( 'NONE', *, *, #13405, .F. ) ;
#28265 = B_SPLINE_CURVE_WITH_KNOTS ( 'NONE', 3,
 ( #27088, #1059, #26664, #15731, #22516, #24544 ),
 .UNSPECIFIED., .F., .F.,
 ( 4, 2, 4 ),
 ( 6.505213034913026604E-19, 0.0004335151646191484848, 0.0008670303292382963191 ),
 .UNSPECIFIED. ) ;
#28266 = EDGE_CURVE ( 'NONE', #22518, #2726, #19927, .T. ) ;
#28267 = DIRECTION ( 'NONE',  ( 0.000000000000000000, -1.000000000000000000, 0.000000000000000000 ) ) ;
#28268 = ORIENTED_EDGE ( 'NONE', *, *, #27579, .T. ) ;
#28269 = LINE ( 'NONE', #23984, #27650 ) ;
#28270 = ORIENTED_EDGE ( 'NONE', *, *, #19395, .F. ) ;
#28271 = CARTESIAN_POINT ( 'NONE',  ( 1.832998868059858122, -138.1720401012269974, 44.33343224355186862 ) ) ;
#28272 = ORIENTED_EDGE ( 'NONE', *, *, #9006, .T. ) ;
#28273 = CARTESIAN_POINT ( 'NONE',  ( -1.239374126674604337, 16.50008610789360119, 42.99367564261261521 ) ) ;
#28274 = ADVANCED_FACE ( 'NONE', ( #1002 ), #28302, .F. ) ;
#28275 = CARTESIAN_POINT ( 'NONE',  ( -21.41427618760458174, -11.22988868156165410, 28.68857606049978415 ) ) ;
#28276 = FACE_OUTER_BOUND ( 'NONE', #22848, .T. ) ;
#28277 = CARTESIAN_POINT ( 'NONE',  ( -16.86833981943428640, -38.94907963570735632, -20.94590537750593739 ) ) ;
#28278 = CARTESIAN_POINT ( 'NONE',  ( 109.1721716018069657, 0.001984900887706629938, 0.01695288006057377519 ) ) ;
#28279 = CARTESIAN_POINT ( 'NONE',  ( 26.11404676487257603, 45.01677474591409833, 103.8885755249570906 ) ) ;
#28280 = EDGE_CURVE ( 'NONE', #22329, #23985, #28175, .T. ) ;
#28281 = CARTESIAN_POINT ( 'NONE',  ( 30.59141879584321089, 111.3296561588019387, -33.33270905817467167 ) ) ;
#28283 = CARTESIAN_POINT ( 'NONE',  ( -1.464342487929856995, 46.14921266389555399, -2.431462367721493045 ) ) ;
#28282 = CARTESIAN_POINT ( 'NONE',  ( 109.1586900883932856, 0.002109621908824146474, 0.006819617742892447251 ) ) ;
#28284 = CARTESIAN_POINT ( 'NONE',  ( 26.11404676487259024, 55.62948129436384193, -98.61392875273304526 ) ) ;
#28285 = ORIENTED_EDGE ( 'NONE', *, *, #27807, .F. ) ;
#28286 = ORIENTED_EDGE ( 'NONE', *, *, #13025, .F. ) ;
#28287 = LINE ( 'NONE', #17637, #10625 ) ;
#28288 = CARTESIAN_POINT ( 'NONE',  ( 1.833485406944057594, 117.7091014914950193, 84.86072343962607079 ) ) ;
#28289 = DIRECTION ( 'NONE',  ( 0.000000000000000000, 0.000000000000000000, -1.000000000000000000 ) ) ;
#28290 = EDGE_CURVE ( 'NONE', #11098, #12613, #27617, .T. ) ;
#28291 = CARTESIAN_POINT ( 'NONE',  ( -2.911734481061399205, -44.38410240830292963, 17.36785190846027049 ) ) ;
#28292 = CARTESIAN_POINT ( 'NONE',  ( -8.786685647604890903, 7.199674155858966529, -53.04920435127184675 ) ) ;
#28293 = CARTESIAN_POINT ( 'NONE',  ( 1.833485406944071361, 29.64752363041738548, -142.0485807715643034 ) ) ;
#28294 = ORIENTED_EDGE ( 'NONE', *, *, #20336, .F. ) ;
#28295 = CARTESIAN_POINT ( 'NONE',  ( 2.263178113027034755, -107.1074314657337396, -98.32595894905942657 ) ) ;
#28296 = CARTESIAN_POINT ( 'NONE',  ( 1.831572820252008738, 31.13525033585688462, -141.7320553118902922 ) ) ;
#28297 = DIRECTION ( 'NONE',  ( 0.000000000000000000, 0.000000000000000000, -1.000000000000000000 ) ) ;
#28298 = CARTESIAN_POINT ( 'NONE',  ( -24.53237795827023859, -33.71192251888856362, 3.868415699416008380 ) ) ;
#28299 = CARTESIAN_POINT ( 'NONE',  ( -9.156249394959706578, 9.022661520478530761, 53.74753343182691623 ) ) ;
#28300 = VERTEX_POINT ( 'NONE', #16401 ) ;
#28301 = CARTESIAN_POINT ( 'NONE',  ( -20.20700224038492721, 29.58392382092673500, -0.9908225410479557516 ) ) ;
#28302 =( BOUNDED_SURFACE ( )  B_SPLINE_SURFACE ( 3, 1, ( 
 ( #3448, #18706 ),
 ( #18405, #23330 ),
 ( #23193, #16701 ),
 ( #27182, #7647 ) ),
 .UNSPECIFIED., .F., .F., .F. ) 
 B_SPLINE_SURFACE_WITH_KNOTS ( ( 4, 4 ),
 ( 2, 2 ),
 ( 0.000000000000000000, 1.000000000000000000 ),
 ( 0.000000000000000000, 1.000000000000000000 ),
 .UNSPECIFIED. ) 
 GEOMETRIC_REPRESENTATION_ITEM ( )  RATIONAL_B_SPLINE_SURFACE ( (
 ( 1.000000000000000000, 1.000000000000000000),
 ( 0.6386103224230302855, 0.9954351624131538845),
 ( 0.6386103224230302855, 0.9954351624131538845),
 ( 1.000000000000000000, 1.000000000000000000) ) ) 
 REPRESENTATION_ITEM ( '' )  SURFACE ( )  );
#28303 = DIRECTION ( 'NONE',  ( 0.000000000000000000, 5.223019709708233256E-21, -1.000000000000000000 ) ) ;
#28304 = ORIENTED_EDGE ( 'NONE', *, *, #96, .T. ) ;
#28305 = DIRECTION ( 'NONE',  ( 0.7071067811865465735, 0.000000000000000000, -0.7071067811865485719 ) ) ;
#28306 = EDGE_LOOP ( 'NONE', ( #8586, #5516, #6230, #1396 ) ) ;
#28307 = CARTESIAN_POINT ( 'NONE',  ( -12.94347594948482794, -6.555928820868979656, 48.30328466416770539 ) ) ;
#28308 = CARTESIAN_POINT ( 'NONE',  ( 1.832998868059858122, -97.49378069860723883, -107.4798986104869982 ) ) ;
#28309 = VERTEX_POINT ( 'NONE', #7495 ) ;
#28310 = B_SPLINE_CURVE_WITH_KNOTS ( 'NONE', 3,
 ( #5690, #927, #14302, #3235, #12162, #5535, #25556, #12016 ),
 .UNSPECIFIED., .F., .F.,
 ( 4, 2, 2, 4 ),
 ( 0.000000000000000000, 0.0002429588503611233006, 0.0004859177007222466012, 0.0009718354014444932024 ),
 .UNSPECIFIED. ) ;
#28311 = CARTESIAN_POINT ( 'NONE',  ( 25.64703792032469210, 97.85829113439956473, 56.32669596053470684 ) ) ;
#28312 =( BOUNDED_SURFACE ( )  B_SPLINE_SURFACE ( 3, 1, ( 
 ( #28254, #21798 ),
 ( #15574, #15149 ),
 ( #17606, #2488 ),
 ( #4659, #2339 ) ),
 .UNSPECIFIED., .F., .F., .F. ) 
 B_SPLINE_SURFACE_WITH_KNOTS ( ( 4, 4 ),
 ( 2, 2 ),
 ( 0.000000000000000000, 1.000000000000000000 ),
 ( 0.000000000000000000, 1.000000000000000000 ),
 .UNSPECIFIED. ) 
 GEOMETRIC_REPRESENTATION_ITEM ( )  RATIONAL_B_SPLINE_SURFACE ( (
 ( 1.000000000000000000, 1.000000000000000000),
 ( 0.9593753223639863714, 0.9995975284513187731),
 ( 0.9593753223639863714, 0.9995975284513187731),
 ( 1.000000000000000000, 1.000000000000000000) ) ) 
 REPRESENTATION_ITEM ( '' )  SURFACE ( )  );
#28313 = CARTESIAN_POINT ( 'NONE',  ( -1.046936909428679785, 37.78538189376546086, 25.87632113675119427 ) ) ;
#28314 = DIRECTION ( 'NONE',  ( 0.000000000000000000, 5.223019709707975211E-21, -1.000000000000000000 ) ) ;
#28315 = CARTESIAN_POINT ( 'NONE',  ( -1.044556982611275053, -45.76404732357875815, 1.643392503293194862 ) ) ;
#28316 = CARTESIAN_POINT ( 'NONE',  ( 1.833206310202324385, -138.2356391007179752, -44.13245377365773692 ) ) ;
#28317 = FACE_BOUND ( 'NONE', #7435, .T. ) ;
#28318 = CARTESIAN_POINT ( 'NONE',  ( -1.050230346682677007, -0.0006945978172492803249, 45.79907861045643358 ) ) ;
#28319 = B_SPLINE_CURVE_WITH_KNOTS ( 'NONE', 3,
 ( #1013, #7797, #12240, #2888, #9806, #5032 ),
 .UNSPECIFIED., .F., .F.,
 ( 4, 2, 4 ),
 ( 0.000000000000000000, 0.0004335151646191517374, 0.0008670303292383034748 ),
 .UNSPECIFIED. ) ;
#28320 = CARTESIAN_POINT ( 'NONE',  ( 6.224689322667647851, -100.9623537450644335, -108.2965163446084631 ) ) ;
#28321 = EDGE_CURVE ( 'NONE', #16924, #20693, #8264, .T. ) ;
#28322 = CARTESIAN_POINT ( 'NONE',  ( 26.11404676487259024, -67.46175819463304890, -90.92995828888270182 ) ) ;
#28323 = CARTESIAN_POINT ( 'NONE',  ( 109.1624594426973118, 0.01216903288310962859, 0.01033277910989008688 ) ) ;
#28324 = ORIENTED_EDGE ( 'NONE', *, *, #7553, .F. ) ;
#28325 = EDGE_CURVE ( 'NONE', #17556, #11003, #2423, .T. ) ;
#28326 = VERTEX_POINT ( 'NONE', #26029 ) ;
#28327 = CARTESIAN_POINT ( 'NONE',  ( -25.21435515916043713, -15.02493970636168896, -31.17620025257581062 ) ) ;
#28328 = CARTESIAN_POINT ( 'NONE',  ( -1.619063947482197729, 16.67502769180622835, 43.26576862488415287 ) ) ;
#28329 = CARTESIAN_POINT ( 'NONE',  ( 109.1586059443104944, 0.003774052605959034648, -0.005983234375919689943 ) ) ;
#28330 = CARTESIAN_POINT ( 'NONE',  ( 109.1587776205901577, -0.0006832286435102948811, -0.007297420966928593392 ) ) ;
#28331 = CARTESIAN_POINT ( 'NONE',  ( -1.019300379054419947, -25.26451264419671361, -38.21680004809154241 ) ) ;
#28332 = CARTESIAN_POINT ( 'NONE',  ( -55.25297051322618813, 0.01019003092403740832, -0.01093108995495187946 ) ) ;
#28333 = CARTESIAN_POINT ( 'NONE',  ( -1.048172774974286847, 26.08722459372787128, -37.64158596421222569 ) ) ;
#28334 = VERTEX_POINT ( 'NONE', #6050 ) ;
#28335 = CARTESIAN_POINT ( 'NONE',  ( 32.73300124599735739, 3.836798148478847370, 117.5726003567930178 ) ) ;
#28336 = CARTESIAN_POINT ( 'NONE',  ( 109.1592201516379674, -0.006536841731962029015, -0.004368284148525239038 ) ) ;
#28337 = CARTESIAN_POINT ( 'NONE',  ( 25.64692232868537758, 23.15582834340436946, -110.5112661748242857 ) ) ;
#28338 = FACE_OUTER_BOUND ( 'NONE', #17055, .T. ) ;
#28339 = ORIENTED_EDGE ( 'NONE', *, *, #9945, .F. ) ;
#28340 = CARTESIAN_POINT ( 'NONE',  ( 1.833206310202334821, -45.54896489827059014, -137.7753867363982181 ) ) ;
#28341 = ORIENTED_EDGE ( 'NONE', *, *, #22568, .F. ) ;
#28342 = ORIENTED_EDGE ( 'NONE', *, *, #12510, .T. ) ;
#28343 = ORIENTED_EDGE ( 'NONE', *, *, #14912, .T. ) ;
#28344 = B_SPLINE_CURVE_WITH_KNOTS ( 'NONE', 3,
 ( #18928, #14597, #8013, #16777, #25559, #5837, #932, #28359, #1886, #9085 ),
 .UNSPECIFIED., .F., .F.,
 ( 4, 3, 3, 4 ),
 ( 0.000000000000000000, 0.0002669560319015731767, 0.0005492286108966727871, 0.0008315040496093689670 ),
 .UNSPECIFIED. ) ;
#28345 = CARTESIAN_POINT ( 'NONE',  ( -20.37983603106074426, -18.69865230096510444, 23.16947629293382960 ) ) ;
#28346 = CARTESIAN_POINT ( 'NONE',  ( 109.1721716018069515, -0.006757465437533647160, -0.01567407524361267776 ) ) ;
#28347 = CARTESIAN_POINT ( 'NONE',  ( -55.24340739397742084, -0.009842732675351817742, 0.002421372372454084262 ) ) ;
#28348 =( BOUNDED_SURFACE ( )  B_SPLINE_SURFACE ( 3, 1, ( 
 ( #7355, #3175 ),
 ( #18418, #27489 ),
 ( #13962, #583 ),
 ( #26912, #20296 ) ),
 .UNSPECIFIED., .F., .F., .F. ) 
 B_SPLINE_SURFACE_WITH_KNOTS ( ( 4, 4 ),
 ( 2, 2 ),
 ( 0.000000000000000000, 1.000000000000000000 ),
 ( 0.000000000000000000, 1.000000000000000000 ),
 .UNSPECIFIED. ) 
 GEOMETRIC_REPRESENTATION_ITEM ( )  RATIONAL_B_SPLINE_SURFACE ( (
 ( 1.000000000000000000, 1.000000000000000000),
 ( 0.9934239774497837239, 0.8357310067453919133),
 ( 0.9934239774497837239, 0.8357310067453919133),
 ( 1.000000000000000000, 1.000000000000000000) ) ) 
 REPRESENTATION_ITEM ( '' )  SURFACE ( )  );
#28349 = EDGE_CURVE ( 'NONE', #5993, #24848, #19570, .T. ) ;
#28350 = EDGE_CURVE ( 'NONE', #18844, #13567, #10635, .T. ) ;
#28351 = CARTESIAN_POINT ( 'NONE',  ( -9.156249394959706578, -38.89149400288433611, -38.17928057391977603 ) ) ;
#28352 = B_SPLINE_CURVE_WITH_KNOTS ( 'NONE', 3,
 ( #27982, #1919, #23971, #19076, #23832, #13008, #28391, #17042 ),
 .UNSPECIFIED., .F., .F.,
 ( 4, 2, 2, 4 ),
 ( 7.757919228897728493E-18, 0.0002429592666046677342, 0.0004859185332093277163, 0.0009718370664186610705 ),
 .UNSPECIFIED. ) ;
#28353 = CARTESIAN_POINT ( 'NONE',  ( 28.37603512858355614, 112.5845402829049249, 22.09615328858486905 ) ) ;
#28354 = ORIENTED_EDGE ( 'NONE', *, *, #13482, .F. ) ;
#28355 = EDGE_CURVE ( 'NONE', #26070, #23363, #20939, .T. ) ;
#28356 = CARTESIAN_POINT ( 'NONE',  ( -1.048172774974286403, -43.86067135048628529, -13.17853518375281041 ) ) ;
#28357 = CARTESIAN_POINT ( 'NONE',  ( -55.24271866751342941, -0.004365563123939053720, 0.008433070970613821063 ) ) ;
#28358 = LINE ( 'NONE', #15537, #28051 ) ;
#28359 = CARTESIAN_POINT ( 'NONE',  ( 25.64700659047695197, 56.25842064176090673, 97.89757946487027596 ) ) ;
#28360 = EDGE_CURVE ( 'NONE', #23301, #15242, #27905, .T. ) ;
#28361 = CARTESIAN_POINT ( 'NONE',  ( -55.24271866751342941, -0.009388511352197387999, -0.001425019990782294558 ) ) ;
#28362 = CARTESIAN_POINT ( 'NONE',  ( -1.323439229708142983, -35.86372896917450959, 28.92147054731879408 ) ) ;
#28363 = CARTESIAN_POINT ( 'NONE',  ( 109.1586900883932856, 0.001385221016536850079, 0.007002774699553664800 ) ) ;
#28364 = CARTESIAN_POINT ( 'NONE',  ( -20.24399999263415140, -10.36954246768226717, 27.76448601145551009 ) ) ;
#28365 = B_SPLINE_CURVE_WITH_KNOTS ( 'NONE', 3,
 ( #9372, #22765, #18127, #7215, #7347, #18259, #24778 ),
 .UNSPECIFIED., .F., .F.,
 ( 4, 3, 4 ),
 ( 0.000000000000000000, 0.006568092053401836973, 0.02506242213020846987 ),
 .UNSPECIFIED. ) ;
#28366 = EDGE_LOOP ( 'NONE', ( #6373, #15123, #24084, #1623 ) ) ;
#28367 = ORIENTED_EDGE ( 'NONE', *, *, #16429, .T. ) ;
#28368 = CARTESIAN_POINT ( 'NONE',  ( 8.186469777910739154, 77.65916160569911142, 127.5731248346290414 ) ) ;
#28369 = CARTESIAN_POINT ( 'NONE',  ( 1.833485406944043827, -138.1714136985311256, 44.33323125129879116 ) ) ;
#28370 = ORIENTED_EDGE ( 'NONE', *, *, #17307, .T. ) ;
#28371 = ORIENTED_EDGE ( 'NONE', *, *, #9559, .T. ) ;
#28372 = ORIENTED_EDGE ( 'NONE', *, *, #6076, .F. ) ;
#28373 = B_SPLINE_CURVE_WITH_KNOTS ( 'NONE', 3,
 ( #27612, #26022, #8332, #21133, #25622, #16693, #4136, #10492 ),
 .UNSPECIFIED., .F., .F.,
 ( 4, 2, 2, 4 ),
 ( 0.000000000000000000, 0.002761524886576655416, 0.005523049773153310832, 0.01104609954630662166 ),
 .UNSPECIFIED. ) ;
#28374 = CARTESIAN_POINT ( 'NONE',  ( 2.430230287190589422, -138.8342928068217077, -43.58368230469532278 ) ) ;
#28375 = EDGE_CURVE ( 'NONE', #25436, #6634, #21707, .T. ) ;
#28376 = EDGE_CURVE ( 'NONE', #8934, #26396, #13382, .T. ) ;
#28377 = CARTESIAN_POINT ( 'NONE',  ( 6.224689322667647851, 121.2721959030538130, 84.93872395423015575 ) ) ;
#28378 = B_SPLINE_CURVE_WITH_KNOTS ( 'NONE', 3,
 ( #13276, #10855, #22061, #10717, #11133, #19617, #28247 ),
 .UNSPECIFIED., .F., .F.,
 ( 4, 3, 4 ),
 ( 2.299948302575412283E-16, 0.009512539173626367167, 0.02506242213020821313 ),
 .UNSPECIFIED. ) ;
#28379 = CARTESIAN_POINT ( 'NONE',  ( -1.049819825607592794, 43.71263398674771139, 13.66706894614392986 ) ) ;
#28380 = EDGE_CURVE ( 'NONE', #16927, #13485, #14420, .T. ) ;
#28381 = FACE_OUTER_BOUND ( 'NONE', #10093, .T. ) ;
#28382 = CARTESIAN_POINT ( 'NONE',  ( 94.22246935314088034, -151.1871800109700246, -12.50000000000000888 ) ) ;
#28383 = CARTESIAN_POINT ( 'NONE',  ( 13.36082413113063083, -151.2941478187909468, 22.28175172543511096 ) ) ;
#28384 =( BOUNDED_SURFACE ( )  B_SPLINE_SURFACE ( 3, 1, ( 
 ( #24677, #6676 ),
 ( #184, #2322 ),
 ( #24529, #13697 ),
 ( #11268, #4490 ) ),
 .UNSPECIFIED., .F., .F., .F. ) 
 B_SPLINE_SURFACE_WITH_KNOTS ( ( 4, 4 ),
 ( 2, 2 ),
 ( 0.000000000000000000, 1.000000000000000000 ),
 ( 0.000000000000000000, 1.000000000000000000 ),
 .UNSPECIFIED. ) 
 GEOMETRIC_REPRESENTATION_ITEM ( )  RATIONAL_B_SPLINE_SURFACE ( (
 ( 1.000000000000000000, 1.000000000000000000),
 ( 0.9956975270656954757, 0.8568959468854893125),
 ( 0.9956975270656954757, 0.8568959468854893125),
 ( 1.000000000000000000, 1.000000000000000000) ) ) 
 REPRESENTATION_ITEM ( '' )  SURFACE ( )  );
#28385 = CARTESIAN_POINT ( 'NONE',  ( -20.57838717382308147, -29.92853265176830746, 1.611677988432673070 ) ) ;
#28386 = LINE ( 'NONE', #13139, #6005 ) ;
#28387 = PLANE ( 'NONE',  #22463 ) ;
#28388 = EDGE_LOOP ( 'NONE', ( #15082, #23646, #19321, #8512 ) ) ;
#28389 = ORIENTED_EDGE ( 'NONE', *, *, #3223, .F. ) ;
#28390 = CARTESIAN_POINT ( 'NONE',  ( -55.24271866751342941, -0.009388511352199774979, 0.001425019990778933097 ) ) ;
#28391 = CARTESIAN_POINT ( 'NONE',  ( 25.64660436782557440, 22.90783756891005396, -110.5628080555243713 ) ) ;
#28392 = B_SPLINE_CURVE_WITH_KNOTS ( 'NONE', 3,
 ( #26957, #24973, #636, #18036, #3084, #9557, #6837, #15581 ),
 .UNSPECIFIED., .F., .F.,
 ( 4, 2, 2, 4 ),
 ( 1.734723475976807094E-18, 0.0002429588503611205359, 0.0004859177007222393371, 0.0009718354014444821436 ),
 .UNSPECIFIED. ) ;
#28393 = CARTESIAN_POINT ( 'NONE',  ( -8.786685647604896232, 9.545808661481343549, 52.67761315067276229 ) ) ;
#28394 = CARTESIAN_POINT ( 'NONE',  ( -1.463510566862828766, -43.13857742234517190, -16.57250862017402682 ) ) ;
#28395 = LINE ( 'NONE', #4228, #22466 ) ;
#28396 = ORIENTED_EDGE ( 'NONE', *, *, #23236, .T. ) ;
#28397 = CARTESIAN_POINT ( 'NONE',  ( -9.156249394959706578, 38.17928057391991103, -38.89149400288420111 ) ) ;
#28398 = CARTESIAN_POINT ( 'NONE',  ( 16.75465622695635659, 98.56308464785224999, -102.5353941815395160 ) ) ;
#28399 = CARTESIAN_POINT ( 'NONE',  ( -20.57838717382308502, 23.26537097894105699, -18.89542499756508320 ) ) ;
#28400 = ORIENTED_EDGE ( 'NONE', *, *, #8839, .F. ) ;
#28401 = ORIENTED_EDGE ( 'NONE', *, *, #23260, .T. ) ;
#28402 = CARTESIAN_POINT ( 'NONE',  ( -1.463510566862834761, -16.57250862017389892, 43.13857742234520032 ) ) ;
#28403 = VERTEX_POINT ( 'NONE', #17375 ) ;
#28404 = CARTESIAN_POINT ( 'NONE',  ( 1.831572820252009626, 117.9752562883666940, 84.49389457294174122 ) ) ;
#28405 = ORIENTED_EDGE ( 'NONE', *, *, #18952, .T. ) ;
#28406 = AXIS2_PLACEMENT_3D ( 'NONE', #18822, #3004, #3428 ) ;
#28407 = CARTESIAN_POINT ( 'NONE',  ( 26.04756280548353686, 67.42001818240466093, 90.90573670389261451 ) ) ;
#28408 = ORIENTED_EDGE ( 'NONE', *, *, #23817, .F. ) ;
#28409 = B_SPLINE_CURVE_WITH_KNOTS ( 'NONE', 3,
 ( #21421, #10494, #12909, #17369, #28170, #19133 ),
 .UNSPECIFIED., .F., .F.,
 ( 4, 2, 4 ),
 ( 3.476216610979977084E-18, 0.0006311571484586040543, 0.001262314296917204422 ),
 .UNSPECIFIED. ) ;
#28410 = EDGE_CURVE ( 'NONE', #15835, #19755, #3107, .T. ) ;
#28411 = CARTESIAN_POINT ( 'NONE',  ( 13.36082413113061307, -22.28175172543663507, 151.2941478187906910 ) ) ;
#28412 = CARTESIAN_POINT ( 'NONE',  ( 2.433796855181219243, 31.67151202413165478, -142.0211193075552956 ) ) ;
#28413 = EDGE_CURVE ( 'NONE', #21724, #414, #15297, .T. ) ;
#28414 = CARTESIAN_POINT ( 'NONE',  ( 109.1592201516379674, 0.006957642258155071965, 0.003661068210032695190 ) ) ;
#28415 = CARTESIAN_POINT ( 'NONE',  ( 1.833485406944043827, 144.2578170162065021, -15.69895494453236395 ) ) ;
#28416 = CARTESIAN_POINT ( 'NONE',  ( 30.59141879584289825, -113.0806649571964755, -26.79785525806519786 ) ) ;
#28417 = EDGE_CURVE ( 'NONE', #13229, #10864, #26798, .T. ) ;
#28418 = CARTESIAN_POINT ( 'NONE',  ( 1.833809397773856542, 125.5796696653637952, 72.70895493223410710 ) ) ;
#28420 = CARTESIAN_POINT ( 'NONE',  ( 1.833206308920055205, -117.8322276971141491, 84.68961866582966991 ) ) ;
#28419 = LINE ( 'NONE', #504, #12970 ) ;
#28421 = CARTESIAN_POINT ( 'NONE',  ( 25.69398547355841700, -112.2438548322123353, 12.54367966928010425 ) ) ;
#28422 =( BOUNDED_SURFACE ( )  B_SPLINE_SURFACE ( 3, 1, ( 
 ( #7230, #13826 ),
 ( #16426, #3327 ),
 ( #11825, #24931 ),
 ( #5045, #22633 ) ),
 .UNSPECIFIED., .F., .F., .F. ) 
 B_SPLINE_SURFACE_WITH_KNOTS ( ( 4, 4 ),
 ( 2, 2 ),
 ( 0.000000000000000000, 1.000000000000000000 ),
 ( 0.000000000000000000, 1.000000000000000000 ),
 .UNSPECIFIED. ) 
 GEOMETRIC_REPRESENTATION_ITEM ( )  RATIONAL_B_SPLINE_SURFACE ( (
 ( 1.000000000000000000, 1.000000000000000000),
 ( 0.9593753223639863714, 0.9995975284513187731),
 ( 0.9593753223639863714, 0.9995975284513187731),
 ( 1.000000000000000000, 1.000000000000000000) ) ) 
 REPRESENTATION_ITEM ( '' )  SURFACE ( )  );
#28423 = ORIENTED_EDGE ( 'NONE', *, *, #7236, .T. ) ;
#28424 = CARTESIAN_POINT ( 'NONE',  ( 25.64708010899962787, 56.40825696968397551, -97.81137751680941506 ) ) ;
#28425 = B_SPLINE_CURVE_WITH_KNOTS ( 'NONE', 3,
 ( #27290, #10335, #16357, #23150, #20955, #19094 ),
 .UNSPECIFIED., .F., .F.,
 ( 4, 2, 4 ),
 ( 1.734723475976807094E-18, 0.0004335184443140231605, 0.0008670368886280445863 ),
 .UNSPECIFIED. ) ;
#28426 = CARTESIAN_POINT ( 'NONE',  ( 1.833485406944057594, -72.09189602597798796, 125.9346397303433065 ) ) ;
#28427 = CARTESIAN_POINT ( 'NONE',  ( -1.050230346682680560, -26.92058491724839797, 37.05182464822011923 ) ) ;
#28428 = CARTESIAN_POINT ( 'NONE',  ( -1.048171036023499925, -43.86077206077059998, 13.17819047681649103 ) ) ;
#28429 = CARTESIAN_POINT ( 'NONE',  ( 25.86096068574580897, 97.40497849554891729, 57.38862431273619791 ) ) ;
#28430 = CARTESIAN_POINT ( 'NONE',  ( 1.833838850093517214, 1.355257560975019971E-17, -145.1097630783160923 ) ) ;
#28431 = ORIENTED_EDGE ( 'NONE', *, *, #21484, .T. ) ;
#28432 = CARTESIAN_POINT ( 'NONE',  ( 1.832998868059858122, 58.53348008137646019, 132.7810136645740045 ) ) ;
#28433 = CARTESIAN_POINT ( 'NONE',  ( -20.20700224038492721, -23.35150625415671755, -18.19058640100215385 ) ) ;
#28434 = CARTESIAN_POINT ( 'NONE',  ( 2.433796855181205476, 109.1007109081238724, -96.28145139437575040 ) ) ;
#28435 = ORIENTED_EDGE ( 'NONE', *, *, #9034, .F. ) ;
#28436 = CARTESIAN_POINT ( 'NONE',  ( -55.24728320129491266, -0.01362040845703012606, 0.005114031043466422087 ) ) ;
#28437 = CARTESIAN_POINT ( 'NONE',  ( 1.833485406944043827, 15.69895494453577101, -144.2578170162061326 ) ) ;
#28438 = CARTESIAN_POINT ( 'NONE',  ( 10.93730112725932635, 0.000000000000000000, 0.000000000000000000 ) ) ;
#28439 = PRODUCT_DEFINITION ( 'UNKNOWN', '', #13478, #18602 ) ;
#28440 = ORIENTED_EDGE ( 'NONE', *, *, #9070, .F. ) ;
#28441 = CARTESIAN_POINT ( 'NONE',  ( 25.64692232868534560, -112.9106972861223426, 0.3267662677147551431 ) ) ;
#28442 = ORIENTED_EDGE ( 'NONE', *, *, #10878, .F. ) ;
#28443 = CARTESIAN_POINT ( 'NONE',  ( -1.463510566862834983, -35.90603835816524025, -29.09194585123821497 ) ) ;
#28444 = EDGE_CURVE ( 'NONE', #28093, #25271, #7247, .T. ) ;
#28445 = EDGE_LOOP ( 'NONE', ( #17169, #9607, #1448, #20223 ) ) ;
#28446 = CARTESIAN_POINT ( 'NONE',  ( -20.57838717382308147, -7.715628353033886278, -28.96176188950215646 ) ) ;
#28447 = DIRECTION ( 'NONE',  ( 1.000000000000000000, -6.938893903907226837E-18, 1.734723475976806709E-18 ) ) ;
#28448 = CARTESIAN_POINT ( 'NONE',  ( 55.79472521941428198, 54.55111121764083748, 48.13855120843901858 ) ) ;
#28449 = CARTESIAN_POINT ( 'NONE',  ( 1.833485406944057594, -138.1714136985305572, -44.33323125130066700 ) ) ;
#28450 = CARTESIAN_POINT ( 'NONE',  ( 28.37644542392847313, -89.64009552702840722, -86.16884085958031392 ) ) ;
#28451 = CARTESIAN_POINT ( 'NONE',  ( 13.36082413113063083, -148.1362653801005251, 37.97423473099245683 ) ) ;
#28452 = CARTESIAN_POINT ( 'NONE',  ( 2.430230287190589422, 46.34481016236826179, 137.9371479820464117 ) ) ;
#28453 = CARTESIAN_POINT ( 'NONE',  ( 109.1721716018069657, -0.01127028715940094246, 0.01281875973824537183 ) ) ;
#28454 = CARTESIAN_POINT ( 'NONE',  ( 2.430230287190572103, -1.451610819318766232, 145.5073573687466819 ) ) ;
#28455 = CARTESIAN_POINT ( 'NONE',  ( -8.786685647604896232, 23.24040270374459993, 48.22796981442743913 ) ) ;
#28456 = VERTEX_POINT ( 'NONE', #4558 ) ;
#28457 = ORIENTED_EDGE ( 'NONE', *, *, #1208, .F. ) ;
#28458 = EDGE_LOOP ( 'NONE', ( #23810, #27390, #204, #19296 ) ) ;
#28459 = CARTESIAN_POINT ( 'NONE',  ( -1.046935749539998906, -43.93230528057173956, 12.93334586714225054 ) ) ;
#28460 = CARTESIAN_POINT ( 'NONE',  ( -20.20612091757422490, -28.48192249925583752, 8.058516044219494745 ) ) ;
#28461 = CARTESIAN_POINT ( 'NONE',  ( 119.2224693531408803, -69.99999999999998579, -20.00000000000000355 ) ) ;
#28462 = CARTESIAN_POINT ( 'NONE',  ( -2.265401668238148591, -46.93990709177548837, -2.645701981445641504 ) ) ;
#28463 = LINE ( 'NONE', #7193, #28201 ) ;
#28464 = CARTESIAN_POINT ( 'NONE',  ( -25.21435515916043357, -25.00736669481038987, -23.92354251275926558 ) ) ;
#28465 = EDGE_LOOP ( 'NONE', ( #1754, #19977, #13946, #15607 ) ) ;
#28466 = CARTESIAN_POINT ( 'NONE',  ( 30.59138290137877902, 38.47117663195945880, 109.6600423140541523 ) ) ;
#28467 = CARTESIAN_POINT ( 'NONE',  ( -55.25719721206881729, -0.006045473558784038998, 0.009391134844733136505 ) ) ;
#28468 = CARTESIAN_POINT ( 'NONE',  ( 1.833485406944043827, 117.7091014914961420, -84.86072343962446496 ) ) ;
#28469 = CARTESIAN_POINT ( 'NONE',  ( -1.031422197589716205, -37.93675465142454328, 25.67058493451484225 ) ) ;
#28470 =( BOUNDED_SURFACE ( )  B_SPLINE_SURFACE ( 3, 1, ( 
 ( #18639, #27411 ),
 ( #7721, #15009 ),
 ( #10716, #19203 ),
 ( #21498, #2051 ) ),
 .UNSPECIFIED., .F., .F., .F. ) 
 B_SPLINE_SURFACE_WITH_KNOTS ( ( 4, 4 ),
 ( 2, 2 ),
 ( 0.000000000000000000, 1.000000000000000000 ),
 ( 0.000000000000000000, 1.000000000000000000 ),
 .UNSPECIFIED. ) 
 GEOMETRIC_REPRESENTATION_ITEM ( )  RATIONAL_B_SPLINE_SURFACE ( (
 ( 1.000000000000000000, 1.000000000000000000),
 ( 0.6386103224230302855, 0.9954351624131538845),
 ( 0.6386103224230302855, 0.9954351624131538845),
 ( 1.000000000000000000, 1.000000000000000000) ) ) 
 REPRESENTATION_ITEM ( '' )  SURFACE ( )  );
#28471 = CARTESIAN_POINT ( 'NONE',  ( 25.65782528836481191, 12.37768345530126091, -112.2379831684171307 ) ) ;
#28472 = CARTESIAN_POINT ( 'NONE',  ( 109.1624594426973260, -0.001206615835671285284, -0.01591840958352308891 ) ) ;
#28473 = ORIENTED_EDGE ( 'NONE', *, *, #11019, .F. ) ;
#28474 = CARTESIAN_POINT ( 'NONE',  ( 28.43349137099829349, 8.951033805646366304, -123.9292945876798200 ) ) ;
#28475 = CARTESIAN_POINT ( 'NONE',  ( 1.833750490713712322, -117.2391074582366883, -85.50916867388922071 ) ) ;
#28476 = ORIENTED_EDGE ( 'NONE', *, *, #23918, .F. ) ;
#28477 =( BOUNDED_SURFACE ( )  B_SPLINE_SURFACE ( 3, 1, ( 
 ( #7125, #18171 ),
 ( #478, #18030 ),
 ( #11713, #3211 ),
 ( #22667, #5227 ) ),
 .UNSPECIFIED., .F., .F., .F. ) 
 B_SPLINE_SURFACE_WITH_KNOTS ( ( 4, 4 ),
 ( 2, 2 ),
 ( 0.000000000000000000, 1.000000000000000000 ),
 ( 0.000000000000000000, 1.000000000000000000 ),
 .UNSPECIFIED. ) 
 GEOMETRIC_REPRESENTATION_ITEM ( )  RATIONAL_B_SPLINE_SURFACE ( (
 ( 1.000000000000000000, 1.000000000000000000),
 ( 0.6386103224230302855, 0.9954351624131538845),
 ( 0.6386103224230302855, 0.9954351624131538845),
 ( 1.000000000000000000, 1.000000000000000000) ) ) 
 REPRESENTATION_ITEM ( '' )  SURFACE ( )  );
#28478 = VERTEX_POINT ( 'NONE', #7173 ) ;
#28479 = ADVANCED_FACE ( 'NONE', ( #13330 ), #152, .F. ) ;
#28480 = VERTEX_POINT ( 'NONE', #20100 ) ;
#28481 = CARTESIAN_POINT ( 'NONE',  ( 2.433796855181233454, 142.6247129145648387, 28.83182736670586266 ) ) ;
#28482 = NEXT_ASSEMBLY_USAGE_OCCURRENCE ( 'NAUO1', ' ', ' ', #9653, #23390, $ ) ;
#28483 = NEXT_ASSEMBLY_USAGE_OCCURRENCE ( 'NAUO2', ' ', ' ', #9653, #28439, $ ) ;
#28484 = NEXT_ASSEMBLY_USAGE_OCCURRENCE ( 'NAUO3', ' ', ' ', #9653, #25506, $ ) ;
#28485 = NEXT_ASSEMBLY_USAGE_OCCURRENCE ( 'NAUO4', ' ', ' ', #9653, #25506, $ ) ;
#28486 = NEXT_ASSEMBLY_USAGE_OCCURRENCE ( 'NAUO5', ' ', ' ', #9653, #28439, $ ) ;
#28487=COLOUR_RGB('Dark Blue',0.08,0.2,0.34);
#28488=FILL_AREA_STYLE_COLOUR('',#28487);
#28489=FILL_AREA_STYLE('',(#28488));
#28490=SURFACE_STYLE_FILL_AREA(#28489);
#28491=SURFACE_SIDE_STYLE('',(#28490));
#28492=SURFACE_STYLE_USAGE(.BOTH.,#28491);
#28493=PRESENTATION_STYLE_ASSIGNMENT((#28492));
#28494=COLOUR_RGB('Light Blue',0.38,0.62,0.78);
#28495=FILL_AREA_STYLE_COLOUR('',#28494);
#28496=FILL_AREA_STYLE('',(#28495));
#28497=SURFACE_STYLE_FILL_AREA(#28496);
#28498=SURFACE_SIDE_STYLE('',(#28497));
#28499=SURFACE_STYLE_USAGE(.BOTH.,#28498);
#28500=PRESENTATION_STYLE_ASSIGNMENT((#28499));
#28501=COLOUR_RGB('Sky Blue',0.24,0.69,0.87);
#28502=FILL_AREA_STYLE_COLOUR('',#28501);
#28503=FILL_AREA_STYLE('',(#28502));
#28504=SURFACE_STYLE_FILL_AREA(#28503);
#28505=SURFACE_SIDE_STYLE('',(#28504));
#28506=SURFACE_STYLE_USAGE(.BOTH.,#28505);
#28507=PRESENTATION_STYLE_ASSIGNMENT((#28506));
#28508=COLOUR_RGB('Grey',0.48,0.52,0.57);
#28509=FILL_AREA_STYLE_COLOUR('',#28508);
#28510=FILL_AREA_STYLE('',(#28509));
#28511=SURFACE_STYLE_FILL_AREA(#28510);
#28512=SURFACE_SIDE_STYLE('',(#28511));
#28513=SURFACE_STYLE_USAGE(.BOTH.,#28512);
#28514=PRESENTATION_STYLE_ASSIGNMENT((#28513));
#28515=COLOUR_RGB('Black',0.12,0.14,0.17);
#28516=FILL_AREA_STYLE_COLOUR('',#28515);
#28517=FILL_AREA_STYLE('',(#28516));
#28518=SURFACE_STYLE_FILL_AREA(#28517);
#28519=SURFACE_SIDE_STYLE('',(#28518));
#28520=SURFACE_STYLE_USAGE(.BOTH.,#28519);
#28521=PRESENTATION_STYLE_ASSIGNMENT((#28520));
#28522=COLOUR_RGB('Off White',0.89,0.88,0.83);
#28523=FILL_AREA_STYLE_COLOUR('',#28522);
#28524=FILL_AREA_STYLE('',(#28523));
#28525=SURFACE_STYLE_FILL_AREA(#28524);
#28526=SURFACE_SIDE_STYLE('',(#28525));
#28527=SURFACE_STYLE_USAGE(.BOTH.,#28526);
#28528=PRESENTATION_STYLE_ASSIGNMENT((#28527));
ENDSEC;
END-ISO-10303-21;
